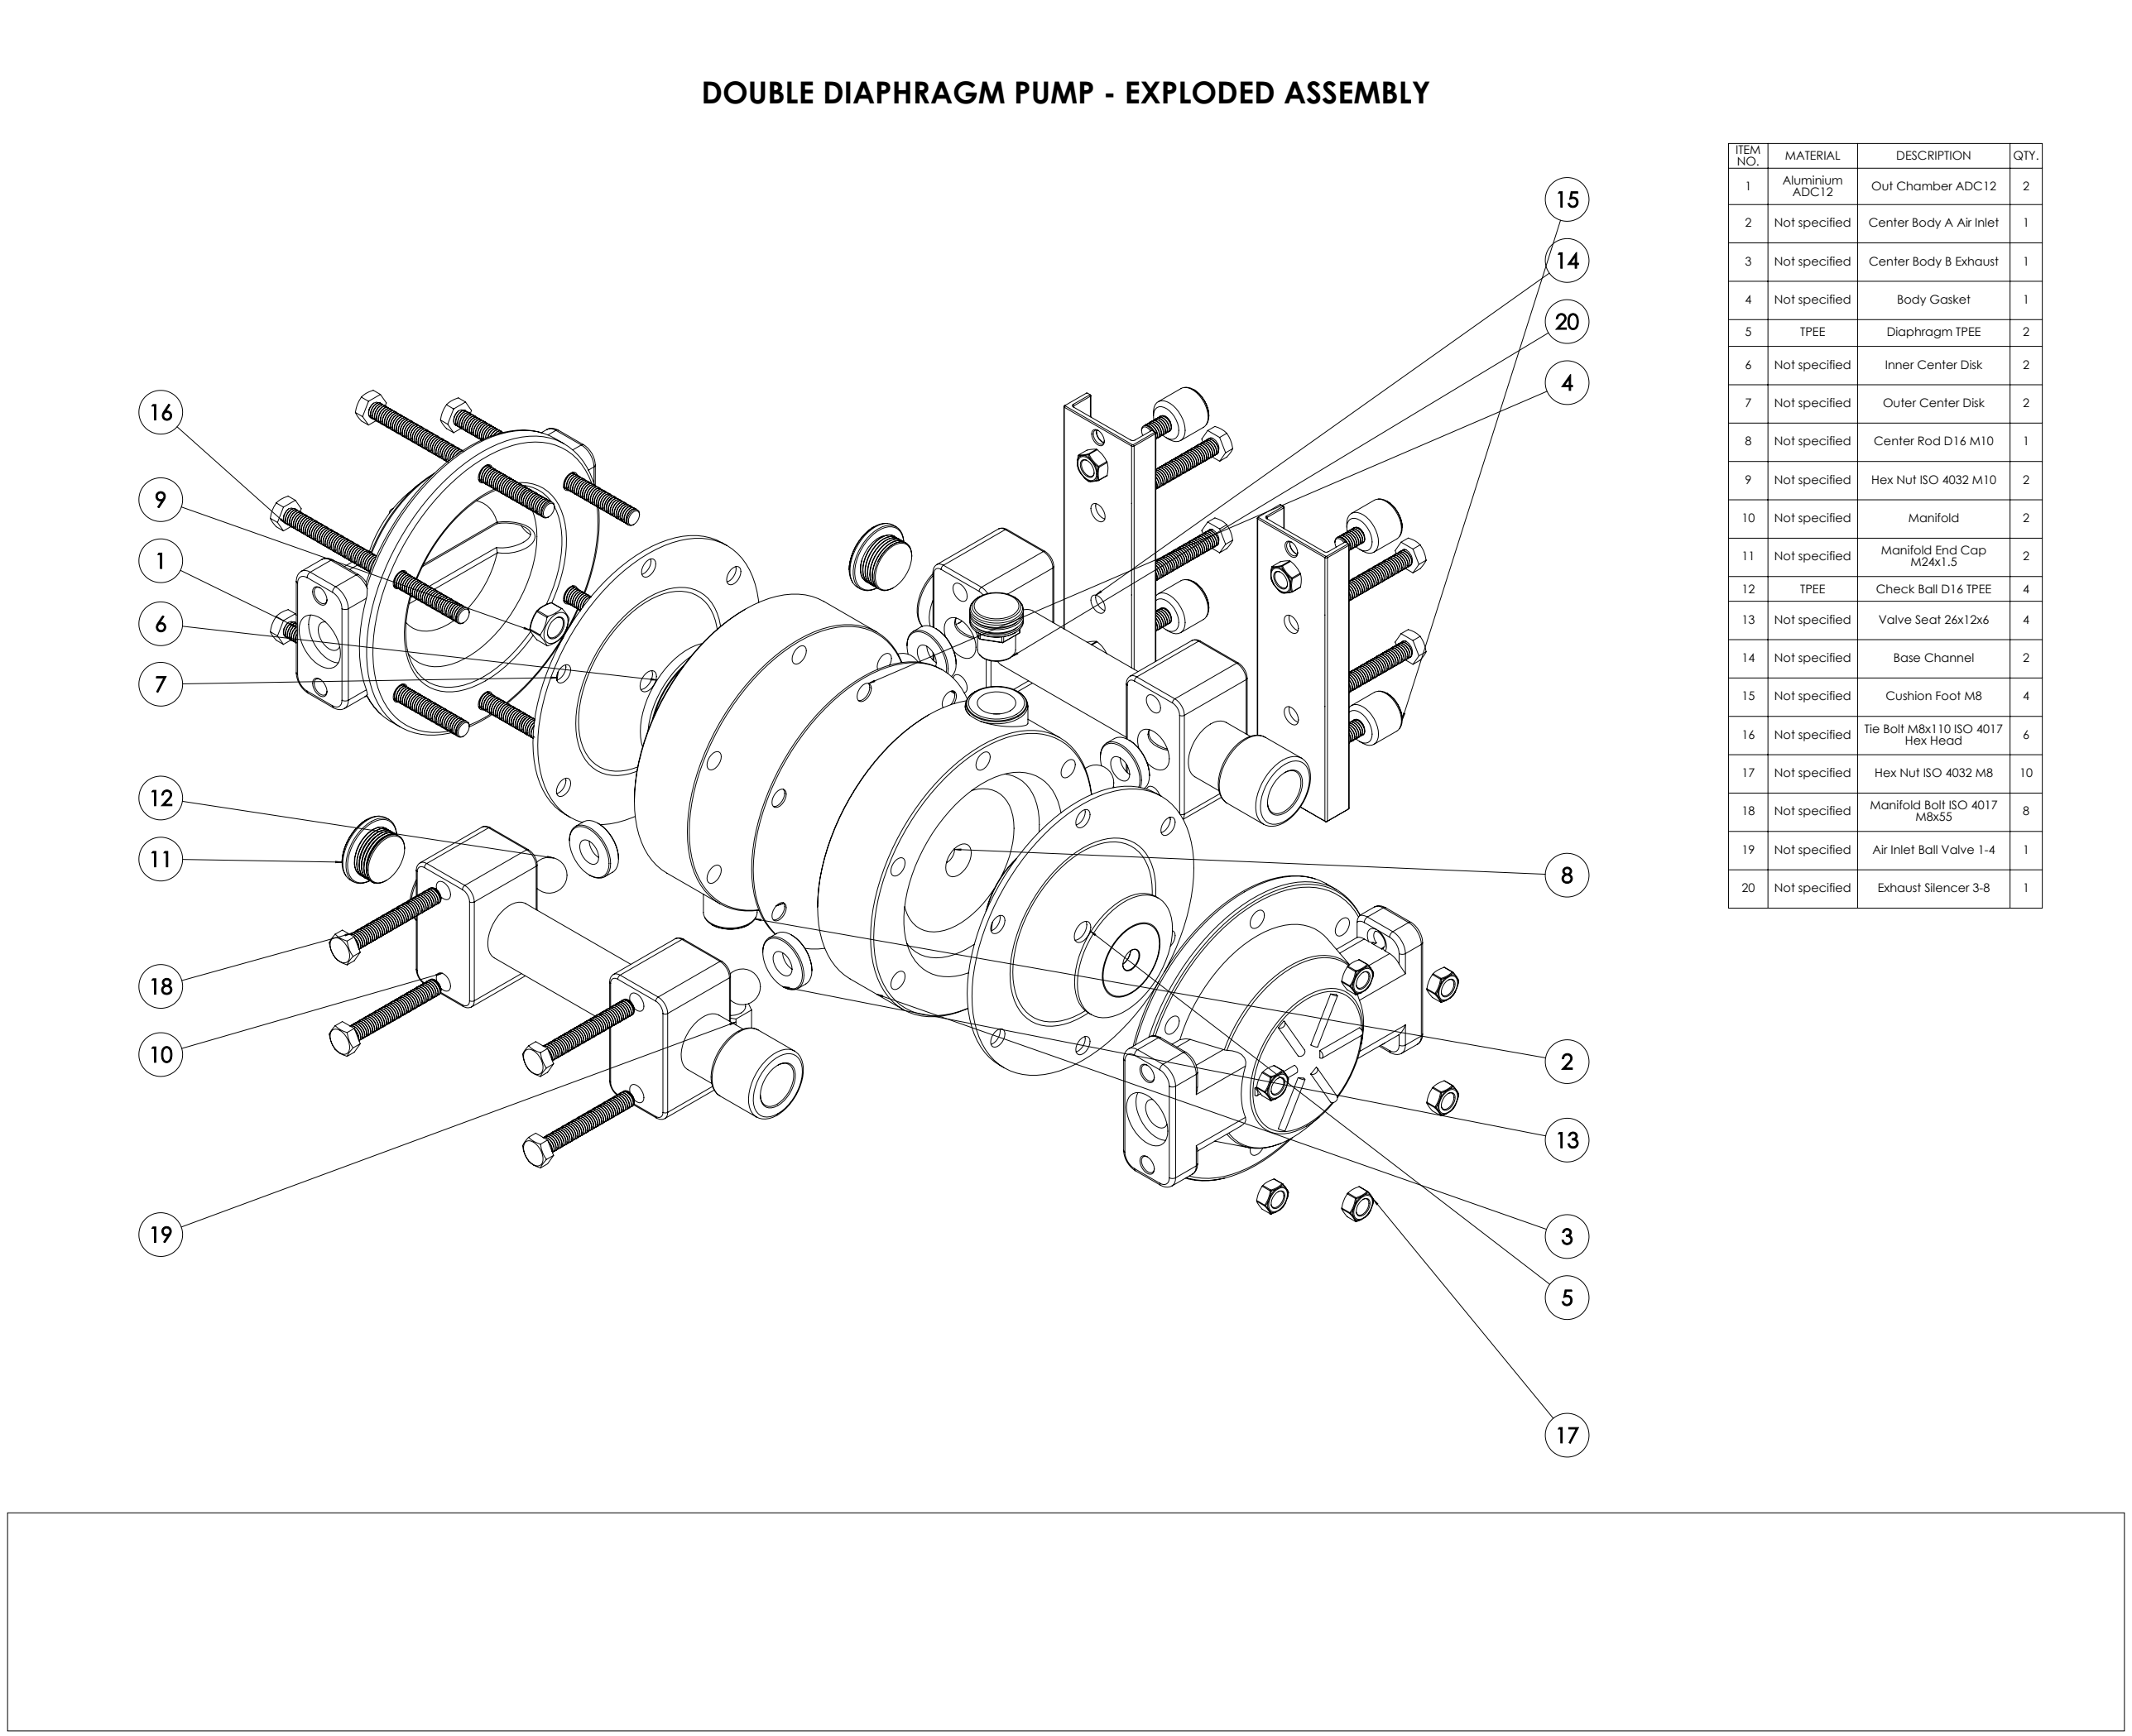
ISO-10303-21;
HEADER;
/* Generated by software containing ST-Developer
 * from STEP Tools, Inc. (www.steptools.com) 
 */

FILE_DESCRIPTION(
/* description */ (''),
/* implementation_level */ '2;1');

FILE_NAME(
/* name */ 'MAS-343',
/* time_stamp */ '2026-10-26T06:13:19-07:00',
/* author */ (''),
/* organization */ (''),
/* preprocessor_version */ 'ST-DEVELOPER v20.2',
/* originating_system */ 'Autodesk Translation Framework v15.15.0.0',
/* authorisation */ '');

FILE_SCHEMA (('AUTOMOTIVE_DESIGN { 1 0 10303 214 3 1 1 }','TECHNICAL_DATA_PACKAGING'));
ENDSEC;

DATA;
#10=MECHANICAL_DESIGN_GEOMETRIC_PRESENTATION_REPRESENTATION('',(#297,#298,
#299,#300,#301,#302,#303,#304,#305,#306,#307,#308,#309,#310,#311,#312,#313,
#314,#315,#316),#56639);
#11=ITEM_DEFINED_TRANSFORMATION($,$,#17191,#18731);
#12=ITEM_DEFINED_TRANSFORMATION($,$,#17191,#18732);
#13=ITEM_DEFINED_TRANSFORMATION($,$,#17485,#18733);
#14=ITEM_DEFINED_TRANSFORMATION($,$,#17536,#18734);
#15=ITEM_DEFINED_TRANSFORMATION($,$,#17588,#18735);
#16=ITEM_DEFINED_TRANSFORMATION($,$,#17615,#18736);
#17=ITEM_DEFINED_TRANSFORMATION($,$,#17615,#18737);
#18=ITEM_DEFINED_TRANSFORMATION($,$,#17650,#18738);
#19=ITEM_DEFINED_TRANSFORMATION($,$,#17650,#18739);
#20=ITEM_DEFINED_TRANSFORMATION($,$,#17664,#18740);
#21=ITEM_DEFINED_TRANSFORMATION($,$,#17664,#18741);
#22=ITEM_DEFINED_TRANSFORMATION($,$,#17684,#18742);
#23=ITEM_DEFINED_TRANSFORMATION($,$,#17774,#18743);
#24=ITEM_DEFINED_TRANSFORMATION($,$,#17774,#18744);
#25=ITEM_DEFINED_TRANSFORMATION($,$,#17818,#18745);
#26=ITEM_DEFINED_TRANSFORMATION($,$,#17818,#18746);
#27=ITEM_DEFINED_TRANSFORMATION($,$,#18010,#18747);
#28=ITEM_DEFINED_TRANSFORMATION($,$,#18010,#18748);
#29=ITEM_DEFINED_TRANSFORMATION($,$,#18066,#18749);
#30=ITEM_DEFINED_TRANSFORMATION($,$,#18137,#18750);
#31=ITEM_DEFINED_TRANSFORMATION($,$,#18202,#18751);
#32=ITEM_DEFINED_TRANSFORMATION($,$,#18202,#18752);
#33=ITEM_DEFINED_TRANSFORMATION($,$,#18205,#18753);
#34=ITEM_DEFINED_TRANSFORMATION($,$,#18205,#18754);
#35=ITEM_DEFINED_TRANSFORMATION($,$,#18218,#18755);
#36=ITEM_DEFINED_TRANSFORMATION($,$,#18327,#18756);
#37=ITEM_DEFINED_TRANSFORMATION($,$,#18687,#18757);
#38=ITEM_DEFINED_TRANSFORMATION($,$,#18327,#18758);
#39=ITEM_DEFINED_TRANSFORMATION($,$,#18687,#18759);
#40=ITEM_DEFINED_TRANSFORMATION($,$,#18375,#18760);
#41=ITEM_DEFINED_TRANSFORMATION($,$,#18375,#18761);
#42=ITEM_DEFINED_TRANSFORMATION($,$,#18375,#18762);
#43=ITEM_DEFINED_TRANSFORMATION($,$,#18375,#18763);
#44=ITEM_DEFINED_TRANSFORMATION($,$,#18202,#18764);
#45=ITEM_DEFINED_TRANSFORMATION($,$,#18202,#18765);
#46=ITEM_DEFINED_TRANSFORMATION($,$,#18205,#18766);
#47=ITEM_DEFINED_TRANSFORMATION($,$,#18205,#18767);
#48=ITEM_DEFINED_TRANSFORMATION($,$,#18218,#18768);
#49=ITEM_DEFINED_TRANSFORMATION($,$,#18327,#18769);
#50=ITEM_DEFINED_TRANSFORMATION($,$,#18687,#18770);
#51=ITEM_DEFINED_TRANSFORMATION($,$,#18327,#18771);
#52=ITEM_DEFINED_TRANSFORMATION($,$,#18687,#18772);
#53=ITEM_DEFINED_TRANSFORMATION($,$,#18375,#18773);
#54=ITEM_DEFINED_TRANSFORMATION($,$,#18375,#18774);
#55=ITEM_DEFINED_TRANSFORMATION($,$,#18375,#18775);
#56=ITEM_DEFINED_TRANSFORMATION($,$,#18375,#18776);
#57=ITEM_DEFINED_TRANSFORMATION($,$,#18487,#18777);
#58=ITEM_DEFINED_TRANSFORMATION($,$,#18687,#18778);
#59=ITEM_DEFINED_TRANSFORMATION($,$,#18487,#18779);
#60=ITEM_DEFINED_TRANSFORMATION($,$,#18687,#18780);
#61=ITEM_DEFINED_TRANSFORMATION($,$,#18487,#18781);
#62=ITEM_DEFINED_TRANSFORMATION($,$,#18687,#18782);
#63=ITEM_DEFINED_TRANSFORMATION($,$,#18487,#18783);
#64=ITEM_DEFINED_TRANSFORMATION($,$,#18687,#18784);
#65=ITEM_DEFINED_TRANSFORMATION($,$,#18487,#18785);
#66=ITEM_DEFINED_TRANSFORMATION($,$,#18687,#18786);
#67=ITEM_DEFINED_TRANSFORMATION($,$,#18487,#18787);
#68=ITEM_DEFINED_TRANSFORMATION($,$,#18687,#18788);
#69=(
REPRESENTATION_RELATIONSHIP($,$,#56745,#56744)
REPRESENTATION_RELATIONSHIP_WITH_TRANSFORMATION(#11)
SHAPE_REPRESENTATION_RELATIONSHIP()
);
#70=(
REPRESENTATION_RELATIONSHIP($,$,#56745,#56744)
REPRESENTATION_RELATIONSHIP_WITH_TRANSFORMATION(#12)
SHAPE_REPRESENTATION_RELATIONSHIP()
);
#71=(
REPRESENTATION_RELATIONSHIP($,$,#56746,#56744)
REPRESENTATION_RELATIONSHIP_WITH_TRANSFORMATION(#13)
SHAPE_REPRESENTATION_RELATIONSHIP()
);
#72=(
REPRESENTATION_RELATIONSHIP($,$,#56747,#56744)
REPRESENTATION_RELATIONSHIP_WITH_TRANSFORMATION(#14)
SHAPE_REPRESENTATION_RELATIONSHIP()
);
#73=(
REPRESENTATION_RELATIONSHIP($,$,#56748,#56744)
REPRESENTATION_RELATIONSHIP_WITH_TRANSFORMATION(#15)
SHAPE_REPRESENTATION_RELATIONSHIP()
);
#74=(
REPRESENTATION_RELATIONSHIP($,$,#56749,#56744)
REPRESENTATION_RELATIONSHIP_WITH_TRANSFORMATION(#16)
SHAPE_REPRESENTATION_RELATIONSHIP()
);
#75=(
REPRESENTATION_RELATIONSHIP($,$,#56749,#56744)
REPRESENTATION_RELATIONSHIP_WITH_TRANSFORMATION(#17)
SHAPE_REPRESENTATION_RELATIONSHIP()
);
#76=(
REPRESENTATION_RELATIONSHIP($,$,#56750,#56744)
REPRESENTATION_RELATIONSHIP_WITH_TRANSFORMATION(#18)
SHAPE_REPRESENTATION_RELATIONSHIP()
);
#77=(
REPRESENTATION_RELATIONSHIP($,$,#56750,#56744)
REPRESENTATION_RELATIONSHIP_WITH_TRANSFORMATION(#19)
SHAPE_REPRESENTATION_RELATIONSHIP()
);
#78=(
REPRESENTATION_RELATIONSHIP($,$,#56751,#56744)
REPRESENTATION_RELATIONSHIP_WITH_TRANSFORMATION(#20)
SHAPE_REPRESENTATION_RELATIONSHIP()
);
#79=(
REPRESENTATION_RELATIONSHIP($,$,#56751,#56744)
REPRESENTATION_RELATIONSHIP_WITH_TRANSFORMATION(#21)
SHAPE_REPRESENTATION_RELATIONSHIP()
);
#80=(
REPRESENTATION_RELATIONSHIP($,$,#56752,#56744)
REPRESENTATION_RELATIONSHIP_WITH_TRANSFORMATION(#22)
SHAPE_REPRESENTATION_RELATIONSHIP()
);
#81=(
REPRESENTATION_RELATIONSHIP($,$,#56753,#56744)
REPRESENTATION_RELATIONSHIP_WITH_TRANSFORMATION(#23)
SHAPE_REPRESENTATION_RELATIONSHIP()
);
#82=(
REPRESENTATION_RELATIONSHIP($,$,#56753,#56744)
REPRESENTATION_RELATIONSHIP_WITH_TRANSFORMATION(#24)
SHAPE_REPRESENTATION_RELATIONSHIP()
);
#83=(
REPRESENTATION_RELATIONSHIP($,$,#56754,#56744)
REPRESENTATION_RELATIONSHIP_WITH_TRANSFORMATION(#25)
SHAPE_REPRESENTATION_RELATIONSHIP()
);
#84=(
REPRESENTATION_RELATIONSHIP($,$,#56754,#56744)
REPRESENTATION_RELATIONSHIP_WITH_TRANSFORMATION(#26)
SHAPE_REPRESENTATION_RELATIONSHIP()
);
#85=(
REPRESENTATION_RELATIONSHIP($,$,#56755,#56744)
REPRESENTATION_RELATIONSHIP_WITH_TRANSFORMATION(#27)
SHAPE_REPRESENTATION_RELATIONSHIP()
);
#86=(
REPRESENTATION_RELATIONSHIP($,$,#56755,#56744)
REPRESENTATION_RELATIONSHIP_WITH_TRANSFORMATION(#28)
SHAPE_REPRESENTATION_RELATIONSHIP()
);
#87=(
REPRESENTATION_RELATIONSHIP($,$,#56756,#56744)
REPRESENTATION_RELATIONSHIP_WITH_TRANSFORMATION(#29)
SHAPE_REPRESENTATION_RELATIONSHIP()
);
#88=(
REPRESENTATION_RELATIONSHIP($,$,#56757,#56744)
REPRESENTATION_RELATIONSHIP_WITH_TRANSFORMATION(#30)
SHAPE_REPRESENTATION_RELATIONSHIP()
);
#89=(
REPRESENTATION_RELATIONSHIP($,$,#56758,#56744)
REPRESENTATION_RELATIONSHIP_WITH_TRANSFORMATION(#31)
SHAPE_REPRESENTATION_RELATIONSHIP()
);
#90=(
REPRESENTATION_RELATIONSHIP($,$,#56758,#56744)
REPRESENTATION_RELATIONSHIP_WITH_TRANSFORMATION(#32)
SHAPE_REPRESENTATION_RELATIONSHIP()
);
#91=(
REPRESENTATION_RELATIONSHIP($,$,#56759,#56744)
REPRESENTATION_RELATIONSHIP_WITH_TRANSFORMATION(#33)
SHAPE_REPRESENTATION_RELATIONSHIP()
);
#92=(
REPRESENTATION_RELATIONSHIP($,$,#56759,#56744)
REPRESENTATION_RELATIONSHIP_WITH_TRANSFORMATION(#34)
SHAPE_REPRESENTATION_RELATIONSHIP()
);
#93=(
REPRESENTATION_RELATIONSHIP($,$,#56760,#56744)
REPRESENTATION_RELATIONSHIP_WITH_TRANSFORMATION(#35)
SHAPE_REPRESENTATION_RELATIONSHIP()
);
#94=(
REPRESENTATION_RELATIONSHIP($,$,#56761,#56744)
REPRESENTATION_RELATIONSHIP_WITH_TRANSFORMATION(#36)
SHAPE_REPRESENTATION_RELATIONSHIP()
);
#95=(
REPRESENTATION_RELATIONSHIP($,$,#56764,#56744)
REPRESENTATION_RELATIONSHIP_WITH_TRANSFORMATION(#37)
SHAPE_REPRESENTATION_RELATIONSHIP()
);
#96=(
REPRESENTATION_RELATIONSHIP($,$,#56761,#56744)
REPRESENTATION_RELATIONSHIP_WITH_TRANSFORMATION(#38)
SHAPE_REPRESENTATION_RELATIONSHIP()
);
#97=(
REPRESENTATION_RELATIONSHIP($,$,#56764,#56744)
REPRESENTATION_RELATIONSHIP_WITH_TRANSFORMATION(#39)
SHAPE_REPRESENTATION_RELATIONSHIP()
);
#98=(
REPRESENTATION_RELATIONSHIP($,$,#56762,#56744)
REPRESENTATION_RELATIONSHIP_WITH_TRANSFORMATION(#40)
SHAPE_REPRESENTATION_RELATIONSHIP()
);
#99=(
REPRESENTATION_RELATIONSHIP($,$,#56762,#56744)
REPRESENTATION_RELATIONSHIP_WITH_TRANSFORMATION(#41)
SHAPE_REPRESENTATION_RELATIONSHIP()
);
#100=(
REPRESENTATION_RELATIONSHIP($,$,#56762,#56744)
REPRESENTATION_RELATIONSHIP_WITH_TRANSFORMATION(#42)
SHAPE_REPRESENTATION_RELATIONSHIP()
);
#101=(
REPRESENTATION_RELATIONSHIP($,$,#56762,#56744)
REPRESENTATION_RELATIONSHIP_WITH_TRANSFORMATION(#43)
SHAPE_REPRESENTATION_RELATIONSHIP()
);
#102=(
REPRESENTATION_RELATIONSHIP($,$,#56758,#56744)
REPRESENTATION_RELATIONSHIP_WITH_TRANSFORMATION(#44)
SHAPE_REPRESENTATION_RELATIONSHIP()
);
#103=(
REPRESENTATION_RELATIONSHIP($,$,#56758,#56744)
REPRESENTATION_RELATIONSHIP_WITH_TRANSFORMATION(#45)
SHAPE_REPRESENTATION_RELATIONSHIP()
);
#104=(
REPRESENTATION_RELATIONSHIP($,$,#56759,#56744)
REPRESENTATION_RELATIONSHIP_WITH_TRANSFORMATION(#46)
SHAPE_REPRESENTATION_RELATIONSHIP()
);
#105=(
REPRESENTATION_RELATIONSHIP($,$,#56759,#56744)
REPRESENTATION_RELATIONSHIP_WITH_TRANSFORMATION(#47)
SHAPE_REPRESENTATION_RELATIONSHIP()
);
#106=(
REPRESENTATION_RELATIONSHIP($,$,#56760,#56744)
REPRESENTATION_RELATIONSHIP_WITH_TRANSFORMATION(#48)
SHAPE_REPRESENTATION_RELATIONSHIP()
);
#107=(
REPRESENTATION_RELATIONSHIP($,$,#56761,#56744)
REPRESENTATION_RELATIONSHIP_WITH_TRANSFORMATION(#49)
SHAPE_REPRESENTATION_RELATIONSHIP()
);
#108=(
REPRESENTATION_RELATIONSHIP($,$,#56764,#56744)
REPRESENTATION_RELATIONSHIP_WITH_TRANSFORMATION(#50)
SHAPE_REPRESENTATION_RELATIONSHIP()
);
#109=(
REPRESENTATION_RELATIONSHIP($,$,#56761,#56744)
REPRESENTATION_RELATIONSHIP_WITH_TRANSFORMATION(#51)
SHAPE_REPRESENTATION_RELATIONSHIP()
);
#110=(
REPRESENTATION_RELATIONSHIP($,$,#56764,#56744)
REPRESENTATION_RELATIONSHIP_WITH_TRANSFORMATION(#52)
SHAPE_REPRESENTATION_RELATIONSHIP()
);
#111=(
REPRESENTATION_RELATIONSHIP($,$,#56762,#56744)
REPRESENTATION_RELATIONSHIP_WITH_TRANSFORMATION(#53)
SHAPE_REPRESENTATION_RELATIONSHIP()
);
#112=(
REPRESENTATION_RELATIONSHIP($,$,#56762,#56744)
REPRESENTATION_RELATIONSHIP_WITH_TRANSFORMATION(#54)
SHAPE_REPRESENTATION_RELATIONSHIP()
);
#113=(
REPRESENTATION_RELATIONSHIP($,$,#56762,#56744)
REPRESENTATION_RELATIONSHIP_WITH_TRANSFORMATION(#55)
SHAPE_REPRESENTATION_RELATIONSHIP()
);
#114=(
REPRESENTATION_RELATIONSHIP($,$,#56762,#56744)
REPRESENTATION_RELATIONSHIP_WITH_TRANSFORMATION(#56)
SHAPE_REPRESENTATION_RELATIONSHIP()
);
#115=(
REPRESENTATION_RELATIONSHIP($,$,#56763,#56744)
REPRESENTATION_RELATIONSHIP_WITH_TRANSFORMATION(#57)
SHAPE_REPRESENTATION_RELATIONSHIP()
);
#116=(
REPRESENTATION_RELATIONSHIP($,$,#56764,#56744)
REPRESENTATION_RELATIONSHIP_WITH_TRANSFORMATION(#58)
SHAPE_REPRESENTATION_RELATIONSHIP()
);
#117=(
REPRESENTATION_RELATIONSHIP($,$,#56763,#56744)
REPRESENTATION_RELATIONSHIP_WITH_TRANSFORMATION(#59)
SHAPE_REPRESENTATION_RELATIONSHIP()
);
#118=(
REPRESENTATION_RELATIONSHIP($,$,#56764,#56744)
REPRESENTATION_RELATIONSHIP_WITH_TRANSFORMATION(#60)
SHAPE_REPRESENTATION_RELATIONSHIP()
);
#119=(
REPRESENTATION_RELATIONSHIP($,$,#56763,#56744)
REPRESENTATION_RELATIONSHIP_WITH_TRANSFORMATION(#61)
SHAPE_REPRESENTATION_RELATIONSHIP()
);
#120=(
REPRESENTATION_RELATIONSHIP($,$,#56764,#56744)
REPRESENTATION_RELATIONSHIP_WITH_TRANSFORMATION(#62)
SHAPE_REPRESENTATION_RELATIONSHIP()
);
#121=(
REPRESENTATION_RELATIONSHIP($,$,#56763,#56744)
REPRESENTATION_RELATIONSHIP_WITH_TRANSFORMATION(#63)
SHAPE_REPRESENTATION_RELATIONSHIP()
);
#122=(
REPRESENTATION_RELATIONSHIP($,$,#56764,#56744)
REPRESENTATION_RELATIONSHIP_WITH_TRANSFORMATION(#64)
SHAPE_REPRESENTATION_RELATIONSHIP()
);
#123=(
REPRESENTATION_RELATIONSHIP($,$,#56763,#56744)
REPRESENTATION_RELATIONSHIP_WITH_TRANSFORMATION(#65)
SHAPE_REPRESENTATION_RELATIONSHIP()
);
#124=(
REPRESENTATION_RELATIONSHIP($,$,#56764,#56744)
REPRESENTATION_RELATIONSHIP_WITH_TRANSFORMATION(#66)
SHAPE_REPRESENTATION_RELATIONSHIP()
);
#125=(
REPRESENTATION_RELATIONSHIP($,$,#56763,#56744)
REPRESENTATION_RELATIONSHIP_WITH_TRANSFORMATION(#67)
SHAPE_REPRESENTATION_RELATIONSHIP()
);
#126=(
REPRESENTATION_RELATIONSHIP($,$,#56764,#56744)
REPRESENTATION_RELATIONSHIP_WITH_TRANSFORMATION(#68)
SHAPE_REPRESENTATION_RELATIONSHIP()
);
#127=CONTEXT_DEPENDENT_SHAPE_REPRESENTATION(#69,#56686);
#128=CONTEXT_DEPENDENT_SHAPE_REPRESENTATION(#70,#56687);
#129=CONTEXT_DEPENDENT_SHAPE_REPRESENTATION(#71,#56688);
#130=CONTEXT_DEPENDENT_SHAPE_REPRESENTATION(#72,#56689);
#131=CONTEXT_DEPENDENT_SHAPE_REPRESENTATION(#73,#56690);
#132=CONTEXT_DEPENDENT_SHAPE_REPRESENTATION(#74,#56691);
#133=CONTEXT_DEPENDENT_SHAPE_REPRESENTATION(#75,#56692);
#134=CONTEXT_DEPENDENT_SHAPE_REPRESENTATION(#76,#56693);
#135=CONTEXT_DEPENDENT_SHAPE_REPRESENTATION(#77,#56694);
#136=CONTEXT_DEPENDENT_SHAPE_REPRESENTATION(#78,#56695);
#137=CONTEXT_DEPENDENT_SHAPE_REPRESENTATION(#79,#56696);
#138=CONTEXT_DEPENDENT_SHAPE_REPRESENTATION(#80,#56697);
#139=CONTEXT_DEPENDENT_SHAPE_REPRESENTATION(#81,#56698);
#140=CONTEXT_DEPENDENT_SHAPE_REPRESENTATION(#82,#56699);
#141=CONTEXT_DEPENDENT_SHAPE_REPRESENTATION(#83,#56700);
#142=CONTEXT_DEPENDENT_SHAPE_REPRESENTATION(#84,#56701);
#143=CONTEXT_DEPENDENT_SHAPE_REPRESENTATION(#85,#56702);
#144=CONTEXT_DEPENDENT_SHAPE_REPRESENTATION(#86,#56703);
#145=CONTEXT_DEPENDENT_SHAPE_REPRESENTATION(#87,#56704);
#146=CONTEXT_DEPENDENT_SHAPE_REPRESENTATION(#88,#56705);
#147=CONTEXT_DEPENDENT_SHAPE_REPRESENTATION(#89,#56706);
#148=CONTEXT_DEPENDENT_SHAPE_REPRESENTATION(#90,#56707);
#149=CONTEXT_DEPENDENT_SHAPE_REPRESENTATION(#91,#56708);
#150=CONTEXT_DEPENDENT_SHAPE_REPRESENTATION(#92,#56709);
#151=CONTEXT_DEPENDENT_SHAPE_REPRESENTATION(#93,#56710);
#152=CONTEXT_DEPENDENT_SHAPE_REPRESENTATION(#94,#56711);
#153=CONTEXT_DEPENDENT_SHAPE_REPRESENTATION(#95,#56712);
#154=CONTEXT_DEPENDENT_SHAPE_REPRESENTATION(#96,#56713);
#155=CONTEXT_DEPENDENT_SHAPE_REPRESENTATION(#97,#56714);
#156=CONTEXT_DEPENDENT_SHAPE_REPRESENTATION(#98,#56715);
#157=CONTEXT_DEPENDENT_SHAPE_REPRESENTATION(#99,#56716);
#158=CONTEXT_DEPENDENT_SHAPE_REPRESENTATION(#100,#56717);
#159=CONTEXT_DEPENDENT_SHAPE_REPRESENTATION(#101,#56718);
#160=CONTEXT_DEPENDENT_SHAPE_REPRESENTATION(#102,#56719);
#161=CONTEXT_DEPENDENT_SHAPE_REPRESENTATION(#103,#56720);
#162=CONTEXT_DEPENDENT_SHAPE_REPRESENTATION(#104,#56721);
#163=CONTEXT_DEPENDENT_SHAPE_REPRESENTATION(#105,#56722);
#164=CONTEXT_DEPENDENT_SHAPE_REPRESENTATION(#106,#56723);
#165=CONTEXT_DEPENDENT_SHAPE_REPRESENTATION(#107,#56724);
#166=CONTEXT_DEPENDENT_SHAPE_REPRESENTATION(#108,#56725);
#167=CONTEXT_DEPENDENT_SHAPE_REPRESENTATION(#109,#56726);
#168=CONTEXT_DEPENDENT_SHAPE_REPRESENTATION(#110,#56727);
#169=CONTEXT_DEPENDENT_SHAPE_REPRESENTATION(#111,#56728);
#170=CONTEXT_DEPENDENT_SHAPE_REPRESENTATION(#112,#56729);
#171=CONTEXT_DEPENDENT_SHAPE_REPRESENTATION(#113,#56730);
#172=CONTEXT_DEPENDENT_SHAPE_REPRESENTATION(#114,#56731);
#173=CONTEXT_DEPENDENT_SHAPE_REPRESENTATION(#115,#56732);
#174=CONTEXT_DEPENDENT_SHAPE_REPRESENTATION(#116,#56733);
#175=CONTEXT_DEPENDENT_SHAPE_REPRESENTATION(#117,#56734);
#176=CONTEXT_DEPENDENT_SHAPE_REPRESENTATION(#118,#56735);
#177=CONTEXT_DEPENDENT_SHAPE_REPRESENTATION(#119,#56736);
#178=CONTEXT_DEPENDENT_SHAPE_REPRESENTATION(#120,#56737);
#179=CONTEXT_DEPENDENT_SHAPE_REPRESENTATION(#121,#56738);
#180=CONTEXT_DEPENDENT_SHAPE_REPRESENTATION(#122,#56739);
#181=CONTEXT_DEPENDENT_SHAPE_REPRESENTATION(#123,#56740);
#182=CONTEXT_DEPENDENT_SHAPE_REPRESENTATION(#124,#56741);
#183=CONTEXT_DEPENDENT_SHAPE_REPRESENTATION(#125,#56742);
#184=CONTEXT_DEPENDENT_SHAPE_REPRESENTATION(#126,#56743);
#185=NEXT_ASSEMBLY_USAGE_OCCURRENCE('01_Out_Chamber_ADC12:2',
'01_Out_Chamber_ADC12:2','01_Out_Chamber_ADC12:2',#56766,#56767,
'01_Out_Chamber_ADC12:2');
#186=NEXT_ASSEMBLY_USAGE_OCCURRENCE('01_Out_Chamber_ADC12:3',
'01_Out_Chamber_ADC12:3','01_Out_Chamber_ADC12:3',#56766,#56767,
'01_Out_Chamber_ADC12:3');
#187=NEXT_ASSEMBLY_USAGE_OCCURRENCE('02_Center_Body_A_Air_Inlet:2',
'02_Center_Body_A_Air_Inlet:2','02_Center_Body_A_Air_Inlet:2',#56766,#56768,
'02_Center_Body_A_Air_Inlet:2');
#188=NEXT_ASSEMBLY_USAGE_OCCURRENCE('03_Center_Body_B_Exhaust:2',
'03_Center_Body_B_Exhaust:2','03_Center_Body_B_Exhaust:2',#56766,#56769,
'03_Center_Body_B_Exhaust:2');
#189=NEXT_ASSEMBLY_USAGE_OCCURRENCE('04_Body_Gasket:2',
'04_Body_Gasket:2','04_Body_Gasket:2',#56766,#56770,'04_Body_Gasket:2');
#190=NEXT_ASSEMBLY_USAGE_OCCURRENCE('05_Diaphragm_TPEE:2',
'05_Diaphragm_TPEE:2','05_Diaphragm_TPEE:2',#56766,#56771,
'05_Diaphragm_TPEE:2');
#191=NEXT_ASSEMBLY_USAGE_OCCURRENCE('05_Diaphragm_TPEE:3',
'05_Diaphragm_TPEE:3','05_Diaphragm_TPEE:3',#56766,#56771,
'05_Diaphragm_TPEE:3');
#192=NEXT_ASSEMBLY_USAGE_OCCURRENCE('06_Inner_Center_Disk:2',
'06_Inner_Center_Disk:2','06_Inner_Center_Disk:2',#56766,#56772,
'06_Inner_Center_Disk:2');
#193=NEXT_ASSEMBLY_USAGE_OCCURRENCE('06_Inner_Center_Disk:3',
'06_Inner_Center_Disk:3','06_Inner_Center_Disk:3',#56766,#56772,
'06_Inner_Center_Disk:3');
#194=NEXT_ASSEMBLY_USAGE_OCCURRENCE('07_Outer_Center_Disk:2',
'07_Outer_Center_Disk:2','07_Outer_Center_Disk:2',#56766,#56773,
'07_Outer_Center_Disk:2');
#195=NEXT_ASSEMBLY_USAGE_OCCURRENCE('07_Outer_Center_Disk:3',
'07_Outer_Center_Disk:3','07_Outer_Center_Disk:3',#56766,#56773,
'07_Outer_Center_Disk:3');
#196=NEXT_ASSEMBLY_USAGE_OCCURRENCE('08_Center_Rod_D16_M10:2',
'08_Center_Rod_D16_M10:2','08_Center_Rod_D16_M10:2',#56766,#56774,
'08_Center_Rod_D16_M10:2');
#197=NEXT_ASSEMBLY_USAGE_OCCURRENCE('09_Hex_Nut_ISO_4032_M10:2',
'09_Hex_Nut_ISO_4032_M10:2','09_Hex_Nut_ISO_4032_M10:2',#56766,#56775,
'09_Hex_Nut_ISO_4032_M10:2');
#198=NEXT_ASSEMBLY_USAGE_OCCURRENCE('09_Hex_Nut_ISO_4032_M10:3',
'09_Hex_Nut_ISO_4032_M10:3','09_Hex_Nut_ISO_4032_M10:3',#56766,#56775,
'09_Hex_Nut_ISO_4032_M10:3');
#199=NEXT_ASSEMBLY_USAGE_OCCURRENCE('10_Manifold:2','10_Manifold:2',
'10_Manifold:2',#56766,#56776,'10_Manifold:2');
#200=NEXT_ASSEMBLY_USAGE_OCCURRENCE('10_Manifold:3','10_Manifold:3',
'10_Manifold:3',#56766,#56776,'10_Manifold:3');
#201=NEXT_ASSEMBLY_USAGE_OCCURRENCE('11_Manifold_End_Cap_M24x1.5:2',
'11_Manifold_End_Cap_M24x1.5:2','11_Manifold_End_Cap_M24x1.5:2',#56766,
#56777,'11_Manifold_End_Cap_M24x1.5:2');
#202=NEXT_ASSEMBLY_USAGE_OCCURRENCE('11_Manifold_End_Cap_M24x1.5:3',
'11_Manifold_End_Cap_M24x1.5:3','11_Manifold_End_Cap_M24x1.5:3',#56766,
#56777,'11_Manifold_End_Cap_M24x1.5:3');
#203=NEXT_ASSEMBLY_USAGE_OCCURRENCE('19_Air_Inlet_Ball_Valve_1-4:2',
'19_Air_Inlet_Ball_Valve_1-4:2','19_Air_Inlet_Ball_Valve_1-4:2',#56766,
#56778,'19_Air_Inlet_Ball_Valve_1-4:2');
#204=NEXT_ASSEMBLY_USAGE_OCCURRENCE('20_Exhaust_Silencer_3-8:2',
'20_Exhaust_Silencer_3-8:2','20_Exhaust_Silencer_3-8:2',#56766,#56779,
'20_Exhaust_Silencer_3-8:2');
#205=NEXT_ASSEMBLY_USAGE_OCCURRENCE('12_Check_Ball_D16_TPEE:2',
'12_Check_Ball_D16_TPEE:2','12_Check_Ball_D16_TPEE:2',#56766,#56780,
'12_Check_Ball_D16_TPEE:2');
#206=NEXT_ASSEMBLY_USAGE_OCCURRENCE('12_Check_Ball_D16_TPEE:3',
'12_Check_Ball_D16_TPEE:3','12_Check_Ball_D16_TPEE:3',#56766,#56780,
'12_Check_Ball_D16_TPEE:3');
#207=NEXT_ASSEMBLY_USAGE_OCCURRENCE('13_Valve_Seat_26x12x6:2',
'13_Valve_Seat_26x12x6:2','13_Valve_Seat_26x12x6:2',#56766,#56781,
'13_Valve_Seat_26x12x6:2');
#208=NEXT_ASSEMBLY_USAGE_OCCURRENCE('13_Valve_Seat_26x12x6:3',
'13_Valve_Seat_26x12x6:3','13_Valve_Seat_26x12x6:3',#56766,#56781,
'13_Valve_Seat_26x12x6:3');
#209=NEXT_ASSEMBLY_USAGE_OCCURRENCE('14_Base_Channel:2',
'14_Base_Channel:2','14_Base_Channel:2',#56766,#56782,
'14_Base_Channel:2');
#210=NEXT_ASSEMBLY_USAGE_OCCURRENCE('15_Cushion_Foot_M8:2',
'15_Cushion_Foot_M8:2','15_Cushion_Foot_M8:2',#56766,#56783,
'15_Cushion_Foot_M8:2');
#211=NEXT_ASSEMBLY_USAGE_OCCURRENCE('17_Hex_Nut_ISO_4032_M8:2',
'17_Hex_Nut_ISO_4032_M8:2','17_Hex_Nut_ISO_4032_M8:2',#56766,#56786,
'17_Hex_Nut_ISO_4032_M8:2');
#212=NEXT_ASSEMBLY_USAGE_OCCURRENCE('15_Cushion_Foot_M8:3',
'15_Cushion_Foot_M8:3','15_Cushion_Foot_M8:3',#56766,#56783,
'15_Cushion_Foot_M8:3');
#213=NEXT_ASSEMBLY_USAGE_OCCURRENCE('17_Hex_Nut_ISO_4032_M8:3',
'17_Hex_Nut_ISO_4032_M8:3','17_Hex_Nut_ISO_4032_M8:3',#56766,#56786,
'17_Hex_Nut_ISO_4032_M8:3');
#214=NEXT_ASSEMBLY_USAGE_OCCURRENCE('18_Manifold_Bolt_ISO_4017_M8x55:2',
'18_Manifold_Bolt_ISO_4017_M8x55:2','18_Manifold_Bolt_ISO_4017_M8x55:2',
#56766,#56784,'18_Manifold_Bolt_ISO_4017_M8x55:2');
#215=NEXT_ASSEMBLY_USAGE_OCCURRENCE('18_Manifold_Bolt_ISO_4017_M8x55:3',
'18_Manifold_Bolt_ISO_4017_M8x55:3','18_Manifold_Bolt_ISO_4017_M8x55:3',
#56766,#56784,'18_Manifold_Bolt_ISO_4017_M8x55:3');
#216=NEXT_ASSEMBLY_USAGE_OCCURRENCE('18_Manifold_Bolt_ISO_4017_M8x55:4',
'18_Manifold_Bolt_ISO_4017_M8x55:4','18_Manifold_Bolt_ISO_4017_M8x55:4',
#56766,#56784,'18_Manifold_Bolt_ISO_4017_M8x55:4');
#217=NEXT_ASSEMBLY_USAGE_OCCURRENCE('18_Manifold_Bolt_ISO_4017_M8x55:5',
'18_Manifold_Bolt_ISO_4017_M8x55:5','18_Manifold_Bolt_ISO_4017_M8x55:5',
#56766,#56784,'18_Manifold_Bolt_ISO_4017_M8x55:5');
#218=NEXT_ASSEMBLY_USAGE_OCCURRENCE('12_Check_Ball_D16_TPEE:4',
'12_Check_Ball_D16_TPEE:4','12_Check_Ball_D16_TPEE:4',#56766,#56780,
'12_Check_Ball_D16_TPEE:4');
#219=NEXT_ASSEMBLY_USAGE_OCCURRENCE('12_Check_Ball_D16_TPEE:5',
'12_Check_Ball_D16_TPEE:5','12_Check_Ball_D16_TPEE:5',#56766,#56780,
'12_Check_Ball_D16_TPEE:5');
#220=NEXT_ASSEMBLY_USAGE_OCCURRENCE('13_Valve_Seat_26x12x6:4',
'13_Valve_Seat_26x12x6:4','13_Valve_Seat_26x12x6:4',#56766,#56781,
'13_Valve_Seat_26x12x6:4');
#221=NEXT_ASSEMBLY_USAGE_OCCURRENCE('13_Valve_Seat_26x12x6:5',
'13_Valve_Seat_26x12x6:5','13_Valve_Seat_26x12x6:5',#56766,#56781,
'13_Valve_Seat_26x12x6:5');
#222=NEXT_ASSEMBLY_USAGE_OCCURRENCE('14_Base_Channel:3',
'14_Base_Channel:3','14_Base_Channel:3',#56766,#56782,
'14_Base_Channel:3');
#223=NEXT_ASSEMBLY_USAGE_OCCURRENCE('15_Cushion_Foot_M8:4',
'15_Cushion_Foot_M8:4','15_Cushion_Foot_M8:4',#56766,#56783,
'15_Cushion_Foot_M8:4');
#224=NEXT_ASSEMBLY_USAGE_OCCURRENCE('17_Hex_Nut_ISO_4032_M8:4',
'17_Hex_Nut_ISO_4032_M8:4','17_Hex_Nut_ISO_4032_M8:4',#56766,#56786,
'17_Hex_Nut_ISO_4032_M8:4');
#225=NEXT_ASSEMBLY_USAGE_OCCURRENCE('15_Cushion_Foot_M8:5',
'15_Cushion_Foot_M8:5','15_Cushion_Foot_M8:5',#56766,#56783,
'15_Cushion_Foot_M8:5');
#226=NEXT_ASSEMBLY_USAGE_OCCURRENCE('17_Hex_Nut_ISO_4032_M8:5',
'17_Hex_Nut_ISO_4032_M8:5','17_Hex_Nut_ISO_4032_M8:5',#56766,#56786,
'17_Hex_Nut_ISO_4032_M8:5');
#227=NEXT_ASSEMBLY_USAGE_OCCURRENCE('18_Manifold_Bolt_ISO_4017_M8x55:6',
'18_Manifold_Bolt_ISO_4017_M8x55:6','18_Manifold_Bolt_ISO_4017_M8x55:6',
#56766,#56784,'18_Manifold_Bolt_ISO_4017_M8x55:6');
#228=NEXT_ASSEMBLY_USAGE_OCCURRENCE('18_Manifold_Bolt_ISO_4017_M8x55:7',
'18_Manifold_Bolt_ISO_4017_M8x55:7','18_Manifold_Bolt_ISO_4017_M8x55:7',
#56766,#56784,'18_Manifold_Bolt_ISO_4017_M8x55:7');
#229=NEXT_ASSEMBLY_USAGE_OCCURRENCE('18_Manifold_Bolt_ISO_4017_M8x55:8',
'18_Manifold_Bolt_ISO_4017_M8x55:8','18_Manifold_Bolt_ISO_4017_M8x55:8',
#56766,#56784,'18_Manifold_Bolt_ISO_4017_M8x55:8');
#230=NEXT_ASSEMBLY_USAGE_OCCURRENCE('18_Manifold_Bolt_ISO_4017_M8x55:9',
'18_Manifold_Bolt_ISO_4017_M8x55:9','18_Manifold_Bolt_ISO_4017_M8x55:9',
#56766,#56784,'18_Manifold_Bolt_ISO_4017_M8x55:9');
#231=NEXT_ASSEMBLY_USAGE_OCCURRENCE(
'16_Tie_Bolt_M8x110_ISO_4017_Hex_Head:2',
'16_Tie_Bolt_M8x110_ISO_4017_Hex_Head:2',
'16_Tie_Bolt_M8x110_ISO_4017_Hex_Head:2',#56766,#56785,
'16_Tie_Bolt_M8x110_ISO_4017_Hex_Head:2');
#232=NEXT_ASSEMBLY_USAGE_OCCURRENCE('17_Hex_Nut_ISO_4032_M8:6',
'17_Hex_Nut_ISO_4032_M8:6','17_Hex_Nut_ISO_4032_M8:6',#56766,#56786,
'17_Hex_Nut_ISO_4032_M8:6');
#233=NEXT_ASSEMBLY_USAGE_OCCURRENCE(
'16_Tie_Bolt_M8x110_ISO_4017_Hex_Head:3',
'16_Tie_Bolt_M8x110_ISO_4017_Hex_Head:3',
'16_Tie_Bolt_M8x110_ISO_4017_Hex_Head:3',#56766,#56785,
'16_Tie_Bolt_M8x110_ISO_4017_Hex_Head:3');
#234=NEXT_ASSEMBLY_USAGE_OCCURRENCE('17_Hex_Nut_ISO_4032_M8:7',
'17_Hex_Nut_ISO_4032_M8:7','17_Hex_Nut_ISO_4032_M8:7',#56766,#56786,
'17_Hex_Nut_ISO_4032_M8:7');
#235=NEXT_ASSEMBLY_USAGE_OCCURRENCE(
'16_Tie_Bolt_M8x110_ISO_4017_Hex_Head:4',
'16_Tie_Bolt_M8x110_ISO_4017_Hex_Head:4',
'16_Tie_Bolt_M8x110_ISO_4017_Hex_Head:4',#56766,#56785,
'16_Tie_Bolt_M8x110_ISO_4017_Hex_Head:4');
#236=NEXT_ASSEMBLY_USAGE_OCCURRENCE('17_Hex_Nut_ISO_4032_M8:8',
'17_Hex_Nut_ISO_4032_M8:8','17_Hex_Nut_ISO_4032_M8:8',#56766,#56786,
'17_Hex_Nut_ISO_4032_M8:8');
#237=NEXT_ASSEMBLY_USAGE_OCCURRENCE(
'16_Tie_Bolt_M8x110_ISO_4017_Hex_Head:5',
'16_Tie_Bolt_M8x110_ISO_4017_Hex_Head:5',
'16_Tie_Bolt_M8x110_ISO_4017_Hex_Head:5',#56766,#56785,
'16_Tie_Bolt_M8x110_ISO_4017_Hex_Head:5');
#238=NEXT_ASSEMBLY_USAGE_OCCURRENCE('17_Hex_Nut_ISO_4032_M8:9',
'17_Hex_Nut_ISO_4032_M8:9','17_Hex_Nut_ISO_4032_M8:9',#56766,#56786,
'17_Hex_Nut_ISO_4032_M8:9');
#239=NEXT_ASSEMBLY_USAGE_OCCURRENCE(
'16_Tie_Bolt_M8x110_ISO_4017_Hex_Head:6',
'16_Tie_Bolt_M8x110_ISO_4017_Hex_Head:6',
'16_Tie_Bolt_M8x110_ISO_4017_Hex_Head:6',#56766,#56785,
'16_Tie_Bolt_M8x110_ISO_4017_Hex_Head:6');
#240=NEXT_ASSEMBLY_USAGE_OCCURRENCE('17_Hex_Nut_ISO_4032_M8:10',
'17_Hex_Nut_ISO_4032_M8:10','17_Hex_Nut_ISO_4032_M8:10',#56766,#56786,
'17_Hex_Nut_ISO_4032_M8:10');
#241=NEXT_ASSEMBLY_USAGE_OCCURRENCE(
'16_Tie_Bolt_M8x110_ISO_4017_Hex_Head:7',
'16_Tie_Bolt_M8x110_ISO_4017_Hex_Head:7',
'16_Tie_Bolt_M8x110_ISO_4017_Hex_Head:7',#56766,#56785,
'16_Tie_Bolt_M8x110_ISO_4017_Hex_Head:7');
#242=NEXT_ASSEMBLY_USAGE_OCCURRENCE('17_Hex_Nut_ISO_4032_M8:11',
'17_Hex_Nut_ISO_4032_M8:11','17_Hex_Nut_ISO_4032_M8:11',#56766,#56786,
'17_Hex_Nut_ISO_4032_M8:11');
#243=SPHERICAL_SURFACE('',#18203,8.);
#244=ELLIPSE('',#17827,15.2397506541282,10.);
#245=ELLIPSE('',#17828,15.2397506541282,10.);
#246=ELLIPSE('',#17829,15.2397506541282,10.);
#247=ELLIPSE('',#17830,15.2397506541282,10.);
#248=ELLIPSE('',#17989,15.2397506541282,10.);
#249=ELLIPSE('',#17990,15.2397506541282,10.);
#250=ELLIPSE('',#17991,15.2397506541282,10.);
#251=ELLIPSE('',#17992,15.2397506541282,10.);
#252=ELLIPSE('',#17993,15.2397506541282,10.);
#253=ELLIPSE('',#17994,15.2397506541282,10.);
#254=ELLIPSE('',#18087,3.46410161513776,3.);
#255=ELLIPSE('',#18088,3.46410161513776,3.);
#256=ELLIPSE('',#18089,3.46410161513776,3.);
#257=SHAPE_REPRESENTATION_RELATIONSHIP('SRR','None',#56745,#277);
#258=SHAPE_REPRESENTATION_RELATIONSHIP('SRR','None',#56746,#278);
#259=SHAPE_REPRESENTATION_RELATIONSHIP('SRR','None',#56747,#279);
#260=SHAPE_REPRESENTATION_RELATIONSHIP('SRR','None',#56748,#280);
#261=SHAPE_REPRESENTATION_RELATIONSHIP('SRR','None',#56749,#281);
#262=SHAPE_REPRESENTATION_RELATIONSHIP('SRR','None',#56750,#282);
#263=SHAPE_REPRESENTATION_RELATIONSHIP('SRR','None',#56751,#283);
#264=SHAPE_REPRESENTATION_RELATIONSHIP('SRR','None',#56752,#284);
#265=SHAPE_REPRESENTATION_RELATIONSHIP('SRR','None',#56753,#285);
#266=SHAPE_REPRESENTATION_RELATIONSHIP('SRR','None',#56754,#286);
#267=SHAPE_REPRESENTATION_RELATIONSHIP('SRR','None',#56755,#287);
#268=SHAPE_REPRESENTATION_RELATIONSHIP('SRR','None',#56756,#288);
#269=SHAPE_REPRESENTATION_RELATIONSHIP('SRR','None',#56757,#289);
#270=SHAPE_REPRESENTATION_RELATIONSHIP('SRR','None',#56758,#290);
#271=SHAPE_REPRESENTATION_RELATIONSHIP('SRR','None',#56759,#291);
#272=SHAPE_REPRESENTATION_RELATIONSHIP('SRR','None',#56760,#292);
#273=SHAPE_REPRESENTATION_RELATIONSHIP('SRR','None',#56761,#293);
#274=SHAPE_REPRESENTATION_RELATIONSHIP('SRR','None',#56762,#294);
#275=SHAPE_REPRESENTATION_RELATIONSHIP('SRR','None',#56763,#295);
#276=SHAPE_REPRESENTATION_RELATIONSHIP('SRR','None',#56764,#296);
#277=ADVANCED_BREP_SHAPE_REPRESENTATION('',(#317),#56619);
#278=ADVANCED_BREP_SHAPE_REPRESENTATION('',(#318),#56620);
#279=ADVANCED_BREP_SHAPE_REPRESENTATION('',(#319),#56621);
#280=ADVANCED_BREP_SHAPE_REPRESENTATION('',(#320),#56622);
#281=ADVANCED_BREP_SHAPE_REPRESENTATION('',(#321),#56623);
#282=ADVANCED_BREP_SHAPE_REPRESENTATION('',(#322),#56624);
#283=ADVANCED_BREP_SHAPE_REPRESENTATION('',(#323),#56625);
#284=ADVANCED_BREP_SHAPE_REPRESENTATION('',(#324),#56626);
#285=ADVANCED_BREP_SHAPE_REPRESENTATION('',(#325),#56627);
#286=ADVANCED_BREP_SHAPE_REPRESENTATION('',(#326),#56628);
#287=ADVANCED_BREP_SHAPE_REPRESENTATION('',(#327),#56629);
#288=ADVANCED_BREP_SHAPE_REPRESENTATION('',(#328),#56630);
#289=ADVANCED_BREP_SHAPE_REPRESENTATION('',(#329),#56631);
#290=ADVANCED_BREP_SHAPE_REPRESENTATION('',(#330),#56632);
#291=ADVANCED_BREP_SHAPE_REPRESENTATION('',(#331),#56633);
#292=ADVANCED_BREP_SHAPE_REPRESENTATION('',(#332),#56634);
#293=ADVANCED_BREP_SHAPE_REPRESENTATION('',(#333),#56635);
#294=ADVANCED_BREP_SHAPE_REPRESENTATION('',(#334),#56636);
#295=ADVANCED_BREP_SHAPE_REPRESENTATION('',(#335),#56637);
#296=ADVANCED_BREP_SHAPE_REPRESENTATION('',(#336),#56638);
#297=STYLED_ITEM('',(#56908),#317);
#298=STYLED_ITEM('',(#56894),#318);
#299=STYLED_ITEM('',(#56894),#319);
#300=STYLED_ITEM('',(#56894),#320);
#301=STYLED_ITEM('',(#56901),#321);
#302=STYLED_ITEM('',(#56929),#322);
#303=STYLED_ITEM('',(#56908),#323);
#304=STYLED_ITEM('',(#56915),#324);
#305=STYLED_ITEM('',(#56922),#325);
#306=STYLED_ITEM('',(#56929),#326);
#307=STYLED_ITEM('',(#56901),#327);
#308=STYLED_ITEM('',(#56929),#328);
#309=STYLED_ITEM('',(#56901),#329);
#310=STYLED_ITEM('',(#56908),#330);
#311=STYLED_ITEM('',(#56908),#331);
#312=STYLED_ITEM('',(#56894),#332);
#313=STYLED_ITEM('',(#56929),#333);
#314=STYLED_ITEM('',(#56922),#334);
#315=STYLED_ITEM('',(#56922),#335);
#316=STYLED_ITEM('',(#56922),#336);
#317=MANIFOLD_SOLID_BREP('Body1',#16949);
#318=MANIFOLD_SOLID_BREP('Body1',#16950);
#319=MANIFOLD_SOLID_BREP('Body1',#16951);
#320=MANIFOLD_SOLID_BREP('Body1',#16952);
#321=MANIFOLD_SOLID_BREP('Body1',#16953);
#322=MANIFOLD_SOLID_BREP('Body1',#16954);
#323=MANIFOLD_SOLID_BREP('Body1',#16955);
#324=MANIFOLD_SOLID_BREP('Body1',#16956);
#325=MANIFOLD_SOLID_BREP('Body1',#16957);
#326=MANIFOLD_SOLID_BREP('Body1',#16958);
#327=MANIFOLD_SOLID_BREP('Body1',#16959);
#328=MANIFOLD_SOLID_BREP('Body1',#16960);
#329=MANIFOLD_SOLID_BREP('Body1',#16961);
#330=MANIFOLD_SOLID_BREP('Body1',#16962);
#331=MANIFOLD_SOLID_BREP('Body1',#16963);
#332=MANIFOLD_SOLID_BREP('Body1',#16964);
#333=MANIFOLD_SOLID_BREP('Body1',#16965);
#334=MANIFOLD_SOLID_BREP('Body1',#16966);
#335=MANIFOLD_SOLID_BREP('Body1',#16967);
#336=MANIFOLD_SOLID_BREP('Body1',#16968);
#337=B_SPLINE_SURFACE_WITH_KNOTS('',3,3,((#23722,#23723,#23724,#23725,#23726,
#23727,#23728,#23729,#23730,#23731,#23732,#23733,#23734,#23735),(#23736,
#23737,#23738,#23739,#23740,#23741,#23742,#23743,#23744,#23745,#23746,#23747,
#23748,#23749),(#23750,#23751,#23752,#23753,#23754,#23755,#23756,#23757,
#23758,#23759,#23760,#23761,#23762,#23763),(#23764,#23765,#23766,#23767,
#23768,#23769,#23770,#23771,#23772,#23773,#23774,#23775,#23776,#23777),
(#23778,#23779,#23780,#23781,#23782,#23783,#23784,#23785,#23786,#23787,
#23788,#23789,#23790,#23791),(#23792,#23793,#23794,#23795,#23796,#23797,
#23798,#23799,#23800,#23801,#23802,#23803,#23804,#23805),(#23806,#23807,
#23808,#23809,#23810,#23811,#23812,#23813,#23814,#23815,#23816,#23817,#23818,
#23819)),.UNSPECIFIED.,.F.,.F.,.F.,(4,1,1,1,4),(4,1,1,1,1,1,1,1,1,1,1,4),
(0.,0.285714285714286,0.571428571428571,0.785714285714286,1.),(4.69190485072485,
5.32399487973813,5.95608490875141,6.27212992325805,6.58817493776469,6.79887161410245,
7.00956829044021,7.22026496677797,7.43096164311573,7.85235499579125,8.48444502480452,
9.1165350538178),.UNSPECIFIED.);
#338=B_SPLINE_SURFACE_WITH_KNOTS('',3,3,((#24134,#24135,#24136,#24137,#24138,
#24139,#24140,#24141,#24142,#24143,#24144,#24145,#24146,#24147,#24148),
(#24149,#24150,#24151,#24152,#24153,#24154,#24155,#24156,#24157,#24158,
#24159,#24160,#24161,#24162,#24163),(#24164,#24165,#24166,#24167,#24168,
#24169,#24170,#24171,#24172,#24173,#24174,#24175,#24176,#24177,#24178),
(#24179,#24180,#24181,#24182,#24183,#24184,#24185,#24186,#24187,#24188,
#24189,#24190,#24191,#24192,#24193),(#24194,#24195,#24196,#24197,#24198,
#24199,#24200,#24201,#24202,#24203,#24204,#24205,#24206,#24207,#24208),
(#24209,#24210,#24211,#24212,#24213,#24214,#24215,#24216,#24217,#24218,
#24219,#24220,#24221,#24222,#24223),(#24224,#24225,#24226,#24227,#24228,
#24229,#24230,#24231,#24232,#24233,#24234,#24235,#24236,#24237,#24238)),
 .UNSPECIFIED.,.F.,.F.,.F.,(4,1,1,1,4),(4,1,1,1,1,1,1,1,1,1,1,1,4),(0.,
0.285714285714286,0.571428571428571,0.785714285714286,1.),(4.69190485072485,
5.32399487973813,5.95608490875141,6.27212992325805,6.58817493776469,6.79887161410245,
7.00956829044021,7.22026496677796,7.43096164311572,7.64165831945348,7.85235499579124,
8.48444502480452,9.1165350538178),.UNSPECIFIED.);
#339=B_SPLINE_SURFACE_WITH_KNOTS('',3,3,((#28895,#28896,#28897,#28898,#28899,
#28900,#28901,#28902,#28903,#28904,#28905,#28906,#28907,#28908,#28909,#28910,
#28911,#28912,#28913,#28914,#28915,#28916,#28917,#28918,#28919,#28920,#28921,
#28922,#28923,#28924,#28925,#28926,#28927,#28928,#28929,#28930,#28931,#28932,
#28933,#28934,#28935,#28936,#28937,#28938,#28939,#28940,#28941,#28942,#28943,
#28944,#28945,#28946,#28947,#28948,#28949,#28950,#28951,#28952,#28953,#28954,
#28955,#28956,#28957,#28958,#28959,#28960,#28961,#28962,#28963,#28964,#28965,
#28966,#28967,#28968,#28969,#28970,#28971,#28972,#28973,#28974,#28975,#28976,
#28977,#28978,#28979,#28980,#28981,#28982,#28983,#28984,#28985,#28986,#28987,
#28988,#28989,#28990,#28991,#28992,#28993,#28994,#28995,#28996,#28997,#28998,
#28999,#29000,#29001,#29002,#29003,#29004,#29005,#29006,#29007,#29008,#29009,
#29010,#29011,#29012,#29013,#29014,#29015,#29016,#29017,#29018,#29019,#29020,
#29021,#29022,#29023,#29024,#29025,#29026,#29027,#29028,#29029,#29030,#29031,
#29032,#29033,#29034,#29035,#29036,#29037,#29038,#29039,#29040,#29041,#29042,
#29043,#29044,#29045,#29046,#29047,#29048,#29049,#29050,#29051,#29052,#29053,
#29054,#29055,#29056,#29057,#29058,#29059,#29060,#29061,#29062,#29063,#29064,
#29065,#29066,#29067,#29068,#29069,#29070,#29071,#29072,#29073,#29074,#29075,
#29076,#29077,#29078,#29079,#29080,#29081,#29082,#29083,#29084,#29085,#29086,
#29087,#29088),(#29089,#29090,#29091,#29092,#29093,#29094,#29095,#29096,
#29097,#29098,#29099,#29100,#29101,#29102,#29103,#29104,#29105,#29106,#29107,
#29108,#29109,#29110,#29111,#29112,#29113,#29114,#29115,#29116,#29117,#29118,
#29119,#29120,#29121,#29122,#29123,#29124,#29125,#29126,#29127,#29128,#29129,
#29130,#29131,#29132,#29133,#29134,#29135,#29136,#29137,#29138,#29139,#29140,
#29141,#29142,#29143,#29144,#29145,#29146,#29147,#29148,#29149,#29150,#29151,
#29152,#29153,#29154,#29155,#29156,#29157,#29158,#29159,#29160,#29161,#29162,
#29163,#29164,#29165,#29166,#29167,#29168,#29169,#29170,#29171,#29172,#29173,
#29174,#29175,#29176,#29177,#29178,#29179,#29180,#29181,#29182,#29183,#29184,
#29185,#29186,#29187,#29188,#29189,#29190,#29191,#29192,#29193,#29194,#29195,
#29196,#29197,#29198,#29199,#29200,#29201,#29202,#29203,#29204,#29205,#29206,
#29207,#29208,#29209,#29210,#29211,#29212,#29213,#29214,#29215,#29216,#29217,
#29218,#29219,#29220,#29221,#29222,#29223,#29224,#29225,#29226,#29227,#29228,
#29229,#29230,#29231,#29232,#29233,#29234,#29235,#29236,#29237,#29238,#29239,
#29240,#29241,#29242,#29243,#29244,#29245,#29246,#29247,#29248,#29249,#29250,
#29251,#29252,#29253,#29254,#29255,#29256,#29257,#29258,#29259,#29260,#29261,
#29262,#29263,#29264,#29265,#29266,#29267,#29268,#29269,#29270,#29271,#29272,
#29273,#29274,#29275,#29276,#29277,#29278,#29279,#29280,#29281,#29282),
(#29283,#29284,#29285,#29286,#29287,#29288,#29289,#29290,#29291,#29292,
#29293,#29294,#29295,#29296,#29297,#29298,#29299,#29300,#29301,#29302,#29303,
#29304,#29305,#29306,#29307,#29308,#29309,#29310,#29311,#29312,#29313,#29314,
#29315,#29316,#29317,#29318,#29319,#29320,#29321,#29322,#29323,#29324,#29325,
#29326,#29327,#29328,#29329,#29330,#29331,#29332,#29333,#29334,#29335,#29336,
#29337,#29338,#29339,#29340,#29341,#29342,#29343,#29344,#29345,#29346,#29347,
#29348,#29349,#29350,#29351,#29352,#29353,#29354,#29355,#29356,#29357,#29358,
#29359,#29360,#29361,#29362,#29363,#29364,#29365,#29366,#29367,#29368,#29369,
#29370,#29371,#29372,#29373,#29374,#29375,#29376,#29377,#29378,#29379,#29380,
#29381,#29382,#29383,#29384,#29385,#29386,#29387,#29388,#29389,#29390,#29391,
#29392,#29393,#29394,#29395,#29396,#29397,#29398,#29399,#29400,#29401,#29402,
#29403,#29404,#29405,#29406,#29407,#29408,#29409,#29410,#29411,#29412,#29413,
#29414,#29415,#29416,#29417,#29418,#29419,#29420,#29421,#29422,#29423,#29424,
#29425,#29426,#29427,#29428,#29429,#29430,#29431,#29432,#29433,#29434,#29435,
#29436,#29437,#29438,#29439,#29440,#29441,#29442,#29443,#29444,#29445,#29446,
#29447,#29448,#29449,#29450,#29451,#29452,#29453,#29454,#29455,#29456,#29457,
#29458,#29459,#29460,#29461,#29462,#29463,#29464,#29465,#29466,#29467,#29468,
#29469,#29470,#29471,#29472,#29473,#29474,#29475,#29476),(#29477,#29478,
#29479,#29480,#29481,#29482,#29483,#29484,#29485,#29486,#29487,#29488,#29489,
#29490,#29491,#29492,#29493,#29494,#29495,#29496,#29497,#29498,#29499,#29500,
#29501,#29502,#29503,#29504,#29505,#29506,#29507,#29508,#29509,#29510,#29511,
#29512,#29513,#29514,#29515,#29516,#29517,#29518,#29519,#29520,#29521,#29522,
#29523,#29524,#29525,#29526,#29527,#29528,#29529,#29530,#29531,#29532,#29533,
#29534,#29535,#29536,#29537,#29538,#29539,#29540,#29541,#29542,#29543,#29544,
#29545,#29546,#29547,#29548,#29549,#29550,#29551,#29552,#29553,#29554,#29555,
#29556,#29557,#29558,#29559,#29560,#29561,#29562,#29563,#29564,#29565,#29566,
#29567,#29568,#29569,#29570,#29571,#29572,#29573,#29574,#29575,#29576,#29577,
#29578,#29579,#29580,#29581,#29582,#29583,#29584,#29585,#29586,#29587,#29588,
#29589,#29590,#29591,#29592,#29593,#29594,#29595,#29596,#29597,#29598,#29599,
#29600,#29601,#29602,#29603,#29604,#29605,#29606,#29607,#29608,#29609,#29610,
#29611,#29612,#29613,#29614,#29615,#29616,#29617,#29618,#29619,#29620,#29621,
#29622,#29623,#29624,#29625,#29626,#29627,#29628,#29629,#29630,#29631,#29632,
#29633,#29634,#29635,#29636,#29637,#29638,#29639,#29640,#29641,#29642,#29643,
#29644,#29645,#29646,#29647,#29648,#29649,#29650,#29651,#29652,#29653,#29654,
#29655,#29656,#29657,#29658,#29659,#29660,#29661,#29662,#29663,#29664,#29665,
#29666,#29667,#29668,#29669,#29670)),.UNSPECIFIED.,.F.,.F.,.F.,(4,4),(4,
1,1,1,1,1,1,1,1,1,1,1,1,1,1,1,1,1,1,1,1,1,1,1,1,1,1,1,1,1,1,1,1,1,1,1,1,
1,1,1,1,1,1,1,1,1,1,1,1,1,1,1,1,1,1,1,1,1,1,1,1,1,1,1,1,1,1,1,1,1,1,1,1,
1,1,1,1,1,1,1,1,1,1,1,1,1,1,1,1,1,1,1,1,1,1,1,1,1,1,1,1,1,1,1,1,1,1,1,1,
1,1,1,1,1,1,1,1,1,1,1,1,1,1,1,1,1,1,1,1,1,1,1,1,1,1,1,1,1,1,1,1,1,1,1,1,
1,1,1,1,1,1,1,1,1,1,1,1,1,1,1,1,1,1,1,1,1,1,1,1,1,1,1,1,1,1,1,1,1,1,1,1,
1,1,1,1,1,1,1,1,1,1,4),(0.,0.0986691610045069),(8.30989595155334,8.80798080180439,
9.30606565205544,9.80415050230649,10.3022353525575,10.8003202028086,11.2984050530596,
11.7964899033107,12.2945747535617,12.7926596038128,13.2907444540638,13.7888293043149,
14.2869141545659,14.784999004817,15.283083855068,15.7811687053191,16.2792535555701,
16.7773384058212,17.2754232560722,17.7735081063233,18.2715929565743,18.7696778068254,
19.2677626570764,19.7658475073275,20.2639323575785,20.7620172078296,21.2601020580806,
21.7581869083317,22.2562717585827,22.7543566088338,23.2524414590848,23.7505263093359,
24.2486111595869,24.746696009838,25.244780860089,25.7428657103401,26.2409505605911,
26.7390354108422,27.2371202610932,27.7352051113443,28.2332899615953,28.7313748118464,
29.2294596620974,29.7275445123485,30.2256293625995,30.7237142128506,31.2217990631016,
31.7198839133527,32.2179687636037,32.7160536138548,33.2141384641058,33.7122233143569,
34.2103081646079,34.708393014859,35.20647786511,35.7045627153611,36.2026475656121,
36.7007324158632,37.1988172661142,37.6969021163653,38.1949869666163,38.6930718168674,
39.1911566671184,39.6892415173695,40.1873263676205,40.6854112178715,41.1834960681226,
41.6815809183737,42.1796657686247,42.6777506188757,43.1758354691268,43.6739203193778,
44.1720051696289,44.67009001988,45.168174870131,45.666259720382,46.1643445706331,
46.6624294208841,47.1605142711352,47.6585991213862,48.1566839716373,48.6547688218883,
49.1528536721394,49.6509385223904,50.1490233726415,50.6471082228925,51.1451930731436,
51.6432779233946,52.1413627736457,52.6394476238967,53.1375324741478,53.6356173243988,
54.1337021746499,54.6317870249009,55.129871875152,56.1260415756541,57.1222112761562,
58.1183809766583,58.6164658269093,59.1145506771604,59.6126355274114,60.1107203776625,
60.6088052279135,61.1068900781646,61.6049749284156,62.1030597786667,62.6011446289177,
63.0992294791688,63.5973143294198,64.0953991796709,64.5934840299219,65.091568880173,
65.589653730424,66.0877385806751,66.5858234309261,67.0839082811772,67.5819931314282,
68.0800779816793,68.5781628319303,69.0762476821814,69.5743325324324,70.0724173826835,
70.5705022329345,71.0685870831856,71.5666719334366,72.0647567836877,72.5628416339387,
73.0609264841898,73.5590113344408,74.0570961846919,74.5551810349429,75.053265885194,
75.551350735445,76.0494355856961,76.5475204359471,77.0456052861982,77.5436901364492,
78.0417749867003,78.5398598369513,79.0379446872024,79.5360295374534,80.0341143877044,
80.5321992379555,81.0302840882066,81.5283689384576,82.0264537887087,82.5245386389597,
83.0226234892107,83.5207083394618,84.0187931897129,84.5168780399639,85.0149628902149,
85.513047740466,86.011132590717,86.5092174409681,87.0073022912191,87.5053871414702,
88.0034719917212,88.5015568419723,88.9996416922233,89.4977265424744,89.9958113927254,
90.4938962429765,90.9919810932275,91.4900659434786,91.9881507937296,92.4862356439807,
92.9843204942317,93.4824053444828,93.9804901947338,94.4785750449849,94.9766598952359,
95.474744745487,95.972829595738,96.4709144459891,96.9689992962401,97.4670841464912,
97.9651689967422,98.4632538469933,98.9613386972443,99.4594235474954,99.9575083977464,
100.455593247997,100.953678098249,101.4517629485,101.949847798751,102.447932649002,
102.946017499253,103.444102349504,103.942187199755,104.440272050006,104.938356900257),
 .UNSPECIFIED.);
#340=B_SPLINE_SURFACE_WITH_KNOTS('',3,3,((#29850,#29851,#29852,#29853,#29854,
#29855,#29856,#29857,#29858,#29859,#29860,#29861,#29862,#29863,#29864,#29865,
#29866,#29867,#29868,#29869,#29870,#29871,#29872,#29873,#29874,#29875,#29876,
#29877,#29878,#29879,#29880,#29881,#29882,#29883,#29884,#29885,#29886,#29887,
#29888,#29889,#29890,#29891,#29892,#29893,#29894,#29895,#29896,#29897,#29898,
#29899,#29900,#29901,#29902,#29903,#29904,#29905,#29906,#29907,#29908,#29909,
#29910,#29911,#29912,#29913,#29914,#29915,#29916,#29917,#29918,#29919,#29920,
#29921,#29922,#29923,#29924,#29925,#29926,#29927,#29928,#29929,#29930,#29931,
#29932,#29933,#29934,#29935,#29936,#29937,#29938,#29939,#29940,#29941,#29942,
#29943,#29944,#29945,#29946,#29947,#29948,#29949,#29950,#29951,#29952,#29953,
#29954,#29955,#29956,#29957,#29958,#29959,#29960,#29961,#29962,#29963,#29964,
#29965,#29966,#29967,#29968,#29969,#29970,#29971,#29972,#29973,#29974,#29975,
#29976,#29977,#29978,#29979,#29980,#29981,#29982,#29983,#29984,#29985,#29986,
#29987,#29988,#29989,#29990,#29991,#29992,#29993,#29994,#29995,#29996,#29997,
#29998,#29999,#30000,#30001,#30002,#30003,#30004,#30005,#30006,#30007,#30008,
#30009,#30010,#30011,#30012,#30013,#30014,#30015,#30016,#30017,#30018,#30019,
#30020,#30021,#30022,#30023,#30024,#30025,#30026,#30027,#30028,#30029,#30030,
#30031,#30032,#30033,#30034,#30035,#30036,#30037,#30038,#30039,#30040,#30041,
#30042,#30043),(#30044,#30045,#30046,#30047,#30048,#30049,#30050,#30051,
#30052,#30053,#30054,#30055,#30056,#30057,#30058,#30059,#30060,#30061,#30062,
#30063,#30064,#30065,#30066,#30067,#30068,#30069,#30070,#30071,#30072,#30073,
#30074,#30075,#30076,#30077,#30078,#30079,#30080,#30081,#30082,#30083,#30084,
#30085,#30086,#30087,#30088,#30089,#30090,#30091,#30092,#30093,#30094,#30095,
#30096,#30097,#30098,#30099,#30100,#30101,#30102,#30103,#30104,#30105,#30106,
#30107,#30108,#30109,#30110,#30111,#30112,#30113,#30114,#30115,#30116,#30117,
#30118,#30119,#30120,#30121,#30122,#30123,#30124,#30125,#30126,#30127,#30128,
#30129,#30130,#30131,#30132,#30133,#30134,#30135,#30136,#30137,#30138,#30139,
#30140,#30141,#30142,#30143,#30144,#30145,#30146,#30147,#30148,#30149,#30150,
#30151,#30152,#30153,#30154,#30155,#30156,#30157,#30158,#30159,#30160,#30161,
#30162,#30163,#30164,#30165,#30166,#30167,#30168,#30169,#30170,#30171,#30172,
#30173,#30174,#30175,#30176,#30177,#30178,#30179,#30180,#30181,#30182,#30183,
#30184,#30185,#30186,#30187,#30188,#30189,#30190,#30191,#30192,#30193,#30194,
#30195,#30196,#30197,#30198,#30199,#30200,#30201,#30202,#30203,#30204,#30205,
#30206,#30207,#30208,#30209,#30210,#30211,#30212,#30213,#30214,#30215,#30216,
#30217,#30218,#30219,#30220,#30221,#30222,#30223,#30224,#30225,#30226,#30227,
#30228,#30229,#30230,#30231,#30232,#30233,#30234,#30235,#30236,#30237),
(#30238,#30239,#30240,#30241,#30242,#30243,#30244,#30245,#30246,#30247,
#30248,#30249,#30250,#30251,#30252,#30253,#30254,#30255,#30256,#30257,#30258,
#30259,#30260,#30261,#30262,#30263,#30264,#30265,#30266,#30267,#30268,#30269,
#30270,#30271,#30272,#30273,#30274,#30275,#30276,#30277,#30278,#30279,#30280,
#30281,#30282,#30283,#30284,#30285,#30286,#30287,#30288,#30289,#30290,#30291,
#30292,#30293,#30294,#30295,#30296,#30297,#30298,#30299,#30300,#30301,#30302,
#30303,#30304,#30305,#30306,#30307,#30308,#30309,#30310,#30311,#30312,#30313,
#30314,#30315,#30316,#30317,#30318,#30319,#30320,#30321,#30322,#30323,#30324,
#30325,#30326,#30327,#30328,#30329,#30330,#30331,#30332,#30333,#30334,#30335,
#30336,#30337,#30338,#30339,#30340,#30341,#30342,#30343,#30344,#30345,#30346,
#30347,#30348,#30349,#30350,#30351,#30352,#30353,#30354,#30355,#30356,#30357,
#30358,#30359,#30360,#30361,#30362,#30363,#30364,#30365,#30366,#30367,#30368,
#30369,#30370,#30371,#30372,#30373,#30374,#30375,#30376,#30377,#30378,#30379,
#30380,#30381,#30382,#30383,#30384,#30385,#30386,#30387,#30388,#30389,#30390,
#30391,#30392,#30393,#30394,#30395,#30396,#30397,#30398,#30399,#30400,#30401,
#30402,#30403,#30404,#30405,#30406,#30407,#30408,#30409,#30410,#30411,#30412,
#30413,#30414,#30415,#30416,#30417,#30418,#30419,#30420,#30421,#30422,#30423,
#30424,#30425,#30426,#30427,#30428,#30429,#30430,#30431),(#30432,#30433,
#30434,#30435,#30436,#30437,#30438,#30439,#30440,#30441,#30442,#30443,#30444,
#30445,#30446,#30447,#30448,#30449,#30450,#30451,#30452,#30453,#30454,#30455,
#30456,#30457,#30458,#30459,#30460,#30461,#30462,#30463,#30464,#30465,#30466,
#30467,#30468,#30469,#30470,#30471,#30472,#30473,#30474,#30475,#30476,#30477,
#30478,#30479,#30480,#30481,#30482,#30483,#30484,#30485,#30486,#30487,#30488,
#30489,#30490,#30491,#30492,#30493,#30494,#30495,#30496,#30497,#30498,#30499,
#30500,#30501,#30502,#30503,#30504,#30505,#30506,#30507,#30508,#30509,#30510,
#30511,#30512,#30513,#30514,#30515,#30516,#30517,#30518,#30519,#30520,#30521,
#30522,#30523,#30524,#30525,#30526,#30527,#30528,#30529,#30530,#30531,#30532,
#30533,#30534,#30535,#30536,#30537,#30538,#30539,#30540,#30541,#30542,#30543,
#30544,#30545,#30546,#30547,#30548,#30549,#30550,#30551,#30552,#30553,#30554,
#30555,#30556,#30557,#30558,#30559,#30560,#30561,#30562,#30563,#30564,#30565,
#30566,#30567,#30568,#30569,#30570,#30571,#30572,#30573,#30574,#30575,#30576,
#30577,#30578,#30579,#30580,#30581,#30582,#30583,#30584,#30585,#30586,#30587,
#30588,#30589,#30590,#30591,#30592,#30593,#30594,#30595,#30596,#30597,#30598,
#30599,#30600,#30601,#30602,#30603,#30604,#30605,#30606,#30607,#30608,#30609,
#30610,#30611,#30612,#30613,#30614,#30615,#30616,#30617,#30618,#30619,#30620,
#30621,#30622,#30623,#30624,#30625)),.UNSPECIFIED.,.F.,.F.,.F.,(4,4),(4,
1,1,1,1,1,1,1,1,1,1,1,1,1,1,1,1,1,1,1,1,1,1,1,1,1,1,1,1,1,1,1,1,1,1,1,1,
1,1,1,1,1,1,1,1,1,1,1,1,1,1,1,1,1,1,1,1,1,1,1,1,1,1,1,1,1,1,1,1,1,1,1,1,
1,1,1,1,1,1,1,1,1,1,1,1,1,1,1,1,1,1,1,1,1,1,1,1,1,1,1,1,1,1,1,1,1,1,1,1,
1,1,1,1,1,1,1,1,1,1,1,1,1,1,1,1,1,1,1,1,1,1,1,1,1,1,1,1,1,1,1,1,1,1,1,1,
1,1,1,1,1,1,1,1,1,1,1,1,1,1,1,1,1,1,1,1,1,1,1,1,1,1,1,1,1,1,1,1,1,1,1,1,
1,1,1,1,1,1,1,1,1,1,4),(0.,0.0986691610045069),(11.6147305479242,12.1128153981753,
12.6109002484263,13.1089850986774,13.6070699489284,14.1051547991795,14.6032396494305,
15.1013244996816,15.5994093499326,16.0974942001837,16.5955790504347,17.0936639006858,
17.5917487509368,18.0898336011878,18.5879184514389,19.0860033016899,19.584088151941,
20.082173002192,20.5802578524431,21.0783427026941,21.5764275529452,22.0745124031962,
22.5725972534473,23.0706821036983,23.5687669539494,24.0668518042004,24.5649366544515,
25.0630215047025,25.5611063549536,26.0591912052046,26.5572760554557,27.0553609057067,
27.5534457559578,28.0515306062088,28.5496154564599,29.0477003067109,29.545785156962,
30.043870007213,30.5419548574641,31.0400397077151,31.5381245579662,32.0362094082172,
32.5342942584683,33.0323791087193,33.5304639589704,34.0285488092214,34.5266336594725,
35.0247185097235,35.5228033599746,36.0208882102256,36.5189730604767,37.0170579107277,
37.5151427609788,38.0132276112298,38.5113124614809,39.0093973117319,39.507482161983,
40.005567012234,40.5036518624851,41.0017367127361,41.4998215629872,41.9979064132382,
42.4959912634893,42.9940761137403,43.4921609639914,43.9902458142424,44.4883306644935,
44.9864155147445,45.4845003649956,45.9825852152466,46.4806700654977,46.9787549157487,
47.4768397659998,47.9749246162508,48.4730094665019,48.9710943167529,49.469179167004,
49.967264017255,50.4653488675061,50.9634337177571,51.4615185680082,51.9596034182592,
52.4576882685103,52.9557731187613,53.4538579690124,53.9519428192634,54.4500276695145,
54.9481125197655,55.4461973700166,55.9442822202676,56.4423670705187,56.9404519207697,
57.4385367710208,57.9366216212718,58.4347064715229,59.430876172025,60.427045872527,
61.4232155730292,61.9213004232802,62.4193852735312,62.9174701237823,63.4155549740333,
63.9136398242844,64.4117246745354,64.9098095247865,65.4078943750375,65.9059792252886,
66.4040640755397,66.9021489257907,67.4002337760417,67.8983186262928,68.3964034765438,
68.8944883267949,69.3925731770459,69.890658027297,70.388742877548,70.8868277277991,
71.3849125780501,71.8829974283012,72.3810822785522,72.8791671288033,73.3772519790543,
73.8753368293054,74.3734216795564,74.8715065298075,75.3695913800585,75.8676762303096,
76.3657610805606,76.8638459308117,77.3619307810627,77.8600156313138,78.3581004815648,
78.8561853318159,79.3542701820669,79.852355032318,80.350439882569,80.8485247328201,
81.3466095830711,81.8446944333222,82.3427792835732,82.8408641338243,83.3389489840753,
83.8370338343264,84.3351186845774,84.8332035348285,85.3312883850795,85.8293732353306,
86.3274580855816,86.8255429358327,87.3236277860837,87.8217126363348,88.3197974865858,
88.8178823368369,89.3159671870879,89.814052037339,90.31213688759,90.8102217378411,
91.3083065880921,91.8063914383432,92.3044762885942,92.8025611388453,93.3006459890963,
93.7987308393474,94.2968156895984,94.7949005398495,95.2929853901005,95.7910702403516,
96.2891550906026,96.7872399408537,97.2853247911047,97.7834096413558,98.2814944916068,
98.7795793418579,99.2776641921089,99.77574904236,100.273833892611,100.771918742862,
101.270003593113,101.768088443364,102.266173293615,102.764258143866,103.262342994117,
103.760427844368,104.258512694619,104.75659754487,105.254682395122,105.752767245373,
106.250852095624,106.748936945875,107.247021796126,107.745106646377,108.243191496628),
 .UNSPECIFIED.);
#341=B_SPLINE_SURFACE_WITH_KNOTS('',3,3,((#30768,#30769,#30770,#30771,#30772,
#30773,#30774,#30775,#30776,#30777,#30778,#30779,#30780,#30781,#30782,#30783,
#30784,#30785,#30786,#30787,#30788,#30789,#30790,#30791,#30792,#30793,#30794,
#30795,#30796,#30797,#30798,#30799,#30800,#30801,#30802,#30803,#30804,#30805,
#30806,#30807,#30808,#30809,#30810,#30811,#30812,#30813,#30814,#30815,#30816,
#30817,#30818,#30819,#30820,#30821,#30822,#30823,#30824,#30825,#30826,#30827,
#30828,#30829,#30830,#30831,#30832,#30833,#30834,#30835,#30836,#30837,#30838,
#30839,#30840,#30841,#30842,#30843,#30844,#30845,#30846,#30847,#30848,#30849,
#30850,#30851,#30852,#30853,#30854,#30855,#30856,#30857,#30858,#30859,#30860,
#30861,#30862,#30863,#30864,#30865,#30866,#30867,#30868,#30869,#30870,#30871,
#30872,#30873,#30874,#30875,#30876,#30877,#30878,#30879,#30880,#30881,#30882,
#30883,#30884,#30885,#30886,#30887,#30888,#30889,#30890,#30891,#30892,#30893,
#30894,#30895,#30896,#30897,#30898,#30899,#30900,#30901,#30902,#30903,#30904,
#30905,#30906,#30907,#30908,#30909,#30910,#30911,#30912,#30913,#30914,#30915,
#30916,#30917,#30918,#30919,#30920,#30921,#30922,#30923,#30924,#30925,#30926,
#30927,#30928,#30929,#30930,#30931,#30932,#30933,#30934,#30935,#30936,#30937,
#30938,#30939,#30940,#30941,#30942,#30943,#30944,#30945,#30946,#30947,#30948,
#30949,#30950,#30951,#30952,#30953,#30954,#30955,#30956,#30957,#30958,#30959,
#30960,#30961),(#30962,#30963,#30964,#30965,#30966,#30967,#30968,#30969,
#30970,#30971,#30972,#30973,#30974,#30975,#30976,#30977,#30978,#30979,#30980,
#30981,#30982,#30983,#30984,#30985,#30986,#30987,#30988,#30989,#30990,#30991,
#30992,#30993,#30994,#30995,#30996,#30997,#30998,#30999,#31000,#31001,#31002,
#31003,#31004,#31005,#31006,#31007,#31008,#31009,#31010,#31011,#31012,#31013,
#31014,#31015,#31016,#31017,#31018,#31019,#31020,#31021,#31022,#31023,#31024,
#31025,#31026,#31027,#31028,#31029,#31030,#31031,#31032,#31033,#31034,#31035,
#31036,#31037,#31038,#31039,#31040,#31041,#31042,#31043,#31044,#31045,#31046,
#31047,#31048,#31049,#31050,#31051,#31052,#31053,#31054,#31055,#31056,#31057,
#31058,#31059,#31060,#31061,#31062,#31063,#31064,#31065,#31066,#31067,#31068,
#31069,#31070,#31071,#31072,#31073,#31074,#31075,#31076,#31077,#31078,#31079,
#31080,#31081,#31082,#31083,#31084,#31085,#31086,#31087,#31088,#31089,#31090,
#31091,#31092,#31093,#31094,#31095,#31096,#31097,#31098,#31099,#31100,#31101,
#31102,#31103,#31104,#31105,#31106,#31107,#31108,#31109,#31110,#31111,#31112,
#31113,#31114,#31115,#31116,#31117,#31118,#31119,#31120,#31121,#31122,#31123,
#31124,#31125,#31126,#31127,#31128,#31129,#31130,#31131,#31132,#31133,#31134,
#31135,#31136,#31137,#31138,#31139,#31140,#31141,#31142,#31143,#31144,#31145,
#31146,#31147,#31148,#31149,#31150,#31151,#31152,#31153,#31154,#31155),
(#31156,#31157,#31158,#31159,#31160,#31161,#31162,#31163,#31164,#31165,
#31166,#31167,#31168,#31169,#31170,#31171,#31172,#31173,#31174,#31175,#31176,
#31177,#31178,#31179,#31180,#31181,#31182,#31183,#31184,#31185,#31186,#31187,
#31188,#31189,#31190,#31191,#31192,#31193,#31194,#31195,#31196,#31197,#31198,
#31199,#31200,#31201,#31202,#31203,#31204,#31205,#31206,#31207,#31208,#31209,
#31210,#31211,#31212,#31213,#31214,#31215,#31216,#31217,#31218,#31219,#31220,
#31221,#31222,#31223,#31224,#31225,#31226,#31227,#31228,#31229,#31230,#31231,
#31232,#31233,#31234,#31235,#31236,#31237,#31238,#31239,#31240,#31241,#31242,
#31243,#31244,#31245,#31246,#31247,#31248,#31249,#31250,#31251,#31252,#31253,
#31254,#31255,#31256,#31257,#31258,#31259,#31260,#31261,#31262,#31263,#31264,
#31265,#31266,#31267,#31268,#31269,#31270,#31271,#31272,#31273,#31274,#31275,
#31276,#31277,#31278,#31279,#31280,#31281,#31282,#31283,#31284,#31285,#31286,
#31287,#31288,#31289,#31290,#31291,#31292,#31293,#31294,#31295,#31296,#31297,
#31298,#31299,#31300,#31301,#31302,#31303,#31304,#31305,#31306,#31307,#31308,
#31309,#31310,#31311,#31312,#31313,#31314,#31315,#31316,#31317,#31318,#31319,
#31320,#31321,#31322,#31323,#31324,#31325,#31326,#31327,#31328,#31329,#31330,
#31331,#31332,#31333,#31334,#31335,#31336,#31337,#31338,#31339,#31340,#31341,
#31342,#31343,#31344,#31345,#31346,#31347,#31348,#31349),(#31350,#31351,
#31352,#31353,#31354,#31355,#31356,#31357,#31358,#31359,#31360,#31361,#31362,
#31363,#31364,#31365,#31366,#31367,#31368,#31369,#31370,#31371,#31372,#31373,
#31374,#31375,#31376,#31377,#31378,#31379,#31380,#31381,#31382,#31383,#31384,
#31385,#31386,#31387,#31388,#31389,#31390,#31391,#31392,#31393,#31394,#31395,
#31396,#31397,#31398,#31399,#31400,#31401,#31402,#31403,#31404,#31405,#31406,
#31407,#31408,#31409,#31410,#31411,#31412,#31413,#31414,#31415,#31416,#31417,
#31418,#31419,#31420,#31421,#31422,#31423,#31424,#31425,#31426,#31427,#31428,
#31429,#31430,#31431,#31432,#31433,#31434,#31435,#31436,#31437,#31438,#31439,
#31440,#31441,#31442,#31443,#31444,#31445,#31446,#31447,#31448,#31449,#31450,
#31451,#31452,#31453,#31454,#31455,#31456,#31457,#31458,#31459,#31460,#31461,
#31462,#31463,#31464,#31465,#31466,#31467,#31468,#31469,#31470,#31471,#31472,
#31473,#31474,#31475,#31476,#31477,#31478,#31479,#31480,#31481,#31482,#31483,
#31484,#31485,#31486,#31487,#31488,#31489,#31490,#31491,#31492,#31493,#31494,
#31495,#31496,#31497,#31498,#31499,#31500,#31501,#31502,#31503,#31504,#31505,
#31506,#31507,#31508,#31509,#31510,#31511,#31512,#31513,#31514,#31515,#31516,
#31517,#31518,#31519,#31520,#31521,#31522,#31523,#31524,#31525,#31526,#31527,
#31528,#31529,#31530,#31531,#31532,#31533,#31534,#31535,#31536,#31537,#31538,
#31539,#31540,#31541,#31542,#31543)),.UNSPECIFIED.,.F.,.F.,.F.,(4,4),(4,
1,1,1,1,1,1,1,1,1,1,1,1,1,1,1,1,1,1,1,1,1,1,1,1,1,1,1,1,1,1,1,1,1,1,1,1,
1,1,1,1,1,1,1,1,1,1,1,1,1,1,1,1,1,1,1,1,1,1,1,1,1,1,1,1,1,1,1,1,1,1,1,1,
1,1,1,1,1,1,1,1,1,1,1,1,1,1,1,1,1,1,1,1,1,1,1,1,1,1,1,1,1,1,1,1,1,1,1,1,
1,1,1,1,1,1,1,1,1,1,1,1,1,1,1,1,1,1,1,1,1,1,1,1,1,1,1,1,1,1,1,1,1,1,1,1,
1,1,1,1,1,1,1,1,1,1,1,1,1,1,1,1,1,1,1,1,1,1,1,1,1,1,1,1,1,1,1,1,1,1,1,1,
1,1,1,1,1,1,1,1,1,1,4),(0.,0.0986691610045069),(8.30989595155336,8.80798080180441,
9.30606565205546,9.80415050230651,10.3022353525576,10.8003202028086,11.2984050530597,
11.7964899033107,12.2945747535618,12.7926596038128,13.2907444540639,13.7888293043149,
14.286914154566,14.784999004817,15.2830838550681,15.7811687053191,16.2792535555702,
16.7773384058212,17.2754232560723,17.7735081063233,18.2715929565744,18.7696778068254,
19.2677626570764,19.7658475073275,20.2639323575785,20.7620172078296,21.2601020580806,
21.7581869083317,22.2562717585827,22.7543566088338,23.2524414590848,23.7505263093359,
24.2486111595869,24.746696009838,25.244780860089,25.7428657103401,26.2409505605911,
26.7390354108422,27.2371202610932,27.7352051113443,28.2332899615953,28.7313748118464,
29.2294596620974,29.7275445123485,30.2256293625995,30.7237142128506,31.2217990631016,
31.7198839133527,32.2179687636037,32.7160536138548,33.2141384641058,33.7122233143569,
34.2103081646079,34.708393014859,35.20647786511,35.7045627153611,36.2026475656121,
36.7007324158632,37.1988172661142,37.6969021163653,38.1949869666163,38.6930718168674,
39.1911566671184,39.6892415173695,40.1873263676205,40.6854112178716,41.1834960681226,
41.6815809183737,42.1796657686247,42.6777506188758,43.1758354691268,43.6739203193779,
44.1720051696289,44.67009001988,45.168174870131,45.6662597203821,46.1643445706331,
46.6624294208842,47.1605142711352,47.6585991213863,48.1566839716373,48.6547688218884,
49.1528536721394,49.6509385223905,50.1490233726415,50.6471082228926,51.1451930731436,
51.6432779233947,52.1413627736457,52.6394476238968,53.1375324741478,53.6356173243989,
54.1337021746499,54.631787024901,55.129871875152,56.1260415756541,57.1222112761562,
58.1183809766583,58.6164658269093,59.1145506771604,59.6126355274115,60.1107203776625,
60.6088052279135,61.1068900781646,61.6049749284156,62.1030597786667,62.6011446289178,
63.0992294791688,63.5973143294198,64.0953991796709,64.5934840299219,65.091568880173,
65.589653730424,66.0877385806751,66.5858234309261,67.0839082811772,67.5819931314282,
68.0800779816793,68.5781628319303,69.0762476821814,69.5743325324324,70.0724173826835,
70.5705022329345,71.0685870831856,71.5666719334366,72.0647567836877,72.5628416339387,
73.0609264841898,73.5590113344408,74.0570961846919,74.5551810349429,75.053265885194,
75.551350735445,76.0494355856961,76.5475204359471,77.0456052861982,77.5436901364492,
78.0417749867003,78.5398598369513,79.0379446872024,79.5360295374534,80.0341143877045,
80.5321992379555,81.0302840882066,81.5283689384576,82.0264537887087,82.5245386389597,
83.0226234892108,83.5207083394618,84.0187931897129,84.5168780399639,85.014962890215,
85.513047740466,86.0111325907171,86.5092174409681,87.0073022912192,87.5053871414702,
88.0034719917213,88.5015568419723,88.9996416922233,89.4977265424744,89.9958113927255,
90.4938962429765,90.9919810932276,91.4900659434786,91.9881507937297,92.4862356439807,
92.9843204942318,93.4824053444828,93.9804901947338,94.4785750449849,94.976659895236,
95.474744745487,95.972829595738,96.4709144459891,96.9689992962401,97.4670841464912,
97.9651689967422,98.4632538469933,98.9613386972443,99.4594235474954,99.9575083977464,
100.455593247997,100.953678098249,101.4517629485,101.949847798751,102.447932649002,
102.946017499253,103.444102349504,103.942187199755,104.440272050006,104.938356900257),
 .UNSPECIFIED.);
#342=B_SPLINE_SURFACE_WITH_KNOTS('',3,3,((#31946,#31947,#31948,#31949,#31950,
#31951,#31952,#31953,#31954,#31955,#31956,#31957,#31958,#31959,#31960,#31961,
#31962,#31963,#31964,#31965,#31966,#31967,#31968,#31969,#31970,#31971,#31972,
#31973,#31974,#31975,#31976,#31977,#31978,#31979,#31980,#31981,#31982,#31983,
#31984,#31985,#31986,#31987,#31988,#31989,#31990,#31991,#31992,#31993,#31994,
#31995,#31996,#31997,#31998,#31999,#32000,#32001,#32002,#32003,#32004,#32005,
#32006,#32007,#32008,#32009,#32010,#32011,#32012,#32013,#32014,#32015,#32016,
#32017,#32018,#32019,#32020,#32021,#32022,#32023,#32024,#32025,#32026,#32027,
#32028,#32029,#32030,#32031,#32032,#32033,#32034,#32035,#32036,#32037,#32038,
#32039,#32040,#32041,#32042,#32043,#32044,#32045,#32046,#32047,#32048,#32049,
#32050,#32051,#32052,#32053,#32054,#32055,#32056,#32057,#32058,#32059,#32060,
#32061,#32062,#32063,#32064,#32065,#32066,#32067,#32068,#32069,#32070,#32071,
#32072,#32073,#32074,#32075,#32076,#32077,#32078,#32079,#32080,#32081,#32082,
#32083,#32084,#32085,#32086,#32087,#32088,#32089,#32090,#32091,#32092,#32093,
#32094,#32095,#32096,#32097,#32098,#32099,#32100,#32101,#32102,#32103,#32104,
#32105,#32106,#32107,#32108,#32109,#32110,#32111,#32112,#32113,#32114,#32115,
#32116,#32117,#32118,#32119,#32120,#32121,#32122,#32123,#32124,#32125,#32126,
#32127,#32128,#32129,#32130,#32131,#32132,#32133,#32134,#32135,#32136,#32137,
#32138,#32139),(#32140,#32141,#32142,#32143,#32144,#32145,#32146,#32147,
#32148,#32149,#32150,#32151,#32152,#32153,#32154,#32155,#32156,#32157,#32158,
#32159,#32160,#32161,#32162,#32163,#32164,#32165,#32166,#32167,#32168,#32169,
#32170,#32171,#32172,#32173,#32174,#32175,#32176,#32177,#32178,#32179,#32180,
#32181,#32182,#32183,#32184,#32185,#32186,#32187,#32188,#32189,#32190,#32191,
#32192,#32193,#32194,#32195,#32196,#32197,#32198,#32199,#32200,#32201,#32202,
#32203,#32204,#32205,#32206,#32207,#32208,#32209,#32210,#32211,#32212,#32213,
#32214,#32215,#32216,#32217,#32218,#32219,#32220,#32221,#32222,#32223,#32224,
#32225,#32226,#32227,#32228,#32229,#32230,#32231,#32232,#32233,#32234,#32235,
#32236,#32237,#32238,#32239,#32240,#32241,#32242,#32243,#32244,#32245,#32246,
#32247,#32248,#32249,#32250,#32251,#32252,#32253,#32254,#32255,#32256,#32257,
#32258,#32259,#32260,#32261,#32262,#32263,#32264,#32265,#32266,#32267,#32268,
#32269,#32270,#32271,#32272,#32273,#32274,#32275,#32276,#32277,#32278,#32279,
#32280,#32281,#32282,#32283,#32284,#32285,#32286,#32287,#32288,#32289,#32290,
#32291,#32292,#32293,#32294,#32295,#32296,#32297,#32298,#32299,#32300,#32301,
#32302,#32303,#32304,#32305,#32306,#32307,#32308,#32309,#32310,#32311,#32312,
#32313,#32314,#32315,#32316,#32317,#32318,#32319,#32320,#32321,#32322,#32323,
#32324,#32325,#32326,#32327,#32328,#32329,#32330,#32331,#32332,#32333),
(#32334,#32335,#32336,#32337,#32338,#32339,#32340,#32341,#32342,#32343,
#32344,#32345,#32346,#32347,#32348,#32349,#32350,#32351,#32352,#32353,#32354,
#32355,#32356,#32357,#32358,#32359,#32360,#32361,#32362,#32363,#32364,#32365,
#32366,#32367,#32368,#32369,#32370,#32371,#32372,#32373,#32374,#32375,#32376,
#32377,#32378,#32379,#32380,#32381,#32382,#32383,#32384,#32385,#32386,#32387,
#32388,#32389,#32390,#32391,#32392,#32393,#32394,#32395,#32396,#32397,#32398,
#32399,#32400,#32401,#32402,#32403,#32404,#32405,#32406,#32407,#32408,#32409,
#32410,#32411,#32412,#32413,#32414,#32415,#32416,#32417,#32418,#32419,#32420,
#32421,#32422,#32423,#32424,#32425,#32426,#32427,#32428,#32429,#32430,#32431,
#32432,#32433,#32434,#32435,#32436,#32437,#32438,#32439,#32440,#32441,#32442,
#32443,#32444,#32445,#32446,#32447,#32448,#32449,#32450,#32451,#32452,#32453,
#32454,#32455,#32456,#32457,#32458,#32459,#32460,#32461,#32462,#32463,#32464,
#32465,#32466,#32467,#32468,#32469,#32470,#32471,#32472,#32473,#32474,#32475,
#32476,#32477,#32478,#32479,#32480,#32481,#32482,#32483,#32484,#32485,#32486,
#32487,#32488,#32489,#32490,#32491,#32492,#32493,#32494,#32495,#32496,#32497,
#32498,#32499,#32500,#32501,#32502,#32503,#32504,#32505,#32506,#32507,#32508,
#32509,#32510,#32511,#32512,#32513,#32514,#32515,#32516,#32517,#32518,#32519,
#32520,#32521,#32522,#32523,#32524,#32525,#32526,#32527),(#32528,#32529,
#32530,#32531,#32532,#32533,#32534,#32535,#32536,#32537,#32538,#32539,#32540,
#32541,#32542,#32543,#32544,#32545,#32546,#32547,#32548,#32549,#32550,#32551,
#32552,#32553,#32554,#32555,#32556,#32557,#32558,#32559,#32560,#32561,#32562,
#32563,#32564,#32565,#32566,#32567,#32568,#32569,#32570,#32571,#32572,#32573,
#32574,#32575,#32576,#32577,#32578,#32579,#32580,#32581,#32582,#32583,#32584,
#32585,#32586,#32587,#32588,#32589,#32590,#32591,#32592,#32593,#32594,#32595,
#32596,#32597,#32598,#32599,#32600,#32601,#32602,#32603,#32604,#32605,#32606,
#32607,#32608,#32609,#32610,#32611,#32612,#32613,#32614,#32615,#32616,#32617,
#32618,#32619,#32620,#32621,#32622,#32623,#32624,#32625,#32626,#32627,#32628,
#32629,#32630,#32631,#32632,#32633,#32634,#32635,#32636,#32637,#32638,#32639,
#32640,#32641,#32642,#32643,#32644,#32645,#32646,#32647,#32648,#32649,#32650,
#32651,#32652,#32653,#32654,#32655,#32656,#32657,#32658,#32659,#32660,#32661,
#32662,#32663,#32664,#32665,#32666,#32667,#32668,#32669,#32670,#32671,#32672,
#32673,#32674,#32675,#32676,#32677,#32678,#32679,#32680,#32681,#32682,#32683,
#32684,#32685,#32686,#32687,#32688,#32689,#32690,#32691,#32692,#32693,#32694,
#32695,#32696,#32697,#32698,#32699,#32700,#32701,#32702,#32703,#32704,#32705,
#32706,#32707,#32708,#32709,#32710,#32711,#32712,#32713,#32714,#32715,#32716,
#32717,#32718,#32719,#32720,#32721)),.UNSPECIFIED.,.F.,.F.,.F.,(4,4),(4,
1,1,1,1,1,1,1,1,1,1,1,1,1,1,1,1,1,1,1,1,1,1,1,1,1,1,1,1,1,1,1,1,1,1,1,1,
1,1,1,1,1,1,1,1,1,1,1,1,1,1,1,1,1,1,1,1,1,1,1,1,1,1,1,1,1,1,1,1,1,1,1,1,
1,1,1,1,1,1,1,1,1,1,1,1,1,1,1,1,1,1,1,1,1,1,1,1,1,1,1,1,1,1,1,1,1,1,1,1,
1,1,1,1,1,1,1,1,1,1,1,1,1,1,1,1,1,1,1,1,1,1,1,1,1,1,1,1,1,1,1,1,1,1,1,1,
1,1,1,1,1,1,1,1,1,1,1,1,1,1,1,1,1,1,1,1,1,1,1,1,1,1,1,1,1,1,1,1,1,1,1,1,
1,1,1,1,1,1,1,1,1,1,4),(0.,0.0986691610045069),(11.6147305479242,12.1128153981753,
12.6109002484263,13.1089850986774,13.6070699489284,14.1051547991795,14.6032396494305,
15.1013244996816,15.5994093499326,16.0974942001837,16.5955790504347,17.0936639006858,
17.5917487509368,18.0898336011879,18.5879184514389,19.08600330169,19.584088151941,
20.0821730021921,20.5802578524431,21.0783427026942,21.5764275529452,22.0745124031963,
22.5725972534473,23.0706821036984,23.5687669539494,24.0668518042005,24.5649366544515,
25.0630215047026,25.5611063549536,26.0591912052047,26.5572760554557,27.0553609057068,
27.5534457559578,28.0515306062089,28.5496154564599,29.047700306711,29.545785156962,
30.0438700072131,30.5419548574641,31.0400397077152,31.5381245579662,32.0362094082173,
32.5342942584683,33.0323791087194,33.5304639589704,34.0285488092214,34.5266336594725,
35.0247185097235,35.5228033599746,36.0208882102256,36.5189730604767,37.0170579107277,
37.5151427609788,38.0132276112299,38.5113124614809,39.0093973117319,39.507482161983,
40.005567012234,40.5036518624851,41.0017367127361,41.4998215629872,41.9979064132382,
42.4959912634893,42.9940761137403,43.4921609639914,43.9902458142424,44.4883306644935,
44.9864155147445,45.4845003649956,45.9825852152466,46.4806700654977,46.9787549157487,
47.4768397659998,47.9749246162508,48.4730094665019,48.9710943167529,49.469179167004,
49.967264017255,50.4653488675061,50.9634337177571,51.4615185680082,51.9596034182592,
52.4576882685103,52.9557731187613,53.4538579690124,53.9519428192634,54.4500276695145,
54.9481125197655,55.4461973700166,55.9442822202676,56.4423670705187,56.9404519207697,
57.4385367710208,57.9366216212718,58.4347064715229,59.430876172025,60.4270458725271,
61.4232155730292,61.9213004232802,62.4193852735313,62.9174701237823,63.4155549740334,
63.9136398242844,64.4117246745355,64.9098095247865,65.4078943750376,65.9059792252886,
66.4040640755397,66.9021489257907,67.4002337760418,67.8983186262928,68.3964034765439,
68.8944883267949,69.392573177046,69.890658027297,70.3887428775481,70.8868277277991,
71.3849125780502,71.8829974283012,72.3810822785523,72.8791671288033,73.3772519790544,
73.8753368293054,74.3734216795565,74.8715065298075,75.3695913800586,75.8676762303096,
76.3657610805606,76.8638459308117,77.3619307810628,77.8600156313138,78.3581004815648,
78.8561853318159,79.3542701820669,79.852355032318,80.350439882569,80.8485247328201,
81.3466095830711,81.8446944333222,82.3427792835733,82.8408641338243,83.3389489840753,
83.8370338343264,84.3351186845774,84.8332035348285,85.3312883850795,85.8293732353306,
86.3274580855816,86.8255429358327,87.3236277860837,87.8217126363348,88.3197974865858,
88.8178823368369,89.3159671870879,89.814052037339,90.31213688759,90.8102217378411,
91.3083065880921,91.8063914383432,92.3044762885942,92.8025611388453,93.3006459890963,
93.7987308393474,94.2968156895984,94.7949005398495,95.2929853901005,95.7910702403516,
96.2891550906026,96.7872399408537,97.2853247911047,97.7834096413558,98.2814944916068,
98.7795793418579,99.2776641921089,99.77574904236,100.273833892611,100.771918742862,
101.270003593113,101.768088443364,102.266173293615,102.764258143866,103.262342994117,
103.760427844368,104.258512694619,104.75659754487,105.254682395122,105.752767245373,
106.250852095624,106.748936945875,107.247021796126,107.745106646377,108.243191496628),
 .UNSPECIFIED.);
#343=B_SPLINE_SURFACE_WITH_KNOTS('',3,3,((#33100,#33101,#33102,#33103,#33104),
(#33105,#33106,#33107,#33108,#33109),(#33110,#33111,#33112,#33113,#33114),
(#33115,#33116,#33117,#33118,#33119)),.UNSPECIFIED.,.F.,.F.,.F.,(4,4),(4,
1,4),(0.,1.),(0.173603820977428,0.583467062619184,1.12995138480819),
 .UNSPECIFIED.);
#344=B_SPLINE_SURFACE_WITH_KNOTS('',3,3,((#33149,#33150,#33151,#33152,#33153),
(#33154,#33155,#33156,#33157,#33158),(#33159,#33160,#33161,#33162,#33163),
(#33164,#33165,#33166,#33167,#33168)),.UNSPECIFIED.,.F.,.F.,.F.,(4,4),(4,
1,4),(0.,1.),(0.173603820977427,0.720088143166436,1.12995138480819),
 .UNSPECIFIED.);
#345=B_SPLINE_SURFACE_WITH_KNOTS('',3,3,((#33238,#33239,#33240,#33241,#33242),
(#33243,#33244,#33245,#33246,#33247),(#33248,#33249,#33250,#33251,#33252),
(#33253,#33254,#33255,#33256,#33257)),.UNSPECIFIED.,.F.,.F.,.F.,(4,4),(4,
1,4),(0.,1.),(0.173603820977428,0.583467062619184,1.12995138480819),
 .UNSPECIFIED.);
#346=B_SPLINE_SURFACE_WITH_KNOTS('',3,3,((#33334,#33335,#33336,#33337,#33338),
(#33339,#33340,#33341,#33342,#33343),(#33344,#33345,#33346,#33347,#33348),
(#33349,#33350,#33351,#33352,#33353)),.UNSPECIFIED.,.F.,.F.,.F.,(4,4),(4,
1,4),(0.,1.),(0.173603820977427,0.720088143166436,1.12995138480819),
 .UNSPECIFIED.);
#347=B_SPLINE_SURFACE_WITH_KNOTS('',3,3,((#33367,#33368,#33369,#33370,#33371),
(#33372,#33373,#33374,#33375,#33376),(#33377,#33378,#33379,#33380,#33381),
(#33382,#33383,#33384,#33385,#33386)),.UNSPECIFIED.,.F.,.F.,.F.,(4,4),(4,
1,4),(0.,1.),(0.173603820977428,0.583467062619184,1.12995138480819),
 .UNSPECIFIED.);
#348=B_SPLINE_SURFACE_WITH_KNOTS('',3,3,((#33408,#33409,#33410,#33411,#33412),
(#33413,#33414,#33415,#33416,#33417),(#33418,#33419,#33420,#33421,#33422),
(#33423,#33424,#33425,#33426,#33427)),.UNSPECIFIED.,.F.,.F.,.F.,(4,4),(4,
1,4),(0.,1.),(0.173603820977428,0.583467062619184,1.12995138480819),
 .UNSPECIFIED.);
#349=B_SPLINE_SURFACE_WITH_KNOTS('',3,3,((#33830,#33831,#33832,#33833,#33834,
#33835,#33836,#33837,#33838,#33839),(#33840,#33841,#33842,#33843,#33844,
#33845,#33846,#33847,#33848,#33849),(#33850,#33851,#33852,#33853,#33854,
#33855,#33856,#33857,#33858,#33859),(#33860,#33861,#33862,#33863,#33864,
#33865,#33866,#33867,#33868,#33869),(#33870,#33871,#33872,#33873,#33874,
#33875,#33876,#33877,#33878,#33879)),.UNSPECIFIED.,.F.,.F.,.F.,(4,1,4),
(4,1,1,1,1,1,1,4),(0.,0.571428571428571,1.),(-1.5707963267949,-1.12199737628207,
-0.673198425769241,-0.224399475256414,0.224399475256414,0.673198425769241,
1.12199737628207,1.5707963267949),.UNSPECIFIED.);
#350=B_SPLINE_SURFACE_WITH_KNOTS('',3,3,((#33883,#33884,#33885,#33886,#33887,
#33888,#33889,#33890,#33891,#33892),(#33893,#33894,#33895,#33896,#33897,
#33898,#33899,#33900,#33901,#33902),(#33903,#33904,#33905,#33906,#33907,
#33908,#33909,#33910,#33911,#33912),(#33913,#33914,#33915,#33916,#33917,
#33918,#33919,#33920,#33921,#33922),(#33923,#33924,#33925,#33926,#33927,
#33928,#33929,#33930,#33931,#33932)),.UNSPECIFIED.,.F.,.F.,.F.,(4,1,4),
(4,1,1,1,1,1,1,4),(0.,0.571428571428571,1.),(-1.5707963267949,-1.12199737628207,
-0.673198425769241,-0.224399475256414,0.224399475256414,0.673198425769241,
1.12199737628207,1.5707963267949),.UNSPECIFIED.);
#351=B_SPLINE_SURFACE_WITH_KNOTS('',3,3,((#33934,#33935,#33936,#33937,#33938,
#33939,#33940,#33941,#33942,#33943),(#33944,#33945,#33946,#33947,#33948,
#33949,#33950,#33951,#33952,#33953),(#33954,#33955,#33956,#33957,#33958,
#33959,#33960,#33961,#33962,#33963),(#33964,#33965,#33966,#33967,#33968,
#33969,#33970,#33971,#33972,#33973),(#33974,#33975,#33976,#33977,#33978,
#33979,#33980,#33981,#33982,#33983)),.UNSPECIFIED.,.F.,.F.,.F.,(4,1,4),
(4,1,1,1,1,1,1,4),(0.,0.571428571428571,1.),(-1.5707963267949,-1.12199737628207,
-0.673198425769241,-0.224399475256414,0.224399475256414,0.673198425769241,
1.12199737628207,1.5707963267949),.UNSPECIFIED.);
#352=B_SPLINE_SURFACE_WITH_KNOTS('',3,3,((#33987,#33988,#33989,#33990,#33991,
#33992,#33993,#33994,#33995,#33996),(#33997,#33998,#33999,#34000,#34001,
#34002,#34003,#34004,#34005,#34006),(#34007,#34008,#34009,#34010,#34011,
#34012,#34013,#34014,#34015,#34016),(#34017,#34018,#34019,#34020,#34021,
#34022,#34023,#34024,#34025,#34026),(#34027,#34028,#34029,#34030,#34031,
#34032,#34033,#34034,#34035,#34036)),.UNSPECIFIED.,.F.,.F.,.F.,(4,1,4),
(4,1,1,1,1,1,1,4),(0.,0.571428571428571,1.),(-1.5707963267949,-1.12199737628207,
-0.673198425769241,-0.224399475256414,0.224399475256414,0.673198425769241,
1.12199737628207,1.5707963267949),.UNSPECIFIED.);
#353=B_SPLINE_SURFACE_WITH_KNOTS('',3,3,((#35356,#35357,#35358,#35359,#35360,
#35361,#35362,#35363,#35364,#35365,#35366,#35367,#35368,#35369,#35370,#35371,
#35372,#35373,#35374,#35375,#35376,#35377,#35378,#35379,#35380,#35381,#35382,
#35383,#35384,#35385,#35386,#35387,#35388,#35389,#35390,#35391,#35392,#35393,
#35394,#35395,#35396,#35397,#35398,#35399,#35400,#35401,#35402,#35403,#35404,
#35405,#35406,#35407,#35408,#35409,#35410,#35411,#35412,#35413,#35414,#35415,
#35416,#35417,#35418,#35419,#35420,#35421,#35422,#35423,#35424,#35425,#35426,
#35427,#35428,#35429,#35430,#35431,#35432,#35433,#35434),(#35435,#35436,
#35437,#35438,#35439,#35440,#35441,#35442,#35443,#35444,#35445,#35446,#35447,
#35448,#35449,#35450,#35451,#35452,#35453,#35454,#35455,#35456,#35457,#35458,
#35459,#35460,#35461,#35462,#35463,#35464,#35465,#35466,#35467,#35468,#35469,
#35470,#35471,#35472,#35473,#35474,#35475,#35476,#35477,#35478,#35479,#35480,
#35481,#35482,#35483,#35484,#35485,#35486,#35487,#35488,#35489,#35490,#35491,
#35492,#35493,#35494,#35495,#35496,#35497,#35498,#35499,#35500,#35501,#35502,
#35503,#35504,#35505,#35506,#35507,#35508,#35509,#35510,#35511,#35512,#35513),
(#35514,#35515,#35516,#35517,#35518,#35519,#35520,#35521,#35522,#35523,
#35524,#35525,#35526,#35527,#35528,#35529,#35530,#35531,#35532,#35533,#35534,
#35535,#35536,#35537,#35538,#35539,#35540,#35541,#35542,#35543,#35544,#35545,
#35546,#35547,#35548,#35549,#35550,#35551,#35552,#35553,#35554,#35555,#35556,
#35557,#35558,#35559,#35560,#35561,#35562,#35563,#35564,#35565,#35566,#35567,
#35568,#35569,#35570,#35571,#35572,#35573,#35574,#35575,#35576,#35577,#35578,
#35579,#35580,#35581,#35582,#35583,#35584,#35585,#35586,#35587,#35588,#35589,
#35590,#35591,#35592),(#35593,#35594,#35595,#35596,#35597,#35598,#35599,
#35600,#35601,#35602,#35603,#35604,#35605,#35606,#35607,#35608,#35609,#35610,
#35611,#35612,#35613,#35614,#35615,#35616,#35617,#35618,#35619,#35620,#35621,
#35622,#35623,#35624,#35625,#35626,#35627,#35628,#35629,#35630,#35631,#35632,
#35633,#35634,#35635,#35636,#35637,#35638,#35639,#35640,#35641,#35642,#35643,
#35644,#35645,#35646,#35647,#35648,#35649,#35650,#35651,#35652,#35653,#35654,
#35655,#35656,#35657,#35658,#35659,#35660,#35661,#35662,#35663,#35664,#35665,
#35666,#35667,#35668,#35669,#35670,#35671)),.UNSPECIFIED.,.F.,.F.,.F.,(4,
4),(4,1,1,1,1,1,1,1,1,1,1,1,1,1,1,1,1,1,1,1,1,1,1,1,1,1,1,1,1,1,1,1,1,1,
1,1,1,1,1,1,1,1,1,1,1,1,1,1,1,1,1,1,1,1,1,1,1,1,1,1,1,1,1,1,1,1,1,1,1,1,
1,1,1,1,1,1,4),(0.,0.0991945497494695),(8.29865039549532,8.79860305073002,
9.29855570596471,9.79850836119941,10.2984610164341,10.7984136716688,11.2983663269035,
11.7983189821382,12.2982716373729,12.7982242926076,13.2981769478423,13.798129603077,
14.2980822583117,14.7980349135464,15.2979875687811,15.7979402240158,16.2978928792505,
16.7978455344852,17.2977981897199,17.7977508449546,18.2977035001893,18.797656155424,
19.2976088106587,19.7975614658934,20.2975141211281,20.7974667763628,21.2974194315975,
21.7973720868322,22.2973247420669,22.7972773973016,23.2972300525363,23.797182707771,
24.2971353630057,24.7970880182404,25.2970406734751,25.7969933287098,26.2969459839445,
26.7968986391792,27.2968512944139,27.7968039496486,28.2967566048833,28.796709260118,
29.2966619153527,29.7966145705874,30.2965672258221,30.7965198810568,31.2964725362915,
31.7964251915262,32.2963778467609,32.7963305019956,33.2962831572303,33.796235812465,
34.2961884676997,34.7961411229344,35.2960937781691,35.7960464334038,36.2959990886385,
36.7959517438732,37.2959043991079,37.7958570543426,38.2958097095773,38.795762364812,
39.2957150200467,39.7956676752814,40.2956203305161,40.7955729857508,41.2955256409855,
41.7954782962202,42.2954309514549,42.7953836066896,43.2953362619243,43.795288917159,
44.2952415723937,44.7951942276284,45.2951468828631,45.7950995380978,46.2950521933325),
 .UNSPECIFIED.);
#354=B_SPLINE_SURFACE_WITH_KNOTS('',3,3,((#35721,#35722,#35723,#35724,#35725,
#35726,#35727,#35728,#35729,#35730,#35731,#35732,#35733,#35734,#35735,#35736,
#35737,#35738,#35739,#35740,#35741,#35742,#35743,#35744,#35745,#35746,#35747,
#35748,#35749,#35750,#35751,#35752,#35753,#35754,#35755,#35756,#35757,#35758,
#35759,#35760,#35761,#35762,#35763,#35764,#35765,#35766,#35767,#35768,#35769,
#35770,#35771,#35772,#35773,#35774,#35775,#35776,#35777,#35778,#35779,#35780,
#35781,#35782,#35783,#35784,#35785,#35786,#35787,#35788,#35789,#35790,#35791,
#35792,#35793,#35794,#35795,#35796,#35797,#35798,#35799),(#35800,#35801,
#35802,#35803,#35804,#35805,#35806,#35807,#35808,#35809,#35810,#35811,#35812,
#35813,#35814,#35815,#35816,#35817,#35818,#35819,#35820,#35821,#35822,#35823,
#35824,#35825,#35826,#35827,#35828,#35829,#35830,#35831,#35832,#35833,#35834,
#35835,#35836,#35837,#35838,#35839,#35840,#35841,#35842,#35843,#35844,#35845,
#35846,#35847,#35848,#35849,#35850,#35851,#35852,#35853,#35854,#35855,#35856,
#35857,#35858,#35859,#35860,#35861,#35862,#35863,#35864,#35865,#35866,#35867,
#35868,#35869,#35870,#35871,#35872,#35873,#35874,#35875,#35876,#35877,#35878),
(#35879,#35880,#35881,#35882,#35883,#35884,#35885,#35886,#35887,#35888,
#35889,#35890,#35891,#35892,#35893,#35894,#35895,#35896,#35897,#35898,#35899,
#35900,#35901,#35902,#35903,#35904,#35905,#35906,#35907,#35908,#35909,#35910,
#35911,#35912,#35913,#35914,#35915,#35916,#35917,#35918,#35919,#35920,#35921,
#35922,#35923,#35924,#35925,#35926,#35927,#35928,#35929,#35930,#35931,#35932,
#35933,#35934,#35935,#35936,#35937,#35938,#35939,#35940,#35941,#35942,#35943,
#35944,#35945,#35946,#35947,#35948,#35949,#35950,#35951,#35952,#35953,#35954,
#35955,#35956,#35957),(#35958,#35959,#35960,#35961,#35962,#35963,#35964,
#35965,#35966,#35967,#35968,#35969,#35970,#35971,#35972,#35973,#35974,#35975,
#35976,#35977,#35978,#35979,#35980,#35981,#35982,#35983,#35984,#35985,#35986,
#35987,#35988,#35989,#35990,#35991,#35992,#35993,#35994,#35995,#35996,#35997,
#35998,#35999,#36000,#36001,#36002,#36003,#36004,#36005,#36006,#36007,#36008,
#36009,#36010,#36011,#36012,#36013,#36014,#36015,#36016,#36017,#36018,#36019,
#36020,#36021,#36022,#36023,#36024,#36025,#36026,#36027,#36028,#36029,#36030,
#36031,#36032,#36033,#36034,#36035,#36036)),.UNSPECIFIED.,.F.,.F.,.F.,(4,
4),(4,1,1,1,1,1,1,1,1,1,1,1,1,1,1,1,1,1,1,1,1,1,1,1,1,1,1,1,1,1,1,1,1,1,
1,1,1,1,1,1,1,1,1,1,1,1,1,1,1,1,1,1,1,1,1,1,1,1,1,1,1,1,1,1,1,1,1,1,1,1,
1,1,1,1,1,1,4),(0.,0.0991945497494695),(11.6149723878396,12.1149250430743,
12.614877698309,13.1148303535437,13.6147830087784,14.1147356640131,14.6146883192478,
15.1146409744825,15.6145936297172,16.1145462849519,16.6144989401866,17.1144515954213,
17.614404250656,18.1143569058907,18.6143095611254,19.1142622163601,19.6142148715948,
20.1141675268295,20.6141201820642,21.1140728372989,21.6140254925336,22.1139781477683,
22.613930803003,23.1138834582377,23.6138361134724,24.1137887687071,24.6137414239418,
25.1136940791765,25.6136467344112,26.1135993896459,26.6135520448806,27.1135047001153,
27.61345735535,28.1134100105847,28.6133626658194,29.1133153210541,29.6132679762888,
30.1132206315235,30.6131732867582,31.1131259419929,31.6130785972276,32.1130312524623,
32.612983907697,33.1129365629317,33.6128892181664,34.1128418734011,34.6127945286358,
35.1127471838705,35.6126998391052,36.1126524943399,36.6126051495746,37.1125578048093,
37.612510460044,38.1124631152787,38.6124157705134,39.1123684257481,39.6123210809828,
40.1122737362175,40.6122263914522,41.1121790466869,41.6121317019216,42.1120843571563,
42.612037012391,43.1119896676257,43.6119423228604,44.1118949780951,44.6118476333298,
45.1118002885645,45.6117529437992,46.1117055990339,46.6116582542686,47.1116109095033,
47.611563564738,48.1115162199727,48.6114688752074,49.1114215304421,49.6113741856768),
 .UNSPECIFIED.);
#355=B_SPLINE_SURFACE_WITH_KNOTS('',3,3,((#37649,#37650,#37651,#37652,#37653,
#37654,#37655,#37656,#37657,#37658,#37659,#37660,#37661,#37662,#37663,#37664,
#37665,#37666,#37667,#37668,#37669,#37670,#37671,#37672,#37673,#37674,#37675,
#37676,#37677,#37678,#37679,#37680,#37681,#37682,#37683,#37684,#37685,#37686,
#37687,#37688,#37689,#37690,#37691,#37692,#37693,#37694,#37695,#37696,#37697,
#37698,#37699,#37700,#37701,#37702,#37703,#37704,#37705,#37706,#37707,#37708,
#37709,#37710,#37711,#37712),(#37713,#37714,#37715,#37716,#37717,#37718,
#37719,#37720,#37721,#37722,#37723,#37724,#37725,#37726,#37727,#37728,#37729,
#37730,#37731,#37732,#37733,#37734,#37735,#37736,#37737,#37738,#37739,#37740,
#37741,#37742,#37743,#37744,#37745,#37746,#37747,#37748,#37749,#37750,#37751,
#37752,#37753,#37754,#37755,#37756,#37757,#37758,#37759,#37760,#37761,#37762,
#37763,#37764,#37765,#37766,#37767,#37768,#37769,#37770,#37771,#37772,#37773,
#37774,#37775,#37776),(#37777,#37778,#37779,#37780,#37781,#37782,#37783,
#37784,#37785,#37786,#37787,#37788,#37789,#37790,#37791,#37792,#37793,#37794,
#37795,#37796,#37797,#37798,#37799,#37800,#37801,#37802,#37803,#37804,#37805,
#37806,#37807,#37808,#37809,#37810,#37811,#37812,#37813,#37814,#37815,#37816,
#37817,#37818,#37819,#37820,#37821,#37822,#37823,#37824,#37825,#37826,#37827,
#37828,#37829,#37830,#37831,#37832,#37833,#37834,#37835,#37836,#37837,#37838,
#37839,#37840),(#37841,#37842,#37843,#37844,#37845,#37846,#37847,#37848,
#37849,#37850,#37851,#37852,#37853,#37854,#37855,#37856,#37857,#37858,#37859,
#37860,#37861,#37862,#37863,#37864,#37865,#37866,#37867,#37868,#37869,#37870,
#37871,#37872,#37873,#37874,#37875,#37876,#37877,#37878,#37879,#37880,#37881,
#37882,#37883,#37884,#37885,#37886,#37887,#37888,#37889,#37890,#37891,#37892,
#37893,#37894,#37895,#37896,#37897,#37898,#37899,#37900,#37901,#37902,#37903,
#37904)),.UNSPECIFIED.,.F.,.F.,.F.,(4,4),(4,1,1,1,1,1,1,1,1,1,1,1,1,1,1,
1,1,1,1,1,1,1,1,1,1,1,1,1,1,1,1,1,1,1,1,1,1,1,1,1,1,1,1,1,1,1,1,1,1,1,1,
1,1,1,1,1,1,1,1,1,1,4),(0.,0.0820126057383863),(8.31473274985799,9.30167185077656,
10.2886109516951,11.2755500526137,12.2624891535323,13.2494282544508,14.2363673553694,
15.223306456288,16.2102455572066,17.1971846581251,18.1841237590437,19.1710628599623,
20.1580019608808,21.1449410617994,22.131880162718,23.1188192636365,24.1057583645551,
25.0926974654737,26.0796365663922,27.0665756673108,28.0535147682294,29.040453869148,
30.0273929700665,31.0143320709851,32.0012711719037,32.9882102728222,33.9751493737408,
34.9620884746594,35.9490275755779,36.9359666764965,37.9229057774151,38.9098448783337,
39.8967839792522,40.8837230801708,41.8706621810894,42.8576012820079,43.8445403829265,
44.8314794838451,45.8184185847636,46.8053576856822,47.7922967866008,48.7792358875193,
49.7661749884379,50.7531140893565,51.7400531902751,52.7269922911936,53.7139313921122,
54.7008704930308,55.6878095939493,56.6747486948679,57.6616877957865,58.6486268967051,
59.6355659976236,60.6225050985422,61.6094441994608,62.5963833003793,63.5833224012979,
64.5702615022165,65.557200603135,66.5441397040536,67.5310788049722,68.5180179058908),
 .UNSPECIFIED.);
#356=B_SPLINE_SURFACE_WITH_KNOTS('',3,3,((#38027,#38028,#38029,#38030,#38031,
#38032,#38033,#38034,#38035,#38036,#38037,#38038,#38039,#38040,#38041,#38042,
#38043,#38044,#38045,#38046,#38047,#38048,#38049,#38050,#38051,#38052,#38053,
#38054,#38055,#38056,#38057,#38058,#38059,#38060,#38061,#38062,#38063,#38064,
#38065,#38066,#38067,#38068,#38069,#38070,#38071,#38072,#38073,#38074,#38075,
#38076,#38077,#38078,#38079,#38080,#38081,#38082,#38083,#38084,#38085,#38086,
#38087,#38088,#38089,#38090),(#38091,#38092,#38093,#38094,#38095,#38096,
#38097,#38098,#38099,#38100,#38101,#38102,#38103,#38104,#38105,#38106,#38107,
#38108,#38109,#38110,#38111,#38112,#38113,#38114,#38115,#38116,#38117,#38118,
#38119,#38120,#38121,#38122,#38123,#38124,#38125,#38126,#38127,#38128,#38129,
#38130,#38131,#38132,#38133,#38134,#38135,#38136,#38137,#38138,#38139,#38140,
#38141,#38142,#38143,#38144,#38145,#38146,#38147,#38148,#38149,#38150,#38151,
#38152,#38153,#38154),(#38155,#38156,#38157,#38158,#38159,#38160,#38161,
#38162,#38163,#38164,#38165,#38166,#38167,#38168,#38169,#38170,#38171,#38172,
#38173,#38174,#38175,#38176,#38177,#38178,#38179,#38180,#38181,#38182,#38183,
#38184,#38185,#38186,#38187,#38188,#38189,#38190,#38191,#38192,#38193,#38194,
#38195,#38196,#38197,#38198,#38199,#38200,#38201,#38202,#38203,#38204,#38205,
#38206,#38207,#38208,#38209,#38210,#38211,#38212,#38213,#38214,#38215,#38216,
#38217,#38218),(#38219,#38220,#38221,#38222,#38223,#38224,#38225,#38226,
#38227,#38228,#38229,#38230,#38231,#38232,#38233,#38234,#38235,#38236,#38237,
#38238,#38239,#38240,#38241,#38242,#38243,#38244,#38245,#38246,#38247,#38248,
#38249,#38250,#38251,#38252,#38253,#38254,#38255,#38256,#38257,#38258,#38259,
#38260,#38261,#38262,#38263,#38264,#38265,#38266,#38267,#38268,#38269,#38270,
#38271,#38272,#38273,#38274,#38275,#38276,#38277,#38278,#38279,#38280,#38281,
#38282)),.UNSPECIFIED.,.F.,.F.,.F.,(4,4),(4,1,1,1,1,1,1,1,1,1,1,1,1,1,1,
1,1,1,1,1,1,1,1,1,1,1,1,1,1,1,1,1,1,1,1,1,1,1,1,1,1,1,1,1,1,1,1,1,1,1,1,
1,1,1,1,1,1,1,1,1,1,4),(0.,0.0820126057383863),(11.6152142277547,12.6021533286733,
13.5890924295918,14.5760315305104,15.562970631429,16.5499097323475,17.5368488332661,
18.5237879341847,19.5107270351033,20.4976661360218,21.4846052369404,22.471544337859,
23.4584834387775,24.4454225396961,25.4323616406147,26.4193007415332,27.4062398424518,
28.3931789433704,29.380118044289,30.3670571452075,31.3539962461261,32.3409353470447,
33.3278744479632,34.3148135488818,35.3017526498004,36.2886917507189,37.2756308516375,
38.2625699525561,39.2495090534747,40.2364481543932,41.2233872553118,42.2103263562304,
43.1972654571489,44.1842045580675,45.1711436589861,46.1580827599046,47.1450218608232,
48.1319609617418,49.1189000626604,50.1058391635789,51.0927782644975,52.0797173654161,
53.0666564663346,54.0535955672532,55.0405346681718,56.0274737690903,57.0144128700089,
58.0013519709275,58.9882910718461,59.9752301727646,60.9621692736832,61.9491083746018,
62.9360474755203,63.9229865764389,64.9099256773575,65.8968647782761,66.8838038791946,
67.8707429801132,68.8576820810318,69.8446211819503,70.8315602828689,71.8184993837875),
 .UNSPECIFIED.);
#357=B_SPLINE_SURFACE_WITH_KNOTS('',3,3,((#41620,#41621,#41622,#41623,#41624,
#41625,#41626,#41627,#41628,#41629,#41630,#41631,#41632,#41633,#41634,#41635,
#41636,#41637,#41638,#41639,#41640,#41641,#41642,#41643,#41644,#41645,#41646,
#41647,#41648,#41649,#41650,#41651,#41652,#41653,#41654,#41655,#41656,#41657,
#41658,#41659,#41660,#41661,#41662,#41663,#41664,#41665,#41666,#41667,#41668,
#41669,#41670,#41671,#41672,#41673,#41674,#41675,#41676,#41677,#41678,#41679,
#41680,#41681,#41682,#41683,#41684,#41685,#41686,#41687,#41688,#41689,#41690,
#41691,#41692,#41693,#41694,#41695,#41696,#41697,#41698,#41699,#41700,#41701,
#41702,#41703,#41704,#41705,#41706,#41707,#41708,#41709,#41710,#41711,#41712,
#41713,#41714,#41715,#41716,#41717,#41718,#41719,#41720,#41721,#41722,#41723,
#41724,#41725,#41726,#41727,#41728,#41729,#41730,#41731,#41732,#41733,#41734,
#41735,#41736,#41737,#41738,#41739,#41740,#41741,#41742,#41743,#41744,#41745,
#41746,#41747,#41748,#41749,#41750,#41751,#41752,#41753,#41754,#41755,#41756,
#41757,#41758,#41759,#41760,#41761,#41762,#41763,#41764,#41765,#41766,#41767,
#41768,#41769,#41770,#41771,#41772,#41773,#41774,#41775,#41776,#41777,#41778,
#41779,#41780,#41781,#41782,#41783,#41784,#41785,#41786,#41787,#41788,#41789,
#41790,#41791,#41792,#41793,#41794,#41795,#41796,#41797,#41798,#41799,#41800,
#41801,#41802,#41803,#41804,#41805,#41806,#41807,#41808,#41809,#41810,#41811,
#41812,#41813,#41814,#41815,#41816,#41817,#41818,#41819,#41820,#41821,#41822,
#41823,#41824,#41825,#41826,#41827,#41828,#41829,#41830,#41831,#41832,#41833,
#41834,#41835,#41836,#41837,#41838,#41839,#41840,#41841,#41842,#41843,#41844,
#41845,#41846,#41847,#41848,#41849,#41850,#41851,#41852,#41853,#41854,#41855,
#41856,#41857,#41858,#41859,#41860,#41861,#41862,#41863,#41864,#41865,#41866,
#41867,#41868,#41869,#41870,#41871,#41872,#41873,#41874,#41875,#41876,#41877,
#41878,#41879,#41880,#41881,#41882,#41883,#41884,#41885,#41886,#41887,#41888,
#41889,#41890,#41891,#41892,#41893,#41894,#41895,#41896,#41897,#41898,#41899),
(#41900,#41901,#41902,#41903,#41904,#41905,#41906,#41907,#41908,#41909,
#41910,#41911,#41912,#41913,#41914,#41915,#41916,#41917,#41918,#41919,#41920,
#41921,#41922,#41923,#41924,#41925,#41926,#41927,#41928,#41929,#41930,#41931,
#41932,#41933,#41934,#41935,#41936,#41937,#41938,#41939,#41940,#41941,#41942,
#41943,#41944,#41945,#41946,#41947,#41948,#41949,#41950,#41951,#41952,#41953,
#41954,#41955,#41956,#41957,#41958,#41959,#41960,#41961,#41962,#41963,#41964,
#41965,#41966,#41967,#41968,#41969,#41970,#41971,#41972,#41973,#41974,#41975,
#41976,#41977,#41978,#41979,#41980,#41981,#41982,#41983,#41984,#41985,#41986,
#41987,#41988,#41989,#41990,#41991,#41992,#41993,#41994,#41995,#41996,#41997,
#41998,#41999,#42000,#42001,#42002,#42003,#42004,#42005,#42006,#42007,#42008,
#42009,#42010,#42011,#42012,#42013,#42014,#42015,#42016,#42017,#42018,#42019,
#42020,#42021,#42022,#42023,#42024,#42025,#42026,#42027,#42028,#42029,#42030,
#42031,#42032,#42033,#42034,#42035,#42036,#42037,#42038,#42039,#42040,#42041,
#42042,#42043,#42044,#42045,#42046,#42047,#42048,#42049,#42050,#42051,#42052,
#42053,#42054,#42055,#42056,#42057,#42058,#42059,#42060,#42061,#42062,#42063,
#42064,#42065,#42066,#42067,#42068,#42069,#42070,#42071,#42072,#42073,#42074,
#42075,#42076,#42077,#42078,#42079,#42080,#42081,#42082,#42083,#42084,#42085,
#42086,#42087,#42088,#42089,#42090,#42091,#42092,#42093,#42094,#42095,#42096,
#42097,#42098,#42099,#42100,#42101,#42102,#42103,#42104,#42105,#42106,#42107,
#42108,#42109,#42110,#42111,#42112,#42113,#42114,#42115,#42116,#42117,#42118,
#42119,#42120,#42121,#42122,#42123,#42124,#42125,#42126,#42127,#42128,#42129,
#42130,#42131,#42132,#42133,#42134,#42135,#42136,#42137,#42138,#42139,#42140,
#42141,#42142,#42143,#42144,#42145,#42146,#42147,#42148,#42149,#42150,#42151,
#42152,#42153,#42154,#42155,#42156,#42157,#42158,#42159,#42160,#42161,#42162,
#42163,#42164,#42165,#42166,#42167,#42168,#42169,#42170,#42171,#42172,#42173,
#42174,#42175,#42176,#42177,#42178,#42179),(#42180,#42181,#42182,#42183,
#42184,#42185,#42186,#42187,#42188,#42189,#42190,#42191,#42192,#42193,#42194,
#42195,#42196,#42197,#42198,#42199,#42200,#42201,#42202,#42203,#42204,#42205,
#42206,#42207,#42208,#42209,#42210,#42211,#42212,#42213,#42214,#42215,#42216,
#42217,#42218,#42219,#42220,#42221,#42222,#42223,#42224,#42225,#42226,#42227,
#42228,#42229,#42230,#42231,#42232,#42233,#42234,#42235,#42236,#42237,#42238,
#42239,#42240,#42241,#42242,#42243,#42244,#42245,#42246,#42247,#42248,#42249,
#42250,#42251,#42252,#42253,#42254,#42255,#42256,#42257,#42258,#42259,#42260,
#42261,#42262,#42263,#42264,#42265,#42266,#42267,#42268,#42269,#42270,#42271,
#42272,#42273,#42274,#42275,#42276,#42277,#42278,#42279,#42280,#42281,#42282,
#42283,#42284,#42285,#42286,#42287,#42288,#42289,#42290,#42291,#42292,#42293,
#42294,#42295,#42296,#42297,#42298,#42299,#42300,#42301,#42302,#42303,#42304,
#42305,#42306,#42307,#42308,#42309,#42310,#42311,#42312,#42313,#42314,#42315,
#42316,#42317,#42318,#42319,#42320,#42321,#42322,#42323,#42324,#42325,#42326,
#42327,#42328,#42329,#42330,#42331,#42332,#42333,#42334,#42335,#42336,#42337,
#42338,#42339,#42340,#42341,#42342,#42343,#42344,#42345,#42346,#42347,#42348,
#42349,#42350,#42351,#42352,#42353,#42354,#42355,#42356,#42357,#42358,#42359,
#42360,#42361,#42362,#42363,#42364,#42365,#42366,#42367,#42368,#42369,#42370,
#42371,#42372,#42373,#42374,#42375,#42376,#42377,#42378,#42379,#42380,#42381,
#42382,#42383,#42384,#42385,#42386,#42387,#42388,#42389,#42390,#42391,#42392,
#42393,#42394,#42395,#42396,#42397,#42398,#42399,#42400,#42401,#42402,#42403,
#42404,#42405,#42406,#42407,#42408,#42409,#42410,#42411,#42412,#42413,#42414,
#42415,#42416,#42417,#42418,#42419,#42420,#42421,#42422,#42423,#42424,#42425,
#42426,#42427,#42428,#42429,#42430,#42431,#42432,#42433,#42434,#42435,#42436,
#42437,#42438,#42439,#42440,#42441,#42442,#42443,#42444,#42445,#42446,#42447,
#42448,#42449,#42450,#42451,#42452,#42453,#42454,#42455,#42456,#42457,#42458,
#42459),(#42460,#42461,#42462,#42463,#42464,#42465,#42466,#42467,#42468,
#42469,#42470,#42471,#42472,#42473,#42474,#42475,#42476,#42477,#42478,#42479,
#42480,#42481,#42482,#42483,#42484,#42485,#42486,#42487,#42488,#42489,#42490,
#42491,#42492,#42493,#42494,#42495,#42496,#42497,#42498,#42499,#42500,#42501,
#42502,#42503,#42504,#42505,#42506,#42507,#42508,#42509,#42510,#42511,#42512,
#42513,#42514,#42515,#42516,#42517,#42518,#42519,#42520,#42521,#42522,#42523,
#42524,#42525,#42526,#42527,#42528,#42529,#42530,#42531,#42532,#42533,#42534,
#42535,#42536,#42537,#42538,#42539,#42540,#42541,#42542,#42543,#42544,#42545,
#42546,#42547,#42548,#42549,#42550,#42551,#42552,#42553,#42554,#42555,#42556,
#42557,#42558,#42559,#42560,#42561,#42562,#42563,#42564,#42565,#42566,#42567,
#42568,#42569,#42570,#42571,#42572,#42573,#42574,#42575,#42576,#42577,#42578,
#42579,#42580,#42581,#42582,#42583,#42584,#42585,#42586,#42587,#42588,#42589,
#42590,#42591,#42592,#42593,#42594,#42595,#42596,#42597,#42598,#42599,#42600,
#42601,#42602,#42603,#42604,#42605,#42606,#42607,#42608,#42609,#42610,#42611,
#42612,#42613,#42614,#42615,#42616,#42617,#42618,#42619,#42620,#42621,#42622,
#42623,#42624,#42625,#42626,#42627,#42628,#42629,#42630,#42631,#42632,#42633,
#42634,#42635,#42636,#42637,#42638,#42639,#42640,#42641,#42642,#42643,#42644,
#42645,#42646,#42647,#42648,#42649,#42650,#42651,#42652,#42653,#42654,#42655,
#42656,#42657,#42658,#42659,#42660,#42661,#42662,#42663,#42664,#42665,#42666,
#42667,#42668,#42669,#42670,#42671,#42672,#42673,#42674,#42675,#42676,#42677,
#42678,#42679,#42680,#42681,#42682,#42683,#42684,#42685,#42686,#42687,#42688,
#42689,#42690,#42691,#42692,#42693,#42694,#42695,#42696,#42697,#42698,#42699,
#42700,#42701,#42702,#42703,#42704,#42705,#42706,#42707,#42708,#42709,#42710,
#42711,#42712,#42713,#42714,#42715,#42716,#42717,#42718,#42719,#42720,#42721,
#42722,#42723,#42724,#42725,#42726,#42727,#42728,#42729,#42730,#42731,#42732,
#42733,#42734,#42735,#42736,#42737,#42738,#42739)),.UNSPECIFIED.,.F.,.F.,
 .F.,(4,4),(4,1,1,1,1,1,1,1,1,1,1,1,1,1,1,1,1,1,1,1,1,1,1,1,1,1,1,1,1,1,
1,1,1,1,1,1,1,1,1,1,1,1,1,1,1,1,1,1,1,1,1,1,1,1,1,1,1,1,1,1,1,1,1,1,1,1,
1,1,1,1,1,1,1,1,1,1,1,1,1,1,1,1,1,1,1,1,1,1,1,1,1,1,1,1,1,1,1,1,1,1,1,1,
1,1,1,1,1,1,1,1,1,1,1,1,1,1,1,1,1,1,1,1,1,1,1,1,1,1,1,1,1,1,1,1,1,1,1,1,
1,1,1,1,1,1,1,1,1,1,1,1,1,1,1,1,1,1,1,1,1,1,1,1,1,1,1,1,1,1,1,1,1,1,1,1,
1,1,1,1,1,1,1,1,1,1,1,1,1,1,1,1,1,1,1,1,1,1,1,1,1,1,1,1,1,1,1,1,1,1,1,1,
1,1,1,1,1,1,1,1,1,1,1,1,1,1,1,1,1,1,1,1,1,1,1,1,1,1,1,1,1,1,1,1,1,1,1,1,
1,1,1,1,1,1,1,1,1,1,1,1,1,1,1,1,1,1,1,1,1,1,1,1,1,1,1,1,1,1,1,4),(0.,0.0820126057383863),
(8.31473274985836,9.31236762250461,10.3100024951509,11.3076373677971,12.3052722404433,
13.3029071130896,14.3005419857358,15.2981768583821,16.2958117310283,17.2934466036746,
18.2910814763208,19.2887163489671,20.2863512216133,21.2839860942596,22.2816209669058,
23.2792558395521,24.2768907121983,25.2745255848446,26.2721604574908,27.2697953301371,
28.2674302027833,29.2650650754296,30.2626999480758,31.2603348207221,32.2579696933683,
33.2556045660146,34.2532394386608,35.2508743113071,36.2485091839533,37.2461440565995,
38.2437789292458,39.241413801892,40.2390486745383,41.2366835471845,42.2343184198308,
43.231953292477,44.2295881651233,45.2272230377695,46.2248579104158,47.222492783062,
48.2201276557083,49.2177625283545,50.2153974010008,51.213032273647,52.2106671462933,
53.2083020189395,54.2059368915858,55.203571764232,56.2012066368783,57.1988415095245,
58.1964763821708,59.194111254817,60.1917461274632,61.1893810001095,62.1870158727557,
63.184650745402,64.1822856180482,65.1799204906945,66.1775553633407,67.175190235987,
68.1728251086332,69.1704599812795,70.1680948539257,71.165729726572,72.1633645992182,
73.1609994718645,74.1586343445107,75.156269217157,76.1539040898032,77.1515389624495,
78.1491738350957,79.146808707742,80.1444435803882,81.1420784530345,82.1397133256807,
83.1373481983269,84.1349830709732,85.1326179436194,86.1302528162657,87.1278876889119,
88.1255225615582,89.1231574342044,90.1207923068507,91.1184271794969,92.1160620521432,
93.1136969247894,94.1113317974357,95.1089666700819,96.1066015427282,97.1042364153744,
98.1018712880207,99.0995061606669,100.097141033313,101.094775905959,102.092410778606,
103.090045651252,104.087680523898,105.085315396544,106.082950269191,107.080585141837,
108.078220014483,109.075854887129,110.073489759776,111.071124632422,112.068759505068,
113.066394377714,114.064029250361,115.061664123007,116.059298995653,117.056933868299,
118.054568740946,119.052203613592,120.049838486238,121.047473358884,122.045108231531,
123.042743104177,124.040377976823,125.038012849469,126.035647722116,127.033282594762,
128.030917467408,129.028552340054,130.026187212701,131.023822085347,132.021456957993,
133.019091830639,134.016726703286,135.014361575932,136.011996448578,137.009631321224,
138.007266193871,139.004901066517,140.002535939163,141.000170811809,141.997805684456,
142.995440557102,143.993075429748,144.990710302394,145.988345175041,146.985980047687,
147.983614920333,148.981249792979,149.978884665626,150.976519538272,151.974154410918,
152.971789283564,153.969424156211,154.967059028857,155.964693901503,156.962328774149,
157.959963646796,158.957598519442,159.955233392088,160.952868264734,161.950503137381,
162.948138010027,163.945772882673,164.943407755319,165.941042627966,166.938677500612,
167.936312373258,168.933947245904,169.931582118551,170.929216991197,171.926851863843,
172.924486736489,173.922121609136,174.919756481782,175.917391354428,176.915026227074,
177.912661099721,178.910295972367,179.907930845013,180.905565717659,181.903200590305,
182.900835462952,183.898470335598,184.896105208244,185.89374008089,186.891374953537,
187.889009826183,188.886644698829,189.884279571475,190.881914444122,191.879549316768,
192.877184189414,193.87481906206,194.872453934707,195.870088807353,196.867723679999,
197.865358552645,198.862993425292,199.860628297938,200.858263170584,201.85589804323,
202.853532915877,203.851167788523,204.848802661169,205.846437533815,206.844072406462,
207.841707279108,208.839342151754,209.8369770244,210.834611897047,211.832246769693,
212.829881642339,213.827516514985,214.825151387632,215.822786260278,216.820421132924,
217.81805600557,218.815690878217,219.813325750863,220.810960623509,221.808595496155,
222.806230368802,223.803865241448,224.801500114094,225.79913498674,226.796769859387,
227.794404732033,228.792039604679,229.789674477325,230.787309349972,231.784944222618,
232.782579095264,233.78021396791,234.777848840557,235.775483713203,236.773118585849,
237.770753458495,238.768388331142,239.766023203788,240.763658076434,241.76129294908,
242.758927821727,243.756562694373,244.754197567019,245.751832439665,246.749467312312,
247.747102184958,248.744737057604,249.74237193025,250.740006802897,251.737641675543,
252.735276548189,253.732911420835,254.730546293482,255.728181166128,256.725816038774,
257.72345091142,258.721085784067,259.718720656713,260.716355529359,261.713990402005,
262.711625274652,263.709260147298,264.706895019944,265.70452989259,266.702164765237,
267.699799637883,268.697434510529,269.695069383175,270.692704255822,271.690339128468,
272.687974001114,273.68560887376,274.683243746407,275.680878619053,276.678513491699,
277.676148364345,278.673783236992,279.671418109638,280.669052982284,281.66668785493,
282.664322727577,283.661957600223,284.659592472869),.UNSPECIFIED.);
#358=B_SPLINE_SURFACE_WITH_KNOTS('',3,3,((#43073,#43074,#43075,#43076,#43077,
#43078,#43079,#43080,#43081,#43082,#43083,#43084,#43085,#43086,#43087,#43088,
#43089,#43090,#43091,#43092,#43093,#43094,#43095,#43096,#43097,#43098,#43099,
#43100,#43101,#43102,#43103,#43104,#43105,#43106,#43107,#43108,#43109,#43110,
#43111,#43112,#43113,#43114,#43115,#43116,#43117,#43118,#43119,#43120,#43121,
#43122,#43123,#43124,#43125,#43126,#43127,#43128,#43129,#43130,#43131,#43132,
#43133,#43134,#43135,#43136,#43137,#43138,#43139,#43140,#43141,#43142,#43143,
#43144,#43145,#43146,#43147,#43148,#43149,#43150,#43151,#43152,#43153,#43154,
#43155,#43156,#43157,#43158,#43159,#43160,#43161,#43162,#43163,#43164,#43165,
#43166,#43167,#43168,#43169,#43170,#43171,#43172,#43173,#43174,#43175,#43176,
#43177,#43178,#43179,#43180,#43181,#43182,#43183,#43184,#43185,#43186,#43187,
#43188,#43189,#43190,#43191,#43192,#43193,#43194,#43195,#43196,#43197,#43198,
#43199,#43200,#43201,#43202,#43203,#43204,#43205,#43206,#43207,#43208,#43209,
#43210,#43211,#43212,#43213,#43214,#43215,#43216,#43217,#43218,#43219,#43220,
#43221,#43222,#43223,#43224,#43225,#43226,#43227,#43228,#43229,#43230,#43231,
#43232,#43233,#43234,#43235,#43236,#43237,#43238,#43239,#43240,#43241,#43242,
#43243,#43244,#43245,#43246,#43247,#43248,#43249,#43250,#43251,#43252,#43253,
#43254,#43255,#43256,#43257,#43258,#43259,#43260,#43261,#43262,#43263,#43264,
#43265,#43266,#43267,#43268,#43269,#43270,#43271,#43272,#43273,#43274,#43275,
#43276,#43277,#43278,#43279,#43280,#43281,#43282,#43283,#43284,#43285,#43286,
#43287,#43288,#43289,#43290,#43291,#43292,#43293,#43294,#43295,#43296,#43297,
#43298,#43299,#43300,#43301,#43302,#43303,#43304,#43305,#43306,#43307,#43308,
#43309,#43310,#43311,#43312,#43313,#43314,#43315,#43316,#43317,#43318,#43319,
#43320,#43321,#43322,#43323,#43324,#43325,#43326,#43327,#43328,#43329,#43330,
#43331,#43332,#43333,#43334,#43335,#43336,#43337,#43338,#43339,#43340,#43341,
#43342,#43343,#43344,#43345,#43346,#43347,#43348,#43349,#43350,#43351,#43352),
(#43353,#43354,#43355,#43356,#43357,#43358,#43359,#43360,#43361,#43362,
#43363,#43364,#43365,#43366,#43367,#43368,#43369,#43370,#43371,#43372,#43373,
#43374,#43375,#43376,#43377,#43378,#43379,#43380,#43381,#43382,#43383,#43384,
#43385,#43386,#43387,#43388,#43389,#43390,#43391,#43392,#43393,#43394,#43395,
#43396,#43397,#43398,#43399,#43400,#43401,#43402,#43403,#43404,#43405,#43406,
#43407,#43408,#43409,#43410,#43411,#43412,#43413,#43414,#43415,#43416,#43417,
#43418,#43419,#43420,#43421,#43422,#43423,#43424,#43425,#43426,#43427,#43428,
#43429,#43430,#43431,#43432,#43433,#43434,#43435,#43436,#43437,#43438,#43439,
#43440,#43441,#43442,#43443,#43444,#43445,#43446,#43447,#43448,#43449,#43450,
#43451,#43452,#43453,#43454,#43455,#43456,#43457,#43458,#43459,#43460,#43461,
#43462,#43463,#43464,#43465,#43466,#43467,#43468,#43469,#43470,#43471,#43472,
#43473,#43474,#43475,#43476,#43477,#43478,#43479,#43480,#43481,#43482,#43483,
#43484,#43485,#43486,#43487,#43488,#43489,#43490,#43491,#43492,#43493,#43494,
#43495,#43496,#43497,#43498,#43499,#43500,#43501,#43502,#43503,#43504,#43505,
#43506,#43507,#43508,#43509,#43510,#43511,#43512,#43513,#43514,#43515,#43516,
#43517,#43518,#43519,#43520,#43521,#43522,#43523,#43524,#43525,#43526,#43527,
#43528,#43529,#43530,#43531,#43532,#43533,#43534,#43535,#43536,#43537,#43538,
#43539,#43540,#43541,#43542,#43543,#43544,#43545,#43546,#43547,#43548,#43549,
#43550,#43551,#43552,#43553,#43554,#43555,#43556,#43557,#43558,#43559,#43560,
#43561,#43562,#43563,#43564,#43565,#43566,#43567,#43568,#43569,#43570,#43571,
#43572,#43573,#43574,#43575,#43576,#43577,#43578,#43579,#43580,#43581,#43582,
#43583,#43584,#43585,#43586,#43587,#43588,#43589,#43590,#43591,#43592,#43593,
#43594,#43595,#43596,#43597,#43598,#43599,#43600,#43601,#43602,#43603,#43604,
#43605,#43606,#43607,#43608,#43609,#43610,#43611,#43612,#43613,#43614,#43615,
#43616,#43617,#43618,#43619,#43620,#43621,#43622,#43623,#43624,#43625,#43626,
#43627,#43628,#43629,#43630,#43631,#43632),(#43633,#43634,#43635,#43636,
#43637,#43638,#43639,#43640,#43641,#43642,#43643,#43644,#43645,#43646,#43647,
#43648,#43649,#43650,#43651,#43652,#43653,#43654,#43655,#43656,#43657,#43658,
#43659,#43660,#43661,#43662,#43663,#43664,#43665,#43666,#43667,#43668,#43669,
#43670,#43671,#43672,#43673,#43674,#43675,#43676,#43677,#43678,#43679,#43680,
#43681,#43682,#43683,#43684,#43685,#43686,#43687,#43688,#43689,#43690,#43691,
#43692,#43693,#43694,#43695,#43696,#43697,#43698,#43699,#43700,#43701,#43702,
#43703,#43704,#43705,#43706,#43707,#43708,#43709,#43710,#43711,#43712,#43713,
#43714,#43715,#43716,#43717,#43718,#43719,#43720,#43721,#43722,#43723,#43724,
#43725,#43726,#43727,#43728,#43729,#43730,#43731,#43732,#43733,#43734,#43735,
#43736,#43737,#43738,#43739,#43740,#43741,#43742,#43743,#43744,#43745,#43746,
#43747,#43748,#43749,#43750,#43751,#43752,#43753,#43754,#43755,#43756,#43757,
#43758,#43759,#43760,#43761,#43762,#43763,#43764,#43765,#43766,#43767,#43768,
#43769,#43770,#43771,#43772,#43773,#43774,#43775,#43776,#43777,#43778,#43779,
#43780,#43781,#43782,#43783,#43784,#43785,#43786,#43787,#43788,#43789,#43790,
#43791,#43792,#43793,#43794,#43795,#43796,#43797,#43798,#43799,#43800,#43801,
#43802,#43803,#43804,#43805,#43806,#43807,#43808,#43809,#43810,#43811,#43812,
#43813,#43814,#43815,#43816,#43817,#43818,#43819,#43820,#43821,#43822,#43823,
#43824,#43825,#43826,#43827,#43828,#43829,#43830,#43831,#43832,#43833,#43834,
#43835,#43836,#43837,#43838,#43839,#43840,#43841,#43842,#43843,#43844,#43845,
#43846,#43847,#43848,#43849,#43850,#43851,#43852,#43853,#43854,#43855,#43856,
#43857,#43858,#43859,#43860,#43861,#43862,#43863,#43864,#43865,#43866,#43867,
#43868,#43869,#43870,#43871,#43872,#43873,#43874,#43875,#43876,#43877,#43878,
#43879,#43880,#43881,#43882,#43883,#43884,#43885,#43886,#43887,#43888,#43889,
#43890,#43891,#43892,#43893,#43894,#43895,#43896,#43897,#43898,#43899,#43900,
#43901,#43902,#43903,#43904,#43905,#43906,#43907,#43908,#43909,#43910,#43911,
#43912),(#43913,#43914,#43915,#43916,#43917,#43918,#43919,#43920,#43921,
#43922,#43923,#43924,#43925,#43926,#43927,#43928,#43929,#43930,#43931,#43932,
#43933,#43934,#43935,#43936,#43937,#43938,#43939,#43940,#43941,#43942,#43943,
#43944,#43945,#43946,#43947,#43948,#43949,#43950,#43951,#43952,#43953,#43954,
#43955,#43956,#43957,#43958,#43959,#43960,#43961,#43962,#43963,#43964,#43965,
#43966,#43967,#43968,#43969,#43970,#43971,#43972,#43973,#43974,#43975,#43976,
#43977,#43978,#43979,#43980,#43981,#43982,#43983,#43984,#43985,#43986,#43987,
#43988,#43989,#43990,#43991,#43992,#43993,#43994,#43995,#43996,#43997,#43998,
#43999,#44000,#44001,#44002,#44003,#44004,#44005,#44006,#44007,#44008,#44009,
#44010,#44011,#44012,#44013,#44014,#44015,#44016,#44017,#44018,#44019,#44020,
#44021,#44022,#44023,#44024,#44025,#44026,#44027,#44028,#44029,#44030,#44031,
#44032,#44033,#44034,#44035,#44036,#44037,#44038,#44039,#44040,#44041,#44042,
#44043,#44044,#44045,#44046,#44047,#44048,#44049,#44050,#44051,#44052,#44053,
#44054,#44055,#44056,#44057,#44058,#44059,#44060,#44061,#44062,#44063,#44064,
#44065,#44066,#44067,#44068,#44069,#44070,#44071,#44072,#44073,#44074,#44075,
#44076,#44077,#44078,#44079,#44080,#44081,#44082,#44083,#44084,#44085,#44086,
#44087,#44088,#44089,#44090,#44091,#44092,#44093,#44094,#44095,#44096,#44097,
#44098,#44099,#44100,#44101,#44102,#44103,#44104,#44105,#44106,#44107,#44108,
#44109,#44110,#44111,#44112,#44113,#44114,#44115,#44116,#44117,#44118,#44119,
#44120,#44121,#44122,#44123,#44124,#44125,#44126,#44127,#44128,#44129,#44130,
#44131,#44132,#44133,#44134,#44135,#44136,#44137,#44138,#44139,#44140,#44141,
#44142,#44143,#44144,#44145,#44146,#44147,#44148,#44149,#44150,#44151,#44152,
#44153,#44154,#44155,#44156,#44157,#44158,#44159,#44160,#44161,#44162,#44163,
#44164,#44165,#44166,#44167,#44168,#44169,#44170,#44171,#44172,#44173,#44174,
#44175,#44176,#44177,#44178,#44179,#44180,#44181,#44182,#44183,#44184,#44185,
#44186,#44187,#44188,#44189,#44190,#44191,#44192)),.UNSPECIFIED.,.F.,.F.,
 .F.,(4,4),(4,1,1,1,1,1,1,1,1,1,1,1,1,1,1,1,1,1,1,1,1,1,1,1,1,1,1,1,1,1,
1,1,1,1,1,1,1,1,1,1,1,1,1,1,1,1,1,1,1,1,1,1,1,1,1,1,1,1,1,1,1,1,1,1,1,1,
1,1,1,1,1,1,1,1,1,1,1,1,1,1,1,1,1,1,1,1,1,1,1,1,1,1,1,1,1,1,1,1,1,1,1,1,
1,1,1,1,1,1,1,1,1,1,1,1,1,1,1,1,1,1,1,1,1,1,1,1,1,1,1,1,1,1,1,1,1,1,1,1,
1,1,1,1,1,1,1,1,1,1,1,1,1,1,1,1,1,1,1,1,1,1,1,1,1,1,1,1,1,1,1,1,1,1,1,1,
1,1,1,1,1,1,1,1,1,1,1,1,1,1,1,1,1,1,1,1,1,1,1,1,1,1,1,1,1,1,1,1,1,1,1,1,
1,1,1,1,1,1,1,1,1,1,1,1,1,1,1,1,1,1,1,1,1,1,1,1,1,1,1,1,1,1,1,1,1,1,1,1,
1,1,1,1,1,1,1,1,1,1,1,1,1,1,1,1,1,1,1,1,1,1,1,1,1,1,1,1,1,1,1,4),(0.,0.0820126057383863),
(11.6152142277551,12.6128491004014,13.6104839730476,14.6081188456939,15.6057537183401,
16.6033885909864,17.6010234636326,18.5986583362789,19.5962932089251,20.5939280815713,
21.5915629542176,22.5891978268638,23.5868326995101,24.5844675721563,25.5821024448026,
26.5797373174488,27.5773721900951,28.5750070627413,29.5726419353876,30.5702768080338,
31.5679116806801,32.5655465533263,33.5631814259726,34.5608162986188,35.5584511712651,
36.5560860439113,37.5537209165576,38.5513557892038,39.54899066185,40.5466255344963,
41.5442604071425,42.5418952797888,43.539530152435,44.5371650250813,45.5347998977275,
46.5324347703738,47.53006964302,48.5277045156663,49.5253393883125,50.5229742609588,
51.520609133605,52.5182440062513,53.5158788788975,54.5135137515438,55.51114862419,
56.5087834968363,57.5064183694825,58.5040532421287,59.501688114775,60.4993229874212,
61.4969578600675,62.4945927327137,63.49222760536,64.4898624780062,65.4874973506525,
66.4851322232987,67.482767095945,68.4804019685912,69.4780368412375,70.4756717138837,
71.47330658653,72.4709414591762,73.4685763318225,74.4662112044687,75.463846077115,
76.4614809497612,77.4591158224074,78.4567506950537,79.4543855676999,80.4520204403462,
81.4496553129924,82.4472901856387,83.4449250582849,84.4425599309312,85.4401948035774,
86.4378296762237,87.4354645488699,88.4330994215162,89.4307342941624,90.4283691668087,
91.4260040394549,92.4236389121012,93.4212737847474,94.4189086573937,95.4165435300399,
96.4141784026861,97.4118132753324,98.4094481479786,99.4070830206249,100.404717893271,
101.402352765917,102.399987638564,103.39762251121,104.395257383856,105.392892256502,
106.390527129149,107.388162001795,108.385796874441,109.383431747087,110.381066619734,
111.37870149238,112.376336365026,113.373971237672,114.371606110319,115.369240982965,
116.366875855611,117.364510728257,118.362145600904,119.35978047355,120.357415346196,
121.355050218842,122.352685091489,123.350319964135,124.347954836781,125.345589709427,
126.343224582074,127.34085945472,128.338494327366,129.336129200012,130.333764072659,
131.331398945305,132.329033817951,133.326668690597,134.324303563244,135.32193843589,
136.319573308536,137.317208181182,138.314843053829,139.312477926475,140.310112799121,
141.307747671767,142.305382544414,143.30301741706,144.300652289706,145.298287162352,
146.295922034999,147.293556907645,148.291191780291,149.288826652937,150.286461525584,
151.28409639823,152.281731270876,153.279366143522,154.277001016168,155.274635888815,
156.272270761461,157.269905634107,158.267540506754,159.2651753794,160.262810252046,
161.260445124692,162.258079997338,163.255714869985,164.253349742631,165.250984615277,
166.248619487923,167.24625436057,168.243889233216,169.241524105862,170.239158978508,
171.236793851155,172.234428723801,173.232063596447,174.229698469093,175.22733334174,
176.224968214386,177.222603087032,178.220237959678,179.217872832325,180.215507704971,
181.213142577617,182.210777450263,183.20841232291,184.206047195556,185.203682068202,
186.201316940848,187.198951813495,188.196586686141,189.194221558787,190.191856431433,
191.18949130408,192.187126176726,193.184761049372,194.182395922018,195.180030794665,
196.177665667311,197.175300539957,198.172935412603,199.17057028525,200.168205157896,
201.165840030542,202.163474903188,203.161109775835,204.158744648481,205.156379521127,
206.154014393773,207.15164926642,208.149284139066,209.146919011712,210.144553884358,
211.142188757005,212.139823629651,213.137458502297,214.135093374943,215.13272824759,
216.130363120236,217.127997992882,218.125632865528,219.123267738175,220.120902610821,
221.118537483467,222.116172356113,223.11380722876,224.111442101406,225.109076974052,
226.106711846698,227.104346719345,228.101981591991,229.099616464637,230.097251337283,
231.09488620993,232.092521082576,233.090155955222,234.087790827868,235.085425700515,
236.083060573161,237.080695445807,238.078330318453,239.0759651911,240.073600063746,
241.071234936392,242.068869809038,243.066504681685,244.064139554331,245.061774426977,
246.059409299623,247.05704417227,248.054679044916,249.052313917562,250.049948790208,
251.047583662854,252.045218535501,253.042853408147,254.040488280793,255.038123153439,
256.035758026086,257.033392898732,258.031027771378,259.028662644024,260.026297516671,
261.023932389317,262.021567261963,263.019202134609,264.016837007256,265.014471879902,
266.012106752548,267.009741625194,268.007376497841,269.005011370487,270.002646243133,
271.000281115779,271.997915988426,272.995550861072,273.993185733718,274.990820606364,
275.988455479011,276.986090351657,277.983725224303,278.981360096949,279.978994969596,
280.976629842242,281.974264714888,282.971899587534,283.969534460181,284.967169332827,
285.964804205473,286.962439078119,287.960073950766),.UNSPECIFIED.);
#359=B_SPLINE_SURFACE_WITH_KNOTS('',3,3,((#50971,#50972,#50973,#50974,#50975,
#50976,#50977,#50978,#50979,#50980,#50981,#50982,#50983,#50984,#50985,#50986,
#50987,#50988,#50989,#50990,#50991,#50992,#50993,#50994,#50995,#50996,#50997,
#50998,#50999,#51000,#51001,#51002,#51003,#51004,#51005,#51006,#51007,#51008,
#51009,#51010,#51011,#51012,#51013,#51014,#51015,#51016,#51017,#51018,#51019,
#51020,#51021,#51022,#51023,#51024,#51025,#51026,#51027,#51028,#51029,#51030,
#51031,#51032,#51033,#51034,#51035,#51036,#51037,#51038,#51039,#51040,#51041,
#51042,#51043,#51044,#51045,#51046,#51047,#51048,#51049,#51050,#51051,#51052,
#51053,#51054,#51055,#51056,#51057,#51058,#51059,#51060,#51061,#51062,#51063,
#51064,#51065,#51066,#51067,#51068,#51069,#51070,#51071,#51072,#51073,#51074,
#51075,#51076,#51077,#51078,#51079,#51080,#51081,#51082,#51083,#51084,#51085,
#51086,#51087,#51088,#51089,#51090,#51091,#51092,#51093,#51094,#51095,#51096,
#51097,#51098,#51099,#51100,#51101,#51102,#51103,#51104,#51105,#51106,#51107,
#51108,#51109,#51110,#51111,#51112,#51113,#51114,#51115,#51116,#51117,#51118,
#51119,#51120,#51121,#51122,#51123,#51124,#51125,#51126,#51127,#51128,#51129,
#51130,#51131,#51132,#51133,#51134,#51135,#51136,#51137,#51138,#51139,#51140,
#51141,#51142,#51143,#51144,#51145,#51146,#51147,#51148,#51149,#51150,#51151,
#51152,#51153,#51154,#51155,#51156,#51157,#51158,#51159,#51160,#51161,#51162,
#51163,#51164,#51165,#51166,#51167,#51168,#51169,#51170,#51171,#51172,#51173,
#51174,#51175,#51176,#51177,#51178,#51179,#51180,#51181,#51182,#51183,#51184,
#51185,#51186,#51187,#51188,#51189,#51190,#51191,#51192,#51193,#51194,#51195,
#51196,#51197,#51198,#51199,#51200,#51201,#51202,#51203,#51204,#51205,#51206,
#51207,#51208,#51209,#51210,#51211,#51212,#51213,#51214,#51215,#51216,#51217,
#51218,#51219,#51220,#51221,#51222,#51223,#51224,#51225,#51226,#51227,#51228,
#51229,#51230,#51231,#51232,#51233,#51234,#51235,#51236,#51237,#51238,#51239,
#51240,#51241,#51242,#51243,#51244,#51245,#51246,#51247,#51248,#51249,#51250,
#51251,#51252,#51253,#51254,#51255,#51256,#51257,#51258,#51259,#51260,#51261,
#51262,#51263,#51264,#51265,#51266,#51267,#51268,#51269,#51270,#51271,#51272,
#51273,#51274,#51275,#51276,#51277,#51278,#51279,#51280,#51281,#51282,#51283,
#51284,#51285,#51286,#51287,#51288,#51289,#51290,#51291,#51292,#51293,#51294,
#51295,#51296,#51297,#51298,#51299,#51300,#51301,#51302,#51303,#51304,#51305,
#51306,#51307,#51308,#51309,#51310,#51311,#51312,#51313,#51314,#51315,#51316,
#51317,#51318,#51319,#51320,#51321,#51322,#51323,#51324,#51325,#51326,#51327,
#51328,#51329,#51330,#51331,#51332,#51333,#51334,#51335,#51336,#51337,#51338,
#51339,#51340,#51341,#51342,#51343,#51344,#51345,#51346,#51347,#51348,#51349,
#51350,#51351,#51352,#51353,#51354,#51355,#51356,#51357,#51358,#51359,#51360,
#51361,#51362,#51363,#51364,#51365,#51366,#51367,#51368,#51369,#51370,#51371,
#51372,#51373,#51374,#51375,#51376,#51377,#51378,#51379,#51380,#51381,#51382,
#51383,#51384,#51385,#51386,#51387,#51388,#51389,#51390,#51391,#51392,#51393,
#51394,#51395,#51396,#51397,#51398,#51399,#51400,#51401,#51402,#51403,#51404,
#51405,#51406,#51407,#51408,#51409,#51410,#51411,#51412,#51413,#51414,#51415,
#51416,#51417,#51418,#51419,#51420,#51421,#51422,#51423,#51424,#51425,#51426,
#51427,#51428,#51429,#51430,#51431,#51432,#51433,#51434,#51435,#51436,#51437,
#51438,#51439,#51440,#51441,#51442,#51443,#51444,#51445,#51446,#51447,#51448,
#51449,#51450,#51451,#51452,#51453,#51454,#51455,#51456,#51457,#51458,#51459,
#51460,#51461,#51462,#51463,#51464,#51465,#51466,#51467,#51468,#51469,#51470,
#51471,#51472,#51473,#51474,#51475,#51476,#51477,#51478,#51479,#51480,#51481,
#51482,#51483,#51484,#51485,#51486,#51487,#51488,#51489,#51490,#51491,#51492,
#51493,#51494,#51495,#51496,#51497,#51498,#51499,#51500,#51501,#51502,#51503,
#51504,#51505,#51506,#51507,#51508,#51509,#51510,#51511,#51512,#51513,#51514,
#51515,#51516,#51517,#51518,#51519,#51520,#51521,#51522,#51523,#51524,#51525,
#51526),(#51527,#51528,#51529,#51530,#51531,#51532,#51533,#51534,#51535,
#51536,#51537,#51538,#51539,#51540,#51541,#51542,#51543,#51544,#51545,#51546,
#51547,#51548,#51549,#51550,#51551,#51552,#51553,#51554,#51555,#51556,#51557,
#51558,#51559,#51560,#51561,#51562,#51563,#51564,#51565,#51566,#51567,#51568,
#51569,#51570,#51571,#51572,#51573,#51574,#51575,#51576,#51577,#51578,#51579,
#51580,#51581,#51582,#51583,#51584,#51585,#51586,#51587,#51588,#51589,#51590,
#51591,#51592,#51593,#51594,#51595,#51596,#51597,#51598,#51599,#51600,#51601,
#51602,#51603,#51604,#51605,#51606,#51607,#51608,#51609,#51610,#51611,#51612,
#51613,#51614,#51615,#51616,#51617,#51618,#51619,#51620,#51621,#51622,#51623,
#51624,#51625,#51626,#51627,#51628,#51629,#51630,#51631,#51632,#51633,#51634,
#51635,#51636,#51637,#51638,#51639,#51640,#51641,#51642,#51643,#51644,#51645,
#51646,#51647,#51648,#51649,#51650,#51651,#51652,#51653,#51654,#51655,#51656,
#51657,#51658,#51659,#51660,#51661,#51662,#51663,#51664,#51665,#51666,#51667,
#51668,#51669,#51670,#51671,#51672,#51673,#51674,#51675,#51676,#51677,#51678,
#51679,#51680,#51681,#51682,#51683,#51684,#51685,#51686,#51687,#51688,#51689,
#51690,#51691,#51692,#51693,#51694,#51695,#51696,#51697,#51698,#51699,#51700,
#51701,#51702,#51703,#51704,#51705,#51706,#51707,#51708,#51709,#51710,#51711,
#51712,#51713,#51714,#51715,#51716,#51717,#51718,#51719,#51720,#51721,#51722,
#51723,#51724,#51725,#51726,#51727,#51728,#51729,#51730,#51731,#51732,#51733,
#51734,#51735,#51736,#51737,#51738,#51739,#51740,#51741,#51742,#51743,#51744,
#51745,#51746,#51747,#51748,#51749,#51750,#51751,#51752,#51753,#51754,#51755,
#51756,#51757,#51758,#51759,#51760,#51761,#51762,#51763,#51764,#51765,#51766,
#51767,#51768,#51769,#51770,#51771,#51772,#51773,#51774,#51775,#51776,#51777,
#51778,#51779,#51780,#51781,#51782,#51783,#51784,#51785,#51786,#51787,#51788,
#51789,#51790,#51791,#51792,#51793,#51794,#51795,#51796,#51797,#51798,#51799,
#51800,#51801,#51802,#51803,#51804,#51805,#51806,#51807,#51808,#51809,#51810,
#51811,#51812,#51813,#51814,#51815,#51816,#51817,#51818,#51819,#51820,#51821,
#51822,#51823,#51824,#51825,#51826,#51827,#51828,#51829,#51830,#51831,#51832,
#51833,#51834,#51835,#51836,#51837,#51838,#51839,#51840,#51841,#51842,#51843,
#51844,#51845,#51846,#51847,#51848,#51849,#51850,#51851,#51852,#51853,#51854,
#51855,#51856,#51857,#51858,#51859,#51860,#51861,#51862,#51863,#51864,#51865,
#51866,#51867,#51868,#51869,#51870,#51871,#51872,#51873,#51874,#51875,#51876,
#51877,#51878,#51879,#51880,#51881,#51882,#51883,#51884,#51885,#51886,#51887,
#51888,#51889,#51890,#51891,#51892,#51893,#51894,#51895,#51896,#51897,#51898,
#51899,#51900,#51901,#51902,#51903,#51904,#51905,#51906,#51907,#51908,#51909,
#51910,#51911,#51912,#51913,#51914,#51915,#51916,#51917,#51918,#51919,#51920,
#51921,#51922,#51923,#51924,#51925,#51926,#51927,#51928,#51929,#51930,#51931,
#51932,#51933,#51934,#51935,#51936,#51937,#51938,#51939,#51940,#51941,#51942,
#51943,#51944,#51945,#51946,#51947,#51948,#51949,#51950,#51951,#51952,#51953,
#51954,#51955,#51956,#51957,#51958,#51959,#51960,#51961,#51962,#51963,#51964,
#51965,#51966,#51967,#51968,#51969,#51970,#51971,#51972,#51973,#51974,#51975,
#51976,#51977,#51978,#51979,#51980,#51981,#51982,#51983,#51984,#51985,#51986,
#51987,#51988,#51989,#51990,#51991,#51992,#51993,#51994,#51995,#51996,#51997,
#51998,#51999,#52000,#52001,#52002,#52003,#52004,#52005,#52006,#52007,#52008,
#52009,#52010,#52011,#52012,#52013,#52014,#52015,#52016,#52017,#52018,#52019,
#52020,#52021,#52022,#52023,#52024,#52025,#52026,#52027,#52028,#52029,#52030,
#52031,#52032,#52033,#52034,#52035,#52036,#52037,#52038,#52039,#52040,#52041,
#52042,#52043,#52044,#52045,#52046,#52047,#52048,#52049,#52050,#52051,#52052,
#52053,#52054,#52055,#52056,#52057,#52058,#52059,#52060,#52061,#52062,#52063,
#52064,#52065,#52066,#52067,#52068,#52069,#52070,#52071,#52072,#52073,#52074,
#52075,#52076,#52077,#52078,#52079,#52080,#52081,#52082),(#52083,#52084,
#52085,#52086,#52087,#52088,#52089,#52090,#52091,#52092,#52093,#52094,#52095,
#52096,#52097,#52098,#52099,#52100,#52101,#52102,#52103,#52104,#52105,#52106,
#52107,#52108,#52109,#52110,#52111,#52112,#52113,#52114,#52115,#52116,#52117,
#52118,#52119,#52120,#52121,#52122,#52123,#52124,#52125,#52126,#52127,#52128,
#52129,#52130,#52131,#52132,#52133,#52134,#52135,#52136,#52137,#52138,#52139,
#52140,#52141,#52142,#52143,#52144,#52145,#52146,#52147,#52148,#52149,#52150,
#52151,#52152,#52153,#52154,#52155,#52156,#52157,#52158,#52159,#52160,#52161,
#52162,#52163,#52164,#52165,#52166,#52167,#52168,#52169,#52170,#52171,#52172,
#52173,#52174,#52175,#52176,#52177,#52178,#52179,#52180,#52181,#52182,#52183,
#52184,#52185,#52186,#52187,#52188,#52189,#52190,#52191,#52192,#52193,#52194,
#52195,#52196,#52197,#52198,#52199,#52200,#52201,#52202,#52203,#52204,#52205,
#52206,#52207,#52208,#52209,#52210,#52211,#52212,#52213,#52214,#52215,#52216,
#52217,#52218,#52219,#52220,#52221,#52222,#52223,#52224,#52225,#52226,#52227,
#52228,#52229,#52230,#52231,#52232,#52233,#52234,#52235,#52236,#52237,#52238,
#52239,#52240,#52241,#52242,#52243,#52244,#52245,#52246,#52247,#52248,#52249,
#52250,#52251,#52252,#52253,#52254,#52255,#52256,#52257,#52258,#52259,#52260,
#52261,#52262,#52263,#52264,#52265,#52266,#52267,#52268,#52269,#52270,#52271,
#52272,#52273,#52274,#52275,#52276,#52277,#52278,#52279,#52280,#52281,#52282,
#52283,#52284,#52285,#52286,#52287,#52288,#52289,#52290,#52291,#52292,#52293,
#52294,#52295,#52296,#52297,#52298,#52299,#52300,#52301,#52302,#52303,#52304,
#52305,#52306,#52307,#52308,#52309,#52310,#52311,#52312,#52313,#52314,#52315,
#52316,#52317,#52318,#52319,#52320,#52321,#52322,#52323,#52324,#52325,#52326,
#52327,#52328,#52329,#52330,#52331,#52332,#52333,#52334,#52335,#52336,#52337,
#52338,#52339,#52340,#52341,#52342,#52343,#52344,#52345,#52346,#52347,#52348,
#52349,#52350,#52351,#52352,#52353,#52354,#52355,#52356,#52357,#52358,#52359,
#52360,#52361,#52362,#52363,#52364,#52365,#52366,#52367,#52368,#52369,#52370,
#52371,#52372,#52373,#52374,#52375,#52376,#52377,#52378,#52379,#52380,#52381,
#52382,#52383,#52384,#52385,#52386,#52387,#52388,#52389,#52390,#52391,#52392,
#52393,#52394,#52395,#52396,#52397,#52398,#52399,#52400,#52401,#52402,#52403,
#52404,#52405,#52406,#52407,#52408,#52409,#52410,#52411,#52412,#52413,#52414,
#52415,#52416,#52417,#52418,#52419,#52420,#52421,#52422,#52423,#52424,#52425,
#52426,#52427,#52428,#52429,#52430,#52431,#52432,#52433,#52434,#52435,#52436,
#52437,#52438,#52439,#52440,#52441,#52442,#52443,#52444,#52445,#52446,#52447,
#52448,#52449,#52450,#52451,#52452,#52453,#52454,#52455,#52456,#52457,#52458,
#52459,#52460,#52461,#52462,#52463,#52464,#52465,#52466,#52467,#52468,#52469,
#52470,#52471,#52472,#52473,#52474,#52475,#52476,#52477,#52478,#52479,#52480,
#52481,#52482,#52483,#52484,#52485,#52486,#52487,#52488,#52489,#52490,#52491,
#52492,#52493,#52494,#52495,#52496,#52497,#52498,#52499,#52500,#52501,#52502,
#52503,#52504,#52505,#52506,#52507,#52508,#52509,#52510,#52511,#52512,#52513,
#52514,#52515,#52516,#52517,#52518,#52519,#52520,#52521,#52522,#52523,#52524,
#52525,#52526,#52527,#52528,#52529,#52530,#52531,#52532,#52533,#52534,#52535,
#52536,#52537,#52538,#52539,#52540,#52541,#52542,#52543,#52544,#52545,#52546,
#52547,#52548,#52549,#52550,#52551,#52552,#52553,#52554,#52555,#52556,#52557,
#52558,#52559,#52560,#52561,#52562,#52563,#52564,#52565,#52566,#52567,#52568,
#52569,#52570,#52571,#52572,#52573,#52574,#52575,#52576,#52577,#52578,#52579,
#52580,#52581,#52582,#52583,#52584,#52585,#52586,#52587,#52588,#52589,#52590,
#52591,#52592,#52593,#52594,#52595,#52596,#52597,#52598,#52599,#52600,#52601,
#52602,#52603,#52604,#52605,#52606,#52607,#52608,#52609,#52610,#52611,#52612,
#52613,#52614,#52615,#52616,#52617,#52618,#52619,#52620,#52621,#52622,#52623,
#52624,#52625,#52626,#52627,#52628,#52629,#52630,#52631,#52632,#52633,#52634,
#52635,#52636,#52637,#52638),(#52639,#52640,#52641,#52642,#52643,#52644,
#52645,#52646,#52647,#52648,#52649,#52650,#52651,#52652,#52653,#52654,#52655,
#52656,#52657,#52658,#52659,#52660,#52661,#52662,#52663,#52664,#52665,#52666,
#52667,#52668,#52669,#52670,#52671,#52672,#52673,#52674,#52675,#52676,#52677,
#52678,#52679,#52680,#52681,#52682,#52683,#52684,#52685,#52686,#52687,#52688,
#52689,#52690,#52691,#52692,#52693,#52694,#52695,#52696,#52697,#52698,#52699,
#52700,#52701,#52702,#52703,#52704,#52705,#52706,#52707,#52708,#52709,#52710,
#52711,#52712,#52713,#52714,#52715,#52716,#52717,#52718,#52719,#52720,#52721,
#52722,#52723,#52724,#52725,#52726,#52727,#52728,#52729,#52730,#52731,#52732,
#52733,#52734,#52735,#52736,#52737,#52738,#52739,#52740,#52741,#52742,#52743,
#52744,#52745,#52746,#52747,#52748,#52749,#52750,#52751,#52752,#52753,#52754,
#52755,#52756,#52757,#52758,#52759,#52760,#52761,#52762,#52763,#52764,#52765,
#52766,#52767,#52768,#52769,#52770,#52771,#52772,#52773,#52774,#52775,#52776,
#52777,#52778,#52779,#52780,#52781,#52782,#52783,#52784,#52785,#52786,#52787,
#52788,#52789,#52790,#52791,#52792,#52793,#52794,#52795,#52796,#52797,#52798,
#52799,#52800,#52801,#52802,#52803,#52804,#52805,#52806,#52807,#52808,#52809,
#52810,#52811,#52812,#52813,#52814,#52815,#52816,#52817,#52818,#52819,#52820,
#52821,#52822,#52823,#52824,#52825,#52826,#52827,#52828,#52829,#52830,#52831,
#52832,#52833,#52834,#52835,#52836,#52837,#52838,#52839,#52840,#52841,#52842,
#52843,#52844,#52845,#52846,#52847,#52848,#52849,#52850,#52851,#52852,#52853,
#52854,#52855,#52856,#52857,#52858,#52859,#52860,#52861,#52862,#52863,#52864,
#52865,#52866,#52867,#52868,#52869,#52870,#52871,#52872,#52873,#52874,#52875,
#52876,#52877,#52878,#52879,#52880,#52881,#52882,#52883,#52884,#52885,#52886,
#52887,#52888,#52889,#52890,#52891,#52892,#52893,#52894,#52895,#52896,#52897,
#52898,#52899,#52900,#52901,#52902,#52903,#52904,#52905,#52906,#52907,#52908,
#52909,#52910,#52911,#52912,#52913,#52914,#52915,#52916,#52917,#52918,#52919,
#52920,#52921,#52922,#52923,#52924,#52925,#52926,#52927,#52928,#52929,#52930,
#52931,#52932,#52933,#52934,#52935,#52936,#52937,#52938,#52939,#52940,#52941,
#52942,#52943,#52944,#52945,#52946,#52947,#52948,#52949,#52950,#52951,#52952,
#52953,#52954,#52955,#52956,#52957,#52958,#52959,#52960,#52961,#52962,#52963,
#52964,#52965,#52966,#52967,#52968,#52969,#52970,#52971,#52972,#52973,#52974,
#52975,#52976,#52977,#52978,#52979,#52980,#52981,#52982,#52983,#52984,#52985,
#52986,#52987,#52988,#52989,#52990,#52991,#52992,#52993,#52994,#52995,#52996,
#52997,#52998,#52999,#53000,#53001,#53002,#53003,#53004,#53005,#53006,#53007,
#53008,#53009,#53010,#53011,#53012,#53013,#53014,#53015,#53016,#53017,#53018,
#53019,#53020,#53021,#53022,#53023,#53024,#53025,#53026,#53027,#53028,#53029,
#53030,#53031,#53032,#53033,#53034,#53035,#53036,#53037,#53038,#53039,#53040,
#53041,#53042,#53043,#53044,#53045,#53046,#53047,#53048,#53049,#53050,#53051,
#53052,#53053,#53054,#53055,#53056,#53057,#53058,#53059,#53060,#53061,#53062,
#53063,#53064,#53065,#53066,#53067,#53068,#53069,#53070,#53071,#53072,#53073,
#53074,#53075,#53076,#53077,#53078,#53079,#53080,#53081,#53082,#53083,#53084,
#53085,#53086,#53087,#53088,#53089,#53090,#53091,#53092,#53093,#53094,#53095,
#53096,#53097,#53098,#53099,#53100,#53101,#53102,#53103,#53104,#53105,#53106,
#53107,#53108,#53109,#53110,#53111,#53112,#53113,#53114,#53115,#53116,#53117,
#53118,#53119,#53120,#53121,#53122,#53123,#53124,#53125,#53126,#53127,#53128,
#53129,#53130,#53131,#53132,#53133,#53134,#53135,#53136,#53137,#53138,#53139,
#53140,#53141,#53142,#53143,#53144,#53145,#53146,#53147,#53148,#53149,#53150,
#53151,#53152,#53153,#53154,#53155,#53156,#53157,#53158,#53159,#53160,#53161,
#53162,#53163,#53164,#53165,#53166,#53167,#53168,#53169,#53170,#53171,#53172,
#53173,#53174,#53175,#53176,#53177,#53178,#53179,#53180,#53181,#53182,#53183,
#53184,#53185,#53186,#53187,#53188,#53189,#53190,#53191,#53192,#53193,#53194)),
 .UNSPECIFIED.,.F.,.F.,.F.,(4,4),(4,1,1,1,1,1,1,1,1,1,1,1,1,1,1,1,1,1,1,
1,1,1,1,1,1,1,1,1,1,1,1,1,1,1,1,1,1,1,1,1,1,1,1,1,1,1,1,1,1,1,1,1,1,1,1,
1,1,1,1,1,1,1,1,1,1,1,1,1,1,1,1,1,1,1,1,1,1,1,1,1,1,1,1,1,1,1,1,1,1,1,1,
1,1,1,1,1,1,1,1,1,1,1,1,1,1,1,1,1,1,1,1,1,1,1,1,1,1,1,1,1,1,1,1,1,1,1,1,
1,1,1,1,1,1,1,1,1,1,1,1,1,1,1,1,1,1,1,1,1,1,1,1,1,1,1,1,1,1,1,1,1,1,1,1,
1,1,1,1,1,1,1,1,1,1,1,1,1,1,1,1,1,1,1,1,1,1,1,1,1,1,1,1,1,1,1,1,1,1,1,1,
1,1,1,1,1,1,1,1,1,1,1,1,1,1,1,1,1,1,1,1,1,1,1,1,1,1,1,1,1,1,1,1,1,1,1,1,
1,1,1,1,1,1,1,1,1,1,1,1,1,1,1,1,1,1,1,1,1,1,1,1,1,1,1,1,1,1,1,1,1,1,1,1,
1,1,1,1,1,1,1,1,1,1,1,1,1,1,1,1,1,1,1,1,1,1,1,1,1,1,1,1,1,1,1,1,1,1,1,1,
1,1,1,1,1,1,1,1,1,1,1,1,1,1,1,1,1,1,1,1,1,1,1,1,1,1,1,1,1,1,1,1,1,1,1,1,
1,1,1,1,1,1,1,1,1,1,1,1,1,1,1,1,1,1,1,1,1,1,1,1,1,1,1,1,1,1,1,1,1,1,1,1,
1,1,1,1,1,1,1,1,1,1,1,1,1,1,1,1,1,1,1,1,1,1,1,1,1,1,1,1,1,1,1,1,1,1,1,1,
1,1,1,1,1,1,1,1,1,1,1,1,1,1,1,1,1,1,1,1,1,1,1,1,1,1,1,1,1,1,1,1,1,1,1,1,
1,1,1,1,1,1,1,1,1,1,1,1,1,1,1,1,1,1,1,1,1,1,1,1,1,1,1,1,1,1,1,1,1,1,1,1,
1,1,1,1,1,1,1,1,1,1,1,1,1,1,1,1,1,1,1,1,1,1,1,1,1,1,1,1,1,1,1,1,1,1,1,1,
1,1,1,1,1,1,1,1,1,1,1,1,1,1,1,1,1,1,1,1,1,1,1,1,1,1,1,1,1,1,4),(0.,0.0820126057383858),
(8.31473274985908,9.31438015173777,10.3140275536165,11.3136749554951,12.3133223573738,
13.3129697592525,14.3126171611312,15.3122645630099,16.3119119648886,17.3115593667672,
18.3112067686459,19.3108541705246,20.3105015724033,21.310148974282,22.3097963761607,
23.3094437780394,24.309091179918,25.3087385817967,26.3083859836754,27.3080333855541,
28.3076807874328,29.3073281893115,30.3069755911901,31.3066229930688,32.3062703949475,
33.3059177968262,34.3055651987049,35.3052126005836,36.3048600024622,37.3045074043409,
38.3041548062196,39.3038022080983,40.303449609977,41.3030970118557,42.3027444137344,
43.302391815613,44.3020392174917,45.3016866193704,46.3013340212491,47.3009814231278,
48.3006288250065,49.3002762268852,50.2999236287638,51.2995710306425,52.2992184325212,
53.2988658343999,54.2985132362786,55.2981606381573,56.2978080400359,57.2974554419146,
58.2971028437933,59.296750245672,60.2963976475507,61.2960450494294,62.295692451308,
63.2953398531867,64.2949872550654,65.2946346569441,66.2942820588228,67.2939294607015,
68.2935768625802,69.2932242644588,70.2928716663375,71.2925190682162,72.2921664700949,
73.2918138719736,74.2914612738523,75.291108675731,76.2907560776096,77.2904034794883,
78.290050881367,79.2896982832457,80.2893456851244,81.2889930870031,82.2886404888818,
83.2882878907604,84.2879352926391,85.2875826945178,86.2872300963965,87.2868774982752,
88.2865249001539,89.2861723020325,90.2858197039112,91.2854671057899,92.2851145076686,
93.2847619095473,94.2844093114259,95.2840567133046,96.2837041151833,97.283351517062,
98.2829989189407,99.2826463208194,100.282293722698,101.281941124577,102.281588526455,
103.281235928334,104.280883330213,105.280530732091,106.28017813397,107.279825535849,
108.279472937728,109.279120339606,110.278767741485,111.278415143364,112.278062545242,
113.277709947121,114.277357349,115.277004750878,116.276652152757,117.276299554636,
118.275946956514,119.275594358393,120.275241760272,121.27488916215,122.274536564029,
123.274183965908,124.273831367786,125.273478769665,126.273126171544,127.272773573423,
128.272420975301,129.27206837718,130.271715779059,131.271363180937,132.271010582816,
133.270657984695,134.270305386573,135.269952788452,136.269600190331,137.269247592209,
138.268894994088,139.268542395967,140.268189797845,141.267837199724,142.267484601603,
143.267132003481,144.26677940536,145.266426807239,146.266074209118,147.265721610996,
148.265369012875,149.265016414754,150.264663816632,151.264311218511,152.26395862039,
153.263606022268,154.263253424147,155.262900826026,156.262548227904,157.262195629783,
158.261843031662,159.26149043354,160.261137835419,161.260785237298,162.260432639177,
163.260080041055,164.259727442934,165.259374844813,166.259022246691,167.25866964857,
168.258317050449,169.257964452327,170.257611854206,171.257259256085,172.256906657963,
173.256554059842,174.256201461721,175.255848863599,176.255496265478,177.255143667357,
178.254791069235,179.254438471114,180.254085872993,181.253733274872,182.25338067675,
183.253028078629,184.252675480508,185.252322882386,186.251970284265,187.251617686144,
188.251265088022,189.250912489901,190.25055989178,191.250207293658,192.249854695537,
193.249502097416,194.249149499294,195.248796901173,196.248444303052,197.24809170493,
198.247739106809,199.247386508688,200.247033910567,201.246681312445,202.246328714324,
203.245976116203,204.245623518081,205.24527091996,206.244918321839,207.244565723717,
208.244213125596,209.243860527475,210.243507929353,211.243155331232,212.242802733111,
213.242450134989,214.242097536868,215.241744938747,216.241392340625,217.241039742504,
218.240687144383,219.240334546262,220.23998194814,221.239629350019,222.239276751898,
223.238924153776,224.238571555655,225.238218957534,226.237866359412,227.237513761291,
228.23716116317,229.236808565048,230.236455966927,231.236103368806,232.235750770684,
233.235398172563,234.235045574442,235.23469297632,236.234340378199,237.233987780078,
238.233635181957,239.233282583835,240.232929985714,241.232577387593,242.232224789471,
243.23187219135,244.231519593229,245.231166995107,246.230814396986,247.230461798865,
248.230109200743,249.229756602622,250.229404004501,251.229051406379,252.228698808258,
253.228346210137,254.227993612015,255.227641013894,256.227288415773,257.226935817652,
258.22658321953,259.226230621409,260.225878023288,261.225525425166,262.225172827045,
263.224820228924,264.224467630802,265.224115032681,266.22376243456,267.223409836438,
268.223057238317,269.222704640196,270.222352042074,271.221999443953,272.221646845832,
273.221294247711,274.220941649589,275.220589051468,276.220236453347,277.219883855225,
278.219531257104,279.219178658983,280.218826060861,281.21847346274,282.218120864619,
283.217768266497,284.217415668376,285.217063070255,286.216710472133,287.216357874012,
288.216005275891,289.215652677769,290.215300079648,291.214947481527,292.214594883406,
293.214242285284,294.213889687163,295.213537089042,296.21318449092,297.212831892799,
298.212479294678,299.212126696556,300.211774098435,301.211421500314,302.211068902192,
303.210716304071,304.21036370595,305.210011107828,306.209658509707,307.209305911586,
308.208953313464,309.208600715343,310.208248117222,311.207895519101,312.207542920979,
313.207190322858,314.206837724737,315.206485126615,316.206132528494,317.205779930373,
318.205427332251,319.20507473413,320.204722136009,321.204369537887,322.204016939766,
323.203664341645,324.203311743523,325.202959145402,326.202606547281,327.20225394916,
328.201901351038,329.201548752917,330.201196154796,331.200843556674,332.200490958553,
333.200138360432,334.19978576231,335.199433164189,336.199080566068,337.198727967946,
338.198375369825,339.198022771704,340.197670173582,341.197317575461,342.19696497734,
343.196612379218,344.196259781097,345.195907182976,346.195554584855,347.195201986733,
348.194849388612,349.194496790491,350.194144192369,351.193791594248,352.193438996127,
353.193086398005,354.192733799884,355.192381201763,356.192028603641,357.19167600552,
358.191323407399,359.190970809277,360.190618211156,361.190265613035,362.189913014913,
363.189560416792,364.189207818671,365.188855220549,366.188502622428,367.188150024307,
368.187797426186,369.187444828064,370.187092229943,371.186739631822,372.1863870337,
373.186034435579,374.185681837458,375.185329239336,376.184976641215,377.184624043094,
378.184271444972,379.183918846851,380.18356624873,381.183213650608,382.182861052487,
383.182508454366,384.182155856244,385.181803258123,386.181450660002,387.181098061881,
388.180745463759,389.180392865638,390.180040267517,391.179687669395,392.179335071274,
393.178982473153,394.178629875031,395.17827727691,396.177924678789,397.177572080667,
398.177219482546,399.176866884425,400.176514286303,401.176161688182,402.175809090061,
403.17545649194,404.175103893818,405.174751295697,406.174398697576,407.174046099454,
408.173693501333,409.173340903212,410.17298830509,411.172635706969,412.172283108848,
413.171930510726,414.171577912605,415.171225314484,416.170872716362,417.170520118241,
418.17016752012,419.169814921998,420.169462323877,421.169109725756,422.168757127635,
423.168404529513,424.168051931392,425.167699333271,426.167346735149,427.166994137028,
428.166641538907,429.166288940785,430.165936342664,431.165583744543,432.165231146421,
433.1648785483,434.164525950179,435.164173352057,436.163820753936,437.163468155815,
438.163115557694,439.162762959572,440.162410361451,441.16205776333,442.161705165208,
443.161352567087,444.160999968966,445.160647370844,446.160294772723,447.159942174602,
448.15958957648,449.159236978359,450.158884380238,451.158531782116,452.158179183995,
453.157826585874,454.157473987752,455.157121389631,456.15676879151,457.156416193389,
458.156063595267,459.155710997146,460.155358399025,461.155005800903,462.154653202782,
463.154300604661,464.153948006539,465.153595408418,466.153242810297,467.152890212175,
468.152537614054,469.152185015933,470.151832417811,471.15147981969,472.151127221569,
473.150774623447,474.150422025326,475.150069427205,476.149716829084,477.149364230962,
478.149011632841,479.14865903472,480.148306436598,481.147953838477,482.147601240356,
483.147248642234,484.146896044113,485.146543445992,486.14619084787,487.145838249749,
488.145485651628,489.145133053506,490.144780455385,491.144427857264,492.144075259142,
493.143722661021,494.1433700629,495.143017464778,496.142664866657,497.142312268536,
498.141959670415,499.141607072293,500.141254474172,501.140901876051,502.140549277929,
503.140196679808,504.139844081687,505.139491483565,506.139138885444,507.138786287323,
508.138433689201,509.13808109108,510.137728492959,511.137375894837,512.137023296716,
513.136670698595,514.136318100474,515.135965502352,516.135612904231,517.13526030611,
518.134907707988,519.134555109867,520.134202511746,521.133849913624,522.133497315503,
523.133144717382,524.13279211926,525.132439521139,526.132086923018,527.131734324896,
528.131381726775,529.131029128654,530.130676530532,531.130323932411,532.12997133429,
533.129618736168,534.129266138047,535.128913539926,536.128560941805,537.128208343683,
538.127855745562,539.127503147441,540.127150549319,541.126797951198,542.126445353077,
543.126092754955,544.125740156834,545.125387558713,546.125034960591,547.12468236247,
548.124329764349,549.123977166228,550.123624568106,551.123271969985,552.122919371864,
553.122566773742,554.122214175621,555.1218615775,556.121508979378,557.121156381257,
558.120803783136,559.120451185014,560.120098586893,561.119745988772),
 .UNSPECIFIED.);
#360=B_SPLINE_SURFACE_WITH_KNOTS('',3,3,((#53525,#53526,#53527,#53528,#53529,
#53530,#53531,#53532,#53533,#53534,#53535,#53536,#53537,#53538,#53539,#53540,
#53541,#53542,#53543,#53544,#53545,#53546,#53547,#53548,#53549,#53550,#53551,
#53552,#53553,#53554,#53555,#53556,#53557,#53558,#53559,#53560,#53561,#53562,
#53563,#53564,#53565,#53566,#53567,#53568,#53569,#53570,#53571,#53572,#53573,
#53574,#53575,#53576,#53577,#53578,#53579,#53580,#53581,#53582,#53583,#53584,
#53585,#53586,#53587,#53588,#53589,#53590,#53591,#53592,#53593,#53594,#53595,
#53596,#53597,#53598,#53599,#53600,#53601,#53602,#53603,#53604,#53605,#53606,
#53607,#53608,#53609,#53610,#53611,#53612,#53613,#53614,#53615,#53616,#53617,
#53618,#53619,#53620,#53621,#53622,#53623,#53624,#53625,#53626,#53627,#53628,
#53629,#53630,#53631,#53632,#53633,#53634,#53635,#53636,#53637,#53638,#53639,
#53640,#53641,#53642,#53643,#53644,#53645,#53646,#53647,#53648,#53649,#53650,
#53651,#53652,#53653,#53654,#53655,#53656,#53657,#53658,#53659,#53660,#53661,
#53662,#53663,#53664,#53665,#53666,#53667,#53668,#53669,#53670,#53671,#53672,
#53673,#53674,#53675,#53676,#53677,#53678,#53679,#53680,#53681,#53682,#53683,
#53684,#53685,#53686,#53687,#53688,#53689,#53690,#53691,#53692,#53693,#53694,
#53695,#53696,#53697,#53698,#53699,#53700,#53701,#53702,#53703,#53704,#53705,
#53706,#53707,#53708,#53709,#53710,#53711,#53712,#53713,#53714,#53715,#53716,
#53717,#53718,#53719,#53720,#53721,#53722,#53723,#53724,#53725,#53726,#53727,
#53728,#53729,#53730,#53731,#53732,#53733,#53734,#53735,#53736,#53737,#53738,
#53739,#53740,#53741,#53742,#53743,#53744,#53745,#53746,#53747,#53748,#53749,
#53750,#53751,#53752,#53753,#53754,#53755,#53756,#53757,#53758,#53759,#53760,
#53761,#53762,#53763,#53764,#53765,#53766,#53767,#53768,#53769,#53770,#53771,
#53772,#53773,#53774,#53775,#53776,#53777,#53778,#53779,#53780,#53781,#53782,
#53783,#53784,#53785,#53786,#53787,#53788,#53789,#53790,#53791,#53792,#53793,
#53794,#53795,#53796,#53797,#53798,#53799,#53800,#53801,#53802,#53803,#53804,
#53805,#53806,#53807,#53808,#53809,#53810,#53811,#53812,#53813,#53814,#53815,
#53816,#53817,#53818,#53819,#53820,#53821,#53822,#53823,#53824,#53825,#53826,
#53827,#53828,#53829,#53830,#53831,#53832,#53833,#53834,#53835,#53836,#53837,
#53838,#53839,#53840,#53841,#53842,#53843,#53844,#53845,#53846,#53847,#53848,
#53849,#53850,#53851,#53852,#53853,#53854,#53855,#53856,#53857,#53858,#53859,
#53860,#53861,#53862,#53863,#53864,#53865,#53866,#53867,#53868,#53869,#53870,
#53871,#53872,#53873,#53874,#53875,#53876,#53877,#53878,#53879,#53880,#53881,
#53882,#53883,#53884,#53885,#53886,#53887,#53888,#53889,#53890,#53891,#53892,
#53893,#53894,#53895,#53896,#53897,#53898,#53899,#53900,#53901,#53902,#53903,
#53904,#53905,#53906,#53907,#53908,#53909,#53910,#53911,#53912,#53913,#53914,
#53915,#53916,#53917,#53918,#53919,#53920,#53921,#53922,#53923,#53924,#53925,
#53926,#53927,#53928,#53929,#53930,#53931,#53932,#53933,#53934,#53935,#53936,
#53937,#53938,#53939,#53940,#53941,#53942,#53943,#53944,#53945,#53946,#53947,
#53948,#53949,#53950,#53951,#53952,#53953,#53954,#53955,#53956,#53957,#53958,
#53959,#53960,#53961,#53962,#53963,#53964,#53965,#53966,#53967,#53968,#53969,
#53970,#53971,#53972,#53973,#53974,#53975,#53976,#53977,#53978,#53979,#53980,
#53981,#53982,#53983,#53984,#53985,#53986,#53987,#53988,#53989,#53990,#53991,
#53992,#53993,#53994,#53995,#53996,#53997,#53998,#53999,#54000,#54001,#54002,
#54003,#54004,#54005,#54006,#54007,#54008,#54009,#54010,#54011,#54012,#54013,
#54014,#54015,#54016,#54017,#54018,#54019,#54020,#54021,#54022,#54023,#54024,
#54025,#54026,#54027,#54028,#54029,#54030,#54031,#54032,#54033,#54034,#54035,
#54036,#54037,#54038,#54039,#54040,#54041,#54042,#54043,#54044,#54045,#54046,
#54047,#54048,#54049,#54050,#54051,#54052,#54053,#54054,#54055,#54056,#54057,
#54058,#54059,#54060,#54061,#54062,#54063,#54064,#54065,#54066,#54067,#54068,
#54069,#54070,#54071,#54072,#54073,#54074,#54075,#54076,#54077,#54078,#54079,
#54080),(#54081,#54082,#54083,#54084,#54085,#54086,#54087,#54088,#54089,
#54090,#54091,#54092,#54093,#54094,#54095,#54096,#54097,#54098,#54099,#54100,
#54101,#54102,#54103,#54104,#54105,#54106,#54107,#54108,#54109,#54110,#54111,
#54112,#54113,#54114,#54115,#54116,#54117,#54118,#54119,#54120,#54121,#54122,
#54123,#54124,#54125,#54126,#54127,#54128,#54129,#54130,#54131,#54132,#54133,
#54134,#54135,#54136,#54137,#54138,#54139,#54140,#54141,#54142,#54143,#54144,
#54145,#54146,#54147,#54148,#54149,#54150,#54151,#54152,#54153,#54154,#54155,
#54156,#54157,#54158,#54159,#54160,#54161,#54162,#54163,#54164,#54165,#54166,
#54167,#54168,#54169,#54170,#54171,#54172,#54173,#54174,#54175,#54176,#54177,
#54178,#54179,#54180,#54181,#54182,#54183,#54184,#54185,#54186,#54187,#54188,
#54189,#54190,#54191,#54192,#54193,#54194,#54195,#54196,#54197,#54198,#54199,
#54200,#54201,#54202,#54203,#54204,#54205,#54206,#54207,#54208,#54209,#54210,
#54211,#54212,#54213,#54214,#54215,#54216,#54217,#54218,#54219,#54220,#54221,
#54222,#54223,#54224,#54225,#54226,#54227,#54228,#54229,#54230,#54231,#54232,
#54233,#54234,#54235,#54236,#54237,#54238,#54239,#54240,#54241,#54242,#54243,
#54244,#54245,#54246,#54247,#54248,#54249,#54250,#54251,#54252,#54253,#54254,
#54255,#54256,#54257,#54258,#54259,#54260,#54261,#54262,#54263,#54264,#54265,
#54266,#54267,#54268,#54269,#54270,#54271,#54272,#54273,#54274,#54275,#54276,
#54277,#54278,#54279,#54280,#54281,#54282,#54283,#54284,#54285,#54286,#54287,
#54288,#54289,#54290,#54291,#54292,#54293,#54294,#54295,#54296,#54297,#54298,
#54299,#54300,#54301,#54302,#54303,#54304,#54305,#54306,#54307,#54308,#54309,
#54310,#54311,#54312,#54313,#54314,#54315,#54316,#54317,#54318,#54319,#54320,
#54321,#54322,#54323,#54324,#54325,#54326,#54327,#54328,#54329,#54330,#54331,
#54332,#54333,#54334,#54335,#54336,#54337,#54338,#54339,#54340,#54341,#54342,
#54343,#54344,#54345,#54346,#54347,#54348,#54349,#54350,#54351,#54352,#54353,
#54354,#54355,#54356,#54357,#54358,#54359,#54360,#54361,#54362,#54363,#54364,
#54365,#54366,#54367,#54368,#54369,#54370,#54371,#54372,#54373,#54374,#54375,
#54376,#54377,#54378,#54379,#54380,#54381,#54382,#54383,#54384,#54385,#54386,
#54387,#54388,#54389,#54390,#54391,#54392,#54393,#54394,#54395,#54396,#54397,
#54398,#54399,#54400,#54401,#54402,#54403,#54404,#54405,#54406,#54407,#54408,
#54409,#54410,#54411,#54412,#54413,#54414,#54415,#54416,#54417,#54418,#54419,
#54420,#54421,#54422,#54423,#54424,#54425,#54426,#54427,#54428,#54429,#54430,
#54431,#54432,#54433,#54434,#54435,#54436,#54437,#54438,#54439,#54440,#54441,
#54442,#54443,#54444,#54445,#54446,#54447,#54448,#54449,#54450,#54451,#54452,
#54453,#54454,#54455,#54456,#54457,#54458,#54459,#54460,#54461,#54462,#54463,
#54464,#54465,#54466,#54467,#54468,#54469,#54470,#54471,#54472,#54473,#54474,
#54475,#54476,#54477,#54478,#54479,#54480,#54481,#54482,#54483,#54484,#54485,
#54486,#54487,#54488,#54489,#54490,#54491,#54492,#54493,#54494,#54495,#54496,
#54497,#54498,#54499,#54500,#54501,#54502,#54503,#54504,#54505,#54506,#54507,
#54508,#54509,#54510,#54511,#54512,#54513,#54514,#54515,#54516,#54517,#54518,
#54519,#54520,#54521,#54522,#54523,#54524,#54525,#54526,#54527,#54528,#54529,
#54530,#54531,#54532,#54533,#54534,#54535,#54536,#54537,#54538,#54539,#54540,
#54541,#54542,#54543,#54544,#54545,#54546,#54547,#54548,#54549,#54550,#54551,
#54552,#54553,#54554,#54555,#54556,#54557,#54558,#54559,#54560,#54561,#54562,
#54563,#54564,#54565,#54566,#54567,#54568,#54569,#54570,#54571,#54572,#54573,
#54574,#54575,#54576,#54577,#54578,#54579,#54580,#54581,#54582,#54583,#54584,
#54585,#54586,#54587,#54588,#54589,#54590,#54591,#54592,#54593,#54594,#54595,
#54596,#54597,#54598,#54599,#54600,#54601,#54602,#54603,#54604,#54605,#54606,
#54607,#54608,#54609,#54610,#54611,#54612,#54613,#54614,#54615,#54616,#54617,
#54618,#54619,#54620,#54621,#54622,#54623,#54624,#54625,#54626,#54627,#54628,
#54629,#54630,#54631,#54632,#54633,#54634,#54635,#54636),(#54637,#54638,
#54639,#54640,#54641,#54642,#54643,#54644,#54645,#54646,#54647,#54648,#54649,
#54650,#54651,#54652,#54653,#54654,#54655,#54656,#54657,#54658,#54659,#54660,
#54661,#54662,#54663,#54664,#54665,#54666,#54667,#54668,#54669,#54670,#54671,
#54672,#54673,#54674,#54675,#54676,#54677,#54678,#54679,#54680,#54681,#54682,
#54683,#54684,#54685,#54686,#54687,#54688,#54689,#54690,#54691,#54692,#54693,
#54694,#54695,#54696,#54697,#54698,#54699,#54700,#54701,#54702,#54703,#54704,
#54705,#54706,#54707,#54708,#54709,#54710,#54711,#54712,#54713,#54714,#54715,
#54716,#54717,#54718,#54719,#54720,#54721,#54722,#54723,#54724,#54725,#54726,
#54727,#54728,#54729,#54730,#54731,#54732,#54733,#54734,#54735,#54736,#54737,
#54738,#54739,#54740,#54741,#54742,#54743,#54744,#54745,#54746,#54747,#54748,
#54749,#54750,#54751,#54752,#54753,#54754,#54755,#54756,#54757,#54758,#54759,
#54760,#54761,#54762,#54763,#54764,#54765,#54766,#54767,#54768,#54769,#54770,
#54771,#54772,#54773,#54774,#54775,#54776,#54777,#54778,#54779,#54780,#54781,
#54782,#54783,#54784,#54785,#54786,#54787,#54788,#54789,#54790,#54791,#54792,
#54793,#54794,#54795,#54796,#54797,#54798,#54799,#54800,#54801,#54802,#54803,
#54804,#54805,#54806,#54807,#54808,#54809,#54810,#54811,#54812,#54813,#54814,
#54815,#54816,#54817,#54818,#54819,#54820,#54821,#54822,#54823,#54824,#54825,
#54826,#54827,#54828,#54829,#54830,#54831,#54832,#54833,#54834,#54835,#54836,
#54837,#54838,#54839,#54840,#54841,#54842,#54843,#54844,#54845,#54846,#54847,
#54848,#54849,#54850,#54851,#54852,#54853,#54854,#54855,#54856,#54857,#54858,
#54859,#54860,#54861,#54862,#54863,#54864,#54865,#54866,#54867,#54868,#54869,
#54870,#54871,#54872,#54873,#54874,#54875,#54876,#54877,#54878,#54879,#54880,
#54881,#54882,#54883,#54884,#54885,#54886,#54887,#54888,#54889,#54890,#54891,
#54892,#54893,#54894,#54895,#54896,#54897,#54898,#54899,#54900,#54901,#54902,
#54903,#54904,#54905,#54906,#54907,#54908,#54909,#54910,#54911,#54912,#54913,
#54914,#54915,#54916,#54917,#54918,#54919,#54920,#54921,#54922,#54923,#54924,
#54925,#54926,#54927,#54928,#54929,#54930,#54931,#54932,#54933,#54934,#54935,
#54936,#54937,#54938,#54939,#54940,#54941,#54942,#54943,#54944,#54945,#54946,
#54947,#54948,#54949,#54950,#54951,#54952,#54953,#54954,#54955,#54956,#54957,
#54958,#54959,#54960,#54961,#54962,#54963,#54964,#54965,#54966,#54967,#54968,
#54969,#54970,#54971,#54972,#54973,#54974,#54975,#54976,#54977,#54978,#54979,
#54980,#54981,#54982,#54983,#54984,#54985,#54986,#54987,#54988,#54989,#54990,
#54991,#54992,#54993,#54994,#54995,#54996,#54997,#54998,#54999,#55000,#55001,
#55002,#55003,#55004,#55005,#55006,#55007,#55008,#55009,#55010,#55011,#55012,
#55013,#55014,#55015,#55016,#55017,#55018,#55019,#55020,#55021,#55022,#55023,
#55024,#55025,#55026,#55027,#55028,#55029,#55030,#55031,#55032,#55033,#55034,
#55035,#55036,#55037,#55038,#55039,#55040,#55041,#55042,#55043,#55044,#55045,
#55046,#55047,#55048,#55049,#55050,#55051,#55052,#55053,#55054,#55055,#55056,
#55057,#55058,#55059,#55060,#55061,#55062,#55063,#55064,#55065,#55066,#55067,
#55068,#55069,#55070,#55071,#55072,#55073,#55074,#55075,#55076,#55077,#55078,
#55079,#55080,#55081,#55082,#55083,#55084,#55085,#55086,#55087,#55088,#55089,
#55090,#55091,#55092,#55093,#55094,#55095,#55096,#55097,#55098,#55099,#55100,
#55101,#55102,#55103,#55104,#55105,#55106,#55107,#55108,#55109,#55110,#55111,
#55112,#55113,#55114,#55115,#55116,#55117,#55118,#55119,#55120,#55121,#55122,
#55123,#55124,#55125,#55126,#55127,#55128,#55129,#55130,#55131,#55132,#55133,
#55134,#55135,#55136,#55137,#55138,#55139,#55140,#55141,#55142,#55143,#55144,
#55145,#55146,#55147,#55148,#55149,#55150,#55151,#55152,#55153,#55154,#55155,
#55156,#55157,#55158,#55159,#55160,#55161,#55162,#55163,#55164,#55165,#55166,
#55167,#55168,#55169,#55170,#55171,#55172,#55173,#55174,#55175,#55176,#55177,
#55178,#55179,#55180,#55181,#55182,#55183,#55184,#55185,#55186,#55187,#55188,
#55189,#55190,#55191,#55192),(#55193,#55194,#55195,#55196,#55197,#55198,
#55199,#55200,#55201,#55202,#55203,#55204,#55205,#55206,#55207,#55208,#55209,
#55210,#55211,#55212,#55213,#55214,#55215,#55216,#55217,#55218,#55219,#55220,
#55221,#55222,#55223,#55224,#55225,#55226,#55227,#55228,#55229,#55230,#55231,
#55232,#55233,#55234,#55235,#55236,#55237,#55238,#55239,#55240,#55241,#55242,
#55243,#55244,#55245,#55246,#55247,#55248,#55249,#55250,#55251,#55252,#55253,
#55254,#55255,#55256,#55257,#55258,#55259,#55260,#55261,#55262,#55263,#55264,
#55265,#55266,#55267,#55268,#55269,#55270,#55271,#55272,#55273,#55274,#55275,
#55276,#55277,#55278,#55279,#55280,#55281,#55282,#55283,#55284,#55285,#55286,
#55287,#55288,#55289,#55290,#55291,#55292,#55293,#55294,#55295,#55296,#55297,
#55298,#55299,#55300,#55301,#55302,#55303,#55304,#55305,#55306,#55307,#55308,
#55309,#55310,#55311,#55312,#55313,#55314,#55315,#55316,#55317,#55318,#55319,
#55320,#55321,#55322,#55323,#55324,#55325,#55326,#55327,#55328,#55329,#55330,
#55331,#55332,#55333,#55334,#55335,#55336,#55337,#55338,#55339,#55340,#55341,
#55342,#55343,#55344,#55345,#55346,#55347,#55348,#55349,#55350,#55351,#55352,
#55353,#55354,#55355,#55356,#55357,#55358,#55359,#55360,#55361,#55362,#55363,
#55364,#55365,#55366,#55367,#55368,#55369,#55370,#55371,#55372,#55373,#55374,
#55375,#55376,#55377,#55378,#55379,#55380,#55381,#55382,#55383,#55384,#55385,
#55386,#55387,#55388,#55389,#55390,#55391,#55392,#55393,#55394,#55395,#55396,
#55397,#55398,#55399,#55400,#55401,#55402,#55403,#55404,#55405,#55406,#55407,
#55408,#55409,#55410,#55411,#55412,#55413,#55414,#55415,#55416,#55417,#55418,
#55419,#55420,#55421,#55422,#55423,#55424,#55425,#55426,#55427,#55428,#55429,
#55430,#55431,#55432,#55433,#55434,#55435,#55436,#55437,#55438,#55439,#55440,
#55441,#55442,#55443,#55444,#55445,#55446,#55447,#55448,#55449,#55450,#55451,
#55452,#55453,#55454,#55455,#55456,#55457,#55458,#55459,#55460,#55461,#55462,
#55463,#55464,#55465,#55466,#55467,#55468,#55469,#55470,#55471,#55472,#55473,
#55474,#55475,#55476,#55477,#55478,#55479,#55480,#55481,#55482,#55483,#55484,
#55485,#55486,#55487,#55488,#55489,#55490,#55491,#55492,#55493,#55494,#55495,
#55496,#55497,#55498,#55499,#55500,#55501,#55502,#55503,#55504,#55505,#55506,
#55507,#55508,#55509,#55510,#55511,#55512,#55513,#55514,#55515,#55516,#55517,
#55518,#55519,#55520,#55521,#55522,#55523,#55524,#55525,#55526,#55527,#55528,
#55529,#55530,#55531,#55532,#55533,#55534,#55535,#55536,#55537,#55538,#55539,
#55540,#55541,#55542,#55543,#55544,#55545,#55546,#55547,#55548,#55549,#55550,
#55551,#55552,#55553,#55554,#55555,#55556,#55557,#55558,#55559,#55560,#55561,
#55562,#55563,#55564,#55565,#55566,#55567,#55568,#55569,#55570,#55571,#55572,
#55573,#55574,#55575,#55576,#55577,#55578,#55579,#55580,#55581,#55582,#55583,
#55584,#55585,#55586,#55587,#55588,#55589,#55590,#55591,#55592,#55593,#55594,
#55595,#55596,#55597,#55598,#55599,#55600,#55601,#55602,#55603,#55604,#55605,
#55606,#55607,#55608,#55609,#55610,#55611,#55612,#55613,#55614,#55615,#55616,
#55617,#55618,#55619,#55620,#55621,#55622,#55623,#55624,#55625,#55626,#55627,
#55628,#55629,#55630,#55631,#55632,#55633,#55634,#55635,#55636,#55637,#55638,
#55639,#55640,#55641,#55642,#55643,#55644,#55645,#55646,#55647,#55648,#55649,
#55650,#55651,#55652,#55653,#55654,#55655,#55656,#55657,#55658,#55659,#55660,
#55661,#55662,#55663,#55664,#55665,#55666,#55667,#55668,#55669,#55670,#55671,
#55672,#55673,#55674,#55675,#55676,#55677,#55678,#55679,#55680,#55681,#55682,
#55683,#55684,#55685,#55686,#55687,#55688,#55689,#55690,#55691,#55692,#55693,
#55694,#55695,#55696,#55697,#55698,#55699,#55700,#55701,#55702,#55703,#55704,
#55705,#55706,#55707,#55708,#55709,#55710,#55711,#55712,#55713,#55714,#55715,
#55716,#55717,#55718,#55719,#55720,#55721,#55722,#55723,#55724,#55725,#55726,
#55727,#55728,#55729,#55730,#55731,#55732,#55733,#55734,#55735,#55736,#55737,
#55738,#55739,#55740,#55741,#55742,#55743,#55744,#55745,#55746,#55747,#55748)),
 .UNSPECIFIED.,.F.,.F.,.F.,(4,4),(4,1,1,1,1,1,1,1,1,1,1,1,1,1,1,1,1,1,1,
1,1,1,1,1,1,1,1,1,1,1,1,1,1,1,1,1,1,1,1,1,1,1,1,1,1,1,1,1,1,1,1,1,1,1,1,
1,1,1,1,1,1,1,1,1,1,1,1,1,1,1,1,1,1,1,1,1,1,1,1,1,1,1,1,1,1,1,1,1,1,1,1,
1,1,1,1,1,1,1,1,1,1,1,1,1,1,1,1,1,1,1,1,1,1,1,1,1,1,1,1,1,1,1,1,1,1,1,1,
1,1,1,1,1,1,1,1,1,1,1,1,1,1,1,1,1,1,1,1,1,1,1,1,1,1,1,1,1,1,1,1,1,1,1,1,
1,1,1,1,1,1,1,1,1,1,1,1,1,1,1,1,1,1,1,1,1,1,1,1,1,1,1,1,1,1,1,1,1,1,1,1,
1,1,1,1,1,1,1,1,1,1,1,1,1,1,1,1,1,1,1,1,1,1,1,1,1,1,1,1,1,1,1,1,1,1,1,1,
1,1,1,1,1,1,1,1,1,1,1,1,1,1,1,1,1,1,1,1,1,1,1,1,1,1,1,1,1,1,1,1,1,1,1,1,
1,1,1,1,1,1,1,1,1,1,1,1,1,1,1,1,1,1,1,1,1,1,1,1,1,1,1,1,1,1,1,1,1,1,1,1,
1,1,1,1,1,1,1,1,1,1,1,1,1,1,1,1,1,1,1,1,1,1,1,1,1,1,1,1,1,1,1,1,1,1,1,1,
1,1,1,1,1,1,1,1,1,1,1,1,1,1,1,1,1,1,1,1,1,1,1,1,1,1,1,1,1,1,1,1,1,1,1,1,
1,1,1,1,1,1,1,1,1,1,1,1,1,1,1,1,1,1,1,1,1,1,1,1,1,1,1,1,1,1,1,1,1,1,1,1,
1,1,1,1,1,1,1,1,1,1,1,1,1,1,1,1,1,1,1,1,1,1,1,1,1,1,1,1,1,1,1,1,1,1,1,1,
1,1,1,1,1,1,1,1,1,1,1,1,1,1,1,1,1,1,1,1,1,1,1,1,1,1,1,1,1,1,1,1,1,1,1,1,
1,1,1,1,1,1,1,1,1,1,1,1,1,1,1,1,1,1,1,1,1,1,1,1,1,1,1,1,1,1,1,1,1,1,1,1,
1,1,1,1,1,1,1,1,1,1,1,1,1,1,1,1,1,1,1,1,1,1,1,1,1,1,1,1,1,1,4),(0.,0.0820126057383858),
(11.6152142277561,12.6148616296348,13.6145090315135,14.6141564333922,15.6138038352709,
16.6134512371495,17.6130986390282,18.6127460409069,19.6123934427856,20.6120408446643,
21.611688246543,22.6113356484216,23.6109830503003,24.610630452179,25.6102778540577,
26.6099252559364,27.6095726578151,28.6092200596937,29.6088674615724,30.6085148634511,
31.6081622653298,32.6078096672085,33.6074570690872,34.6071044709659,35.6067518728445,
36.6063992747232,37.6060466766019,38.6056940784806,39.6053414803593,40.604988882238,
41.6046362841166,42.6042836859953,43.603931087874,44.6035784897527,45.6032258916314,
46.6028732935101,47.6025206953887,48.6021680972674,49.6018154991461,50.6014629010248,
51.6011103029035,52.6007577047822,53.6004051066608,54.6000525085395,55.5996999104182,
56.5993473122969,57.5989947141756,58.5986421160543,59.5982895179329,60.5979369198116,
61.5975843216903,62.597231723569,63.5968791254477,64.5965265273264,65.5961739292051,
66.5958213310837,67.5954687329624,68.5951161348411,69.5947635367198,70.5944109385985,
71.5940583404772,72.5937057423558,73.5933531442345,74.5930005461132,75.5926479479919,
76.5922953498706,77.5919427517493,78.5915901536279,79.5912375555066,80.5908849573853,
81.590532359264,82.5901797611427,83.5898271630214,84.5894745649001,85.5891219667787,
86.5887693686574,87.5884167705361,88.5880641724148,89.5877115742935,90.5873589761722,
91.5870063780508,92.5866537799295,93.5863011818082,94.5859485836869,95.5855959855656,
96.5852433874443,97.5848907893229,98.5845381912016,99.5841855930803,100.583832994959,
101.583480396838,102.583127798716,103.582775200595,104.582422602474,105.582070004352,
106.581717406231,107.58136480811,108.581012209988,109.580659611867,110.580307013746,
111.579954415625,112.579601817503,113.579249219382,114.578896621261,115.578544023139,
116.578191425018,117.577838826897,118.577486228775,119.577133630654,120.576781032533,
121.576428434411,122.57607583629,123.575723238169,124.575370640047,125.575018041926,
126.574665443805,127.574312845683,128.573960247562,129.573607649441,130.57325505132,
131.572902453198,132.572549855077,133.572197256956,134.571844658834,135.571492060713,
136.571139462592,137.57078686447,138.570434266349,139.570081668228,140.569729070106,
141.569376471985,142.569023873864,143.568671275742,144.568318677621,145.5679660795,
146.567613481378,147.567260883257,148.566908285136,149.566555687014,150.566203088893,
151.565850490772,152.565497892651,153.565145294529,154.564792696408,155.564440098287,
156.564087500165,157.563734902044,158.563382303923,159.563029705801,160.56267710768,
161.562324509559,162.561971911437,163.561619313316,164.561266715195,165.560914117073,
166.560561518952,167.560208920831,168.559856322709,169.559503724588,170.559151126467,
171.558798528346,172.558445930224,173.558093332103,174.557740733982,175.55738813586,
176.557035537739,177.556682939618,178.556330341496,179.555977743375,180.555625145254,
181.555272547132,182.554919949011,183.55456735089,184.554214752768,185.553862154647,
186.553509556526,187.553156958405,188.552804360283,189.552451762162,190.552099164041,
191.551746565919,192.551393967798,193.551041369677,194.550688771555,195.550336173434,
196.549983575313,197.549630977191,198.54927837907,199.548925780949,200.548573182827,
201.548220584706,202.547867986585,203.547515388463,204.547162790342,205.546810192221,
206.5464575941,207.546104995978,208.545752397857,209.545399799736,210.545047201614,
211.544694603493,212.544342005372,213.54398940725,214.543636809129,215.543284211008,
216.542931612886,217.542579014765,218.542226416644,219.541873818522,220.541521220401,
221.54116862228,222.540816024158,223.540463426037,224.540110827916,225.539758229795,
226.539405631673,227.539053033552,228.538700435431,229.538347837309,230.537995239188,
231.537642641067,232.537290042945,233.536937444824,234.536584846703,235.536232248581,
236.53587965046,237.535527052339,238.535174454217,239.534821856096,240.534469257975,
241.534116659853,242.533764061732,243.533411463611,244.533058865489,245.532706267368,
246.532353669247,247.532001071126,248.531648473004,249.531295874883,250.530943276762,
251.53059067864,252.530238080519,253.529885482398,254.529532884276,255.529180286155,
256.528827688034,257.528475089912,258.528122491791,259.52776989367,260.527417295548,
261.527064697427,262.526712099306,263.526359501184,264.526006903063,265.525654304942,
266.525301706821,267.524949108699,268.524596510578,269.524243912457,270.523891314335,
271.523538716214,272.523186118093,273.522833519971,274.52248092185,275.522128323729,
276.521775725607,277.521423127486,278.521070529365,279.520717931243,280.520365333122,
281.520012735001,282.519660136879,283.519307538758,284.518954940637,285.518602342516,
286.518249744394,287.517897146273,288.517544548152,289.51719195003,290.516839351909,
291.516486753788,292.516134155666,293.515781557545,294.515428959424,295.515076361302,
296.514723763181,297.51437116506,298.514018566938,299.513665968817,300.513313370696,
301.512960772574,302.512608174453,303.512255576332,304.511902978211,305.511550380089,
306.511197781968,307.510845183847,308.510492585725,309.510139987604,310.509787389483,
311.509434791361,312.50908219324,313.508729595119,314.508376996997,315.508024398876,
316.507671800755,317.507319202633,318.506966604512,319.506614006391,320.506261408269,
321.505908810148,322.505556212027,323.505203613906,324.504851015784,325.504498417663,
326.504145819542,327.50379322142,328.503440623299,329.503088025178,330.502735427056,
331.502382828935,332.502030230814,333.501677632692,334.501325034571,335.50097243645,
336.500619838328,337.500267240207,338.499914642086,339.499562043964,340.499209445843,
341.498856847722,342.498504249601,343.498151651479,344.497799053358,345.497446455237,
346.497093857115,347.496741258994,348.496388660873,349.496036062751,350.49568346463,
351.495330866509,352.494978268387,353.494625670266,354.494273072145,355.493920474023,
356.493567875902,357.493215277781,358.492862679659,359.492510081538,360.492157483417,
361.491804885295,362.491452287174,363.491099689053,364.490747090932,365.49039449281,
366.490041894689,367.489689296568,368.489336698446,369.488984100325,370.488631502204,
371.488278904082,372.487926305961,373.48757370784,374.487221109718,375.486868511597,
376.486515913476,377.486163315354,378.485810717233,379.485458119112,380.48510552099,
381.484752922869,382.484400324748,383.484047726626,384.483695128505,385.483342530384,
386.482989932263,387.482637334141,388.48228473602,389.481932137899,390.481579539777,
391.481226941656,392.480874343535,393.480521745413,394.480169147292,395.479816549171,
396.479463951049,397.479111352928,398.478758754807,399.478406156685,400.478053558564,
401.477700960443,402.477348362322,403.4769957642,404.476643166079,405.476290567958,
406.475937969836,407.475585371715,408.475232773594,409.474880175472,410.474527577351,
411.47417497923,412.473822381108,413.473469782987,414.473117184866,415.472764586744,
416.472411988623,417.472059390502,418.47170679238,419.471354194259,420.471001596138,
421.470648998017,422.470296399895,423.469943801774,424.469591203653,425.469238605531,
426.46888600741,427.468533409289,428.468180811167,429.467828213046,430.467475614925,
431.467123016803,432.466770418682,433.466417820561,434.466065222439,435.465712624318,
436.465360026197,437.465007428075,438.464654829954,439.464302231833,440.463949633712,
441.46359703559,442.463244437469,443.462891839348,444.462539241226,445.462186643105,
446.461834044984,447.461481446862,448.461128848741,449.46077625062,450.460423652498,
451.460071054377,452.459718456256,453.459365858134,454.459013260013,455.458660661892,
456.45830806377,457.457955465649,458.457602867528,459.457250269407,460.456897671285,
461.456545073164,462.456192475043,463.455839876921,464.4554872788,465.455134680679,
466.454782082557,467.454429484436,468.454076886315,469.453724288193,470.453371690072,
471.453019091951,472.452666493829,473.452313895708,474.451961297587,475.451608699465,
476.451256101344,477.450903503223,478.450550905102,479.45019830698,480.449845708859,
481.449493110738,482.449140512616,483.448787914495,484.448435316374,485.448082718252,
486.447730120131,487.44737752201,488.447024923888,489.446672325767,490.446319727646,
491.445967129524,492.445614531403,493.445261933282,494.44490933516,495.444556737039,
496.444204138918,497.443851540797,498.443498942675,499.443146344554,500.442793746433,
501.442441148311,502.44208855019,503.441735952069,504.441383353947,505.441030755826,
506.440678157705,507.440325559583,508.439972961462,509.439620363341,510.439267765219,
511.438915167098,512.438562568977,513.438209970855,514.437857372734,515.437504774613,
516.437152176492,517.43679957837,518.436446980249,519.436094382128,520.435741784006,
521.435389185885,522.435036587764,523.434683989642,524.434331391521,525.4339787934,
526.433626195278,527.433273597157,528.432920999036,529.432568400914,530.432215802793,
531.431863204672,532.431510606551,533.431158008429,534.430805410308,535.430452812187,
536.430100214065,537.429747615944,538.429395017823,539.429042419701,540.42868982158,
541.428337223459,542.427984625337,543.427632027216,544.427279429095,545.426926830973,
546.426574232852,547.426221634731,548.425869036609,549.425516438488,550.425163840367,
551.424811242245,552.424458644124,553.424106046003,554.423753447881,555.42340084976,
556.423048251639,557.422695653518,558.422343055396,559.421990457275,560.421637859154,
561.421285261032,562.420932662911,563.42058006479,564.420227466668),
 .UNSPECIFIED.);
#361=B_SPLINE_SURFACE_WITH_KNOTS('',3,3,((#56136,#56137,#56138,#56139,#56140),
(#56141,#56142,#56143,#56144,#56145),(#56146,#56147,#56148,#56149,#56150),
(#56151,#56152,#56153,#56154,#56155)),.UNSPECIFIED.,.F.,.F.,.F.,(4,4),(4,
1,4),(0.,1.),(0.166194858401647,0.504344050522728,0.955209640017503),
 .UNSPECIFIED.);
#362=B_SPLINE_SURFACE_WITH_KNOTS('',3,3,((#56185,#56186,#56187,#56188,#56189),
(#56190,#56191,#56192,#56193,#56194),(#56195,#56196,#56197,#56198,#56199),
(#56200,#56201,#56202,#56203,#56204)),.UNSPECIFIED.,.F.,.F.,.F.,(4,4),(4,
1,4),(0.,1.),(0.166194858401647,0.504344050522728,0.955209640017503),
 .UNSPECIFIED.);
#363=B_SPLINE_SURFACE_WITH_KNOTS('',3,3,((#56274,#56275,#56276,#56277,#56278),
(#56279,#56280,#56281,#56282,#56283),(#56284,#56285,#56286,#56287,#56288),
(#56289,#56290,#56291,#56292,#56293)),.UNSPECIFIED.,.F.,.F.,.F.,(4,4),(4,
1,4),(0.,1.),(0.166194858401646,0.617060447896421,0.955209640017502),
 .UNSPECIFIED.);
#364=B_SPLINE_SURFACE_WITH_KNOTS('',3,3,((#56370,#56371,#56372,#56373,#56374),
(#56375,#56376,#56377,#56378,#56379),(#56380,#56381,#56382,#56383,#56384),
(#56385,#56386,#56387,#56388,#56389)),.UNSPECIFIED.,.F.,.F.,.F.,(4,4),(4,
1,4),(0.,1.),(0.166194858401647,0.617060447896421,0.955209640017502),
 .UNSPECIFIED.);
#365=B_SPLINE_SURFACE_WITH_KNOTS('',3,3,((#56403,#56404,#56405,#56406,#56407),
(#56408,#56409,#56410,#56411,#56412),(#56413,#56414,#56415,#56416,#56417),
(#56418,#56419,#56420,#56421,#56422)),.UNSPECIFIED.,.F.,.F.,.F.,(4,4),(4,
1,4),(0.,1.),(0.166194858401647,0.504344050522728,0.955209640017502),
 .UNSPECIFIED.);
#366=B_SPLINE_SURFACE_WITH_KNOTS('',3,3,((#56444,#56445,#56446,#56447,#56448),
(#56449,#56450,#56451,#56452,#56453),(#56454,#56455,#56456,#56457,#56458),
(#56459,#56460,#56461,#56462,#56463)),.UNSPECIFIED.,.F.,.F.,.F.,(4,4),(4,
1,4),(0.,1.),(0.166194858401646,0.504344050522728,0.955209640017502),
 .UNSPECIFIED.);
#367=TOROIDAL_SURFACE('',#17234,45.2410588351948,2.);
#368=TOROIDAL_SURFACE('',#17239,45.2410588351948,2.);
#369=TOROIDAL_SURFACE('',#17245,34.2759001296373,2.);
#370=TOROIDAL_SURFACE('',#17254,71.1954923578975,2.);
#371=TOROIDAL_SURFACE('',#17261,71.,2.);
#372=TOROIDAL_SURFACE('',#17269,71.1954923578975,2.);
#373=TOROIDAL_SURFACE('',#17276,71.,2.);
#374=TOROIDAL_SURFACE('',#17277,71.,2.);
#375=TOROIDAL_SURFACE('',#17288,6.,2.);
#376=TOROIDAL_SURFACE('',#17294,6.,2.);
#377=TOROIDAL_SURFACE('',#17306,6.00000000000001,2.);
#378=TOROIDAL_SURFACE('',#17311,6.,2.);
#379=TOROIDAL_SURFACE('',#17316,6.,2.);
#380=TOROIDAL_SURFACE('',#17321,6.,2.);
#381=TOROIDAL_SURFACE('',#17333,6.,2.);
#382=TOROIDAL_SURFACE('',#17335,6.00000000000001,2.);
#383=TOROIDAL_SURFACE('',#17340,51.1654934782503,2.);
#384=TOROIDAL_SURFACE('',#17354,6.,2.);
#385=TOROIDAL_SURFACE('',#17360,6.,2.);
#386=TOROIDAL_SURFACE('',#17371,6.05,2.);
#387=TOROIDAL_SURFACE('',#17373,6.00000000000001,2.);
#388=TOROIDAL_SURFACE('',#17379,6.,2.);
#389=TOROIDAL_SURFACE('',#17384,6.,2.);
#390=TOROIDAL_SURFACE('',#17388,6.,2.);
#391=TOROIDAL_SURFACE('',#17398,6.00000000000001,2.);
#392=TOROIDAL_SURFACE('',#17403,6.,2.);
#393=TOROIDAL_SURFACE('',#17412,6.05,2.);
#394=TOROIDAL_SURFACE('',#17838,15.5,1.5);
#395=TOROIDAL_SURFACE('',#17844,15.5,1.5);
#396=TOROIDAL_SURFACE('',#17849,15.5,1.5);
#397=TOROIDAL_SURFACE('',#17858,15.5,1.5);
#398=TOROIDAL_SURFACE('',#17866,4.5,1.5);
#399=TOROIDAL_SURFACE('',#17872,4.50000000000001,1.5);
#400=TOROIDAL_SURFACE('',#17878,4.50000000000001,1.5);
#401=TOROIDAL_SURFACE('',#17884,4.5,1.5);
#402=TOROIDAL_SURFACE('',#17901,4.5,1.5);
#403=TOROIDAL_SURFACE('',#17906,4.50000000000001,1.5);
#404=TOROIDAL_SURFACE('',#17911,4.50000000000001,1.5);
#405=TOROIDAL_SURFACE('',#17917,4.5,1.5);
#406=TOROIDAL_SURFACE('',#17929,4.50000000000001,1.5);
#407=TOROIDAL_SURFACE('',#17935,4.5,1.5);
#408=TOROIDAL_SURFACE('',#17941,4.5,1.5);
#409=TOROIDAL_SURFACE('',#17947,4.50000000000001,1.5);
#410=TOROIDAL_SURFACE('',#17964,4.50000000000001,1.5);
#411=TOROIDAL_SURFACE('',#17969,4.5,1.5);
#412=TOROIDAL_SURFACE('',#17974,4.5,1.5);
#413=TOROIDAL_SURFACE('',#17980,4.50000000000001,1.5);
#414=FACE_BOUND('',#2788,.T.);
#415=FACE_BOUND('',#2789,.T.);
#416=FACE_BOUND('',#2790,.T.);
#417=FACE_BOUND('',#2794,.T.);
#418=FACE_BOUND('',#2795,.T.);
#419=FACE_BOUND('',#2796,.T.);
#420=FACE_BOUND('',#2807,.T.);
#421=FACE_BOUND('',#2808,.T.);
#422=FACE_BOUND('',#2809,.T.);
#423=FACE_BOUND('',#2810,.T.);
#424=FACE_BOUND('',#2811,.T.);
#425=FACE_BOUND('',#2812,.T.);
#426=FACE_BOUND('',#2815,.T.);
#427=FACE_BOUND('',#2816,.T.);
#428=FACE_BOUND('',#2817,.T.);
#429=FACE_BOUND('',#2822,.T.);
#430=FACE_BOUND('',#2823,.T.);
#431=FACE_BOUND('',#2824,.T.);
#432=FACE_BOUND('',#2828,.T.);
#433=FACE_BOUND('',#2829,.T.);
#434=FACE_BOUND('',#2830,.T.);
#435=FACE_BOUND('',#2831,.T.);
#436=FACE_BOUND('',#2832,.T.);
#437=FACE_BOUND('',#2833,.T.);
#438=FACE_BOUND('',#2834,.T.);
#439=FACE_BOUND('',#2922,.T.);
#440=FACE_BOUND('',#2925,.T.);
#441=FACE_BOUND('',#2927,.T.);
#442=FACE_BOUND('',#2951,.T.);
#443=FACE_BOUND('',#2956,.T.);
#444=FACE_BOUND('',#2958,.T.);
#445=FACE_BOUND('',#2959,.T.);
#446=FACE_BOUND('',#2960,.T.);
#447=FACE_BOUND('',#2961,.T.);
#448=FACE_BOUND('',#2962,.T.);
#449=FACE_BOUND('',#2963,.T.);
#450=FACE_BOUND('',#2964,.T.);
#451=FACE_BOUND('',#2974,.T.);
#452=FACE_BOUND('',#2978,.T.);
#453=FACE_BOUND('',#2979,.T.);
#454=FACE_BOUND('',#2980,.T.);
#455=FACE_BOUND('',#2981,.T.);
#456=FACE_BOUND('',#2982,.T.);
#457=FACE_BOUND('',#2983,.T.);
#458=FACE_BOUND('',#2984,.T.);
#459=FACE_BOUND('',#2990,.T.);
#460=FACE_BOUND('',#2994,.T.);
#461=FACE_BOUND('',#2995,.T.);
#462=FACE_BOUND('',#2996,.T.);
#463=FACE_BOUND('',#2997,.T.);
#464=FACE_BOUND('',#2998,.T.);
#465=FACE_BOUND('',#2999,.T.);
#466=FACE_BOUND('',#3000,.T.);
#467=FACE_BOUND('',#3002,.T.);
#468=FACE_BOUND('',#3015,.T.);
#469=FACE_BOUND('',#3016,.T.);
#470=FACE_BOUND('',#3017,.T.);
#471=FACE_BOUND('',#3018,.T.);
#472=FACE_BOUND('',#3019,.T.);
#473=FACE_BOUND('',#3020,.T.);
#474=FACE_BOUND('',#3021,.T.);
#475=FACE_BOUND('',#3025,.T.);
#476=FACE_BOUND('',#3034,.T.);
#477=FACE_BOUND('',#3035,.T.);
#478=FACE_BOUND('',#3036,.T.);
#479=FACE_BOUND('',#3037,.T.);
#480=FACE_BOUND('',#3038,.T.);
#481=FACE_BOUND('',#3039,.T.);
#482=FACE_BOUND('',#3040,.T.);
#483=FACE_BOUND('',#3043,.T.);
#484=FACE_BOUND('',#3044,.T.);
#485=FACE_BOUND('',#3045,.T.);
#486=FACE_BOUND('',#3046,.T.);
#487=FACE_BOUND('',#3047,.T.);
#488=FACE_BOUND('',#3048,.T.);
#489=FACE_BOUND('',#3049,.T.);
#490=FACE_BOUND('',#3058,.T.);
#491=FACE_BOUND('',#3061,.T.);
#492=FACE_BOUND('',#3062,.T.);
#493=FACE_BOUND('',#3063,.T.);
#494=FACE_BOUND('',#3064,.T.);
#495=FACE_BOUND('',#3065,.T.);
#496=FACE_BOUND('',#3066,.T.);
#497=FACE_BOUND('',#3067,.T.);
#498=FACE_BOUND('',#3070,.T.);
#499=FACE_BOUND('',#3071,.T.);
#500=FACE_BOUND('',#3072,.T.);
#501=FACE_BOUND('',#3073,.T.);
#502=FACE_BOUND('',#3074,.T.);
#503=FACE_BOUND('',#3075,.T.);
#504=FACE_BOUND('',#3076,.T.);
#505=FACE_BOUND('',#3079,.T.);
#506=FACE_BOUND('',#3082,.T.);
#507=FACE_BOUND('',#3087,.T.);
#508=FACE_BOUND('',#3090,.T.);
#509=FACE_BOUND('',#3095,.T.);
#510=FACE_BOUND('',#3171,.T.);
#511=FACE_BOUND('',#3174,.T.);
#512=FACE_BOUND('',#3188,.T.);
#513=FACE_BOUND('',#3215,.T.);
#514=FACE_BOUND('',#3218,.T.);
#515=FACE_BOUND('',#3222,.T.);
#516=FACE_BOUND('',#3228,.T.);
#517=FACE_BOUND('',#3232,.T.);
#518=FACE_BOUND('',#3235,.T.);
#519=FACE_BOUND('',#3248,.T.);
#520=FACE_BOUND('',#3250,.T.);
#521=FACE_BOUND('',#3251,.T.);
#522=FACE_BOUND('',#3252,.T.);
#523=FACE_BOUND('',#3265,.T.);
#524=FACE_BOUND('',#3266,.T.);
#525=FACE_BOUND('',#3279,.T.);
#526=FACE_BOUND('',#3281,.T.);
#527=FACE_BOUND('',#3282,.T.);
#528=FACE_BOUND('',#3283,.T.);
#529=FACE_BOUND('',#3296,.T.);
#530=FACE_BOUND('',#3297,.T.);
#531=FACE_BOUND('',#3310,.T.);
#532=FACE_BOUND('',#3312,.T.);
#533=FACE_BOUND('',#3315,.T.);
#534=FACE_BOUND('',#3333,.T.);
#535=FACE_BOUND('',#3338,.T.);
#536=FACE_BOUND('',#3360,.T.);
#537=FACE_BOUND('',#3383,.T.);
#538=FACE_BOUND('',#3390,.T.);
#539=FACE_BOUND('',#3422,.T.);
#540=FACE_BOUND('',#3431,.T.);
#541=FACE_BOUND('',#3433,.T.);
#542=FACE_BOUND('',#3435,.T.);
#543=FACE_BOUND('',#3439,.T.);
#544=FACE_BOUND('',#3441,.T.);
#545=FACE_BOUND('',#3452,.T.);
#546=FACE_BOUND('',#3457,.T.);
#547=FACE_BOUND('',#3460,.T.);
#548=FACE_BOUND('',#3461,.T.);
#549=FACE_BOUND('',#3462,.T.);
#550=FACE_BOUND('',#3463,.T.);
#551=FACE_BOUND('',#3464,.T.);
#552=FACE_BOUND('',#3465,.T.);
#553=FACE_BOUND('',#3493,.T.);
#554=FACE_BOUND('',#3494,.T.);
#555=FACE_BOUND('',#3495,.T.);
#556=FACE_BOUND('',#3496,.T.);
#557=FACE_BOUND('',#3497,.T.);
#558=FACE_BOUND('',#3498,.T.);
#559=FACE_BOUND('',#3561,.T.);
#560=FACE_BOUND('',#3661,.T.);
#561=FACE_BOUND('',#3854,.T.);
#562=FACE_BOUND('',#3873,.T.);
#563=FACE_BOUND('',#3900,.T.);
#564=CONICAL_SURFACE('',#17208,4.3,0.785398163397448);
#565=CONICAL_SURFACE('',#17217,4.3,0.785398163397448);
#566=CONICAL_SURFACE('',#17218,4.3,0.785398163397439);
#567=CONICAL_SURFACE('',#17230,4.3,0.785398163397439);
#568=CONICAL_SURFACE('',#17237,50.,0.272145890531187);
#569=CONICAL_SURFACE('',#17243,50.,0.272145890531187);
#570=CONICAL_SURFACE('',#17250,41.,0.876058050598193);
#571=CONICAL_SURFACE('',#17344,47.,0.477345382373672);
#572=CONICAL_SURFACE('',#17465,38.,0.785398163397448);
#573=CONICAL_SURFACE('',#17486,10.9267766952966,1.17809724509617);
#574=CONICAL_SURFACE('',#17489,11.5,0.785398163397449);
#575=CONICAL_SURFACE('',#17493,11.8232233047034,0.392699081698727);
#576=CONICAL_SURFACE('',#17496,69.7,0.785398163397444);
#577=CONICAL_SURFACE('',#17528,40.,1.03037682652431);
#578=CONICAL_SURFACE('',#17530,47.5,0.484477929037023);
#579=CONICAL_SURFACE('',#17534,69.5,0.785398163397448);
#580=CONICAL_SURFACE('',#17537,12.9267766952966,1.17809724509617);
#581=CONICAL_SURFACE('',#17540,13.5,0.785398163397451);
#582=CONICAL_SURFACE('',#17544,13.8232233047034,0.392699081698724);
#583=CONICAL_SURFACE('',#17547,69.7,0.785398163397444);
#584=CONICAL_SURFACE('',#17579,69.5,0.785398163397448);
#585=CONICAL_SURFACE('',#17583,47.5,0.484477929037023);
#586=CONICAL_SURFACE('',#17585,40.,1.03037682652431);
#587=CONICAL_SURFACE('',#17639,45.,1.44644133224813);
#588=CONICAL_SURFACE('',#17647,45.,1.44644133224814);
#589=CONICAL_SURFACE('',#17651,28.9663172798365,1.17809724509618);
#590=CONICAL_SURFACE('',#17657,29.5,0.785398163397448);
#591=CONICAL_SURFACE('',#17665,17.9940985792758,1.40992104959658);
#592=CONICAL_SURFACE('',#17671,24.,1.24904577239825);
#593=CONICAL_SURFACE('',#17673,5.215,0.785398163397446);
#594=CONICAL_SURFACE('',#17682,5.215,0.785398163397455);
#595=CONICAL_SURFACE('',#17763,4.75,0.78539816339745);
#596=CONICAL_SURFACE('',#17771,4.75,0.78539816339745);
#597=CONICAL_SURFACE('',#17775,7.580184099288,1.30874388895068);
#598=CONICAL_SURFACE('',#17783,8.83380215351701,1.04669145110647);
#599=CONICAL_SURFACE('',#17784,8.83380215351701,1.04669145110647);
#600=CONICAL_SURFACE('',#17785,8.83380215351701,1.04669145110647);
#601=CONICAL_SURFACE('',#17786,8.83380215351701,1.04669145110647);
#602=CONICAL_SURFACE('',#17787,8.83380215351701,1.04669145110647);
#603=CONICAL_SURFACE('',#17788,8.83380215351701,1.04669145110647);
#604=CONICAL_SURFACE('',#17806,8.83380215351701,1.04669145110647);
#605=CONICAL_SURFACE('',#17808,5.25,0.674740942223553);
#606=CONICAL_SURFACE('',#17813,5.25,0.674740942223554);
#607=CONICAL_SURFACE('',#17819,10.25,0.785398163397459);
#608=CONICAL_SURFACE('',#17831,10.8,0.785398163397442);
#609=CONICAL_SURFACE('',#18026,15.75,0.785398163397442);
#610=CONICAL_SURFACE('',#18035,15.8232233047034,0.392699081698714);
#611=CONICAL_SURFACE('',#18038,15.5,0.785398163397451);
#612=CONICAL_SURFACE('',#18041,14.9267766952966,1.17809724509618);
#613=CONICAL_SURFACE('',#18063,11.75,0.785398163397442);
#614=CONICAL_SURFACE('',#18116,8.5,0.78539816339745);
#615=CONICAL_SURFACE('',#18134,6.65,0.540419500270586);
#616=CONICAL_SURFACE('',#18161,11.8232233047034,0.392699081698714);
#617=CONICAL_SURFACE('',#18166,11.25,0.785398163397447);
#618=CONICAL_SURFACE('',#18171,10.4267766952966,1.17809724509618);
#619=CONICAL_SURFACE('',#18174,11.75,0.785398163397451);
#620=CONICAL_SURFACE('',#18199,8.35,0.540419500270581);
#621=CONICAL_SURFACE('',#18211,12.75,0.785398163397449);
#622=CONICAL_SURFACE('',#18215,12.75,0.78539816339745);
#623=CONICAL_SURFACE('',#18219,3.75,0.785398163397446);
#624=CONICAL_SURFACE('',#18230,3.75,0.785398163397446);
#625=CONICAL_SURFACE('',#18235,0.550000000000001,0.785398163397449);
#626=CONICAL_SURFACE('',#18239,0.550000000000001,0.785398163397449);
#627=CONICAL_SURFACE('',#18243,0.550000000000001,0.785398163397449);
#628=CONICAL_SURFACE('',#18247,1.05,0.785398163397449);
#629=CONICAL_SURFACE('',#18251,1.05,0.785398163397449);
#630=CONICAL_SURFACE('',#18255,0.550000000000001,0.785398163397449);
#631=CONICAL_SURFACE('',#18259,0.550000000000001,0.785398163397449);
#632=CONICAL_SURFACE('',#18263,0.550000000000001,0.785398163397449);
#633=CONICAL_SURFACE('',#18286,0.550000000000001,0.78539816339744);
#634=CONICAL_SURFACE('',#18290,0.550000000000001,0.78539816339744);
#635=CONICAL_SURFACE('',#18294,0.550000000000001,0.78539816339744);
#636=CONICAL_SURFACE('',#18298,1.05,0.78539816339744);
#637=CONICAL_SURFACE('',#18302,1.05,0.78539816339744);
#638=CONICAL_SURFACE('',#18305,0.550000000000001,0.78539816339744);
#639=CONICAL_SURFACE('',#18308,0.550000000000001,0.78539816339744);
#640=CONICAL_SURFACE('',#18311,0.550000000000001,0.78539816339744);
#641=CONICAL_SURFACE('',#18321,3.75,0.785398163397448);
#642=CONICAL_SURFACE('',#18322,3.75,0.785398163397448);
#643=CONICAL_SURFACE('',#18350,9.82322330470336,0.392699081698723);
#644=CONICAL_SURFACE('',#18355,9.5,0.785398163397448);
#645=CONICAL_SURFACE('',#18360,8.92677669529664,1.17809724509617);
#646=CONICAL_SURFACE('',#18369,9.,0.785398163397448);
#647=CONICAL_SURFACE('',#18372,3.75,0.785398163397451);
#648=CONICAL_SURFACE('',#18472,7.25527674973257,1.046630884618);
#649=CONICAL_SURFACE('',#18485,3.75,0.785398163397451);
#650=CONICAL_SURFACE('',#18672,7.25527674973257,1.046630884618);
#651=CONICAL_SURFACE('',#18685,3.75,0.785398163397442);
#652=CONICAL_SURFACE('',#18688,6.15985379710312,1.30871360570645);
#653=CONICAL_SURFACE('',#18696,7.25527674973257,1.046630884618);
#654=CONICAL_SURFACE('',#18697,7.25527674973257,1.046630884618);
#655=CONICAL_SURFACE('',#18698,7.25527674973257,1.046630884618);
#656=CONICAL_SURFACE('',#18699,7.25527674973257,1.046630884618);
#657=CONICAL_SURFACE('',#18700,7.25527674973257,1.046630884618);
#658=CONICAL_SURFACE('',#18701,7.25527674973257,1.046630884618);
#659=CONICAL_SURFACE('',#18719,7.25527674973257,1.046630884618);
#660=CONICAL_SURFACE('',#18721,4.25,0.674740942223553);
#661=CONICAL_SURFACE('',#18726,4.25,0.674740942223553);
#662=CIRCLE('',#17196,4.05);
#663=CIRCLE('',#17197,4.05);
#664=CIRCLE('',#17198,4.05);
#665=CIRCLE('',#17199,4.05);
#666=CIRCLE('',#17204,4.05);
#667=CIRCLE('',#17205,4.05);
#668=CIRCLE('',#17206,4.05);
#669=CIRCLE('',#17207,4.05);
#670=CIRCLE('',#17209,4.55);
#671=CIRCLE('',#17211,6.00000000000001);
#672=CIRCLE('',#17212,6.);
#673=CIRCLE('',#17213,6.);
#674=CIRCLE('',#17214,6.);
#675=CIRCLE('',#17215,4.55);
#676=CIRCLE('',#17216,13.05);
#677=CIRCLE('',#17219,4.55);
#678=CIRCLE('',#17220,4.05);
#679=CIRCLE('',#17222,6.00000000000001);
#680=CIRCLE('',#17223,6.);
#681=CIRCLE('',#17224,6.);
#682=CIRCLE('',#17225,6.);
#683=CIRCLE('',#17226,4.55);
#684=CIRCLE('',#17227,13.05);
#685=CIRCLE('',#17229,4.05);
#686=CIRCLE('',#17231,4.05);
#687=CIRCLE('',#17233,4.05);
#688=CIRCLE('',#17235,47.1674514378614);
#689=CIRCLE('',#17236,46.5214276345237);
#690=CIRCLE('',#17238,53.);
#691=CIRCLE('',#17240,47.1674514378614);
#692=CIRCLE('',#17241,46.5214276345237);
#693=CIRCLE('',#17242,46.5214276345237);
#694=CIRCLE('',#17244,53.);
#695=CIRCLE('',#17246,34.2759001296373);
#696=CIRCLE('',#17247,2.);
#697=CIRCLE('',#17248,35.5562689289663);
#698=CIRCLE('',#17249,35.5562689289663);
#699=CIRCLE('',#17251,38.6);
#700=CIRCLE('',#17252,38.6);
#701=CIRCLE('',#17255,72.4142135623731);
#702=CIRCLE('',#17256,71.1954923578975);
#703=CIRCLE('',#17258,4.5);
#704=CIRCLE('',#17259,4.5);
#705=CIRCLE('',#17260,4.5);
#706=CIRCLE('',#17262,73.);
#707=CIRCLE('',#17263,73.);
#708=CIRCLE('',#17265,73.);
#709=CIRCLE('',#17266,73.);
#710=CIRCLE('',#17267,73.);
#711=CIRCLE('',#17268,73.);
#712=CIRCLE('',#17270,72.4142135623731);
#713=CIRCLE('',#17271,71.1954923578975);
#714=CIRCLE('',#17273,4.5);
#715=CIRCLE('',#17274,4.5);
#716=CIRCLE('',#17275,4.5);
#717=CIRCLE('',#17278,2.);
#718=CIRCLE('',#17279,71.);
#719=CIRCLE('',#17281,4.5);
#720=CIRCLE('',#17282,4.5);
#721=CIRCLE('',#17283,4.5);
#722=CIRCLE('',#17284,4.5);
#723=CIRCLE('',#17285,4.5);
#724=CIRCLE('',#17286,4.5);
#725=CIRCLE('',#17287,51.1654934782503);
#726=CIRCLE('',#17289,6.);
#727=CIRCLE('',#17290,2.);
#728=CIRCLE('',#17291,8.);
#729=CIRCLE('',#17293,2.);
#730=CIRCLE('',#17295,2.);
#731=CIRCLE('',#17296,8.);
#732=CIRCLE('',#17297,6.);
#733=CIRCLE('',#17301,8.);
#734=CIRCLE('',#17302,8.00000000000001);
#735=CIRCLE('',#17304,2.);
#736=CIRCLE('',#17305,2.);
#737=CIRCLE('',#17307,2.);
#738=CIRCLE('',#17308,8.00000000000001);
#739=CIRCLE('',#17310,2.);
#740=CIRCLE('',#17312,2.);
#741=CIRCLE('',#17313,8.);
#742=CIRCLE('',#17315,2.);
#743=CIRCLE('',#17317,2.);
#744=CIRCLE('',#17318,8.);
#745=CIRCLE('',#17320,2.);
#746=CIRCLE('',#17322,8.);
#747=CIRCLE('',#17324,8.);
#748=CIRCLE('',#17327,8.00000000000001);
#749=CIRCLE('',#17329,2.);
#750=CIRCLE('',#17331,2.00000000000001);
#751=CIRCLE('',#17332,2.);
#752=CIRCLE('',#17334,6.);
#753=CIRCLE('',#17336,6.00000000000001);
#754=CIRCLE('',#17338,8.00000000000002);
#755=CIRCLE('',#17339,8.00000000000001);
#756=CIRCLE('',#17341,2.);
#757=CIRCLE('',#17342,49.3890581919384);
#758=CIRCLE('',#17343,49.3890581919384);
#759=CIRCLE('',#17345,44.);
#760=CIRCLE('',#17349,32.);
#761=CIRCLE('',#17350,32.);
#762=CIRCLE('',#17352,7.);
#763=CIRCLE('',#17353,7.);
#764=CIRCLE('',#17355,8.);
#765=CIRCLE('',#17356,2.);
#766=CIRCLE('',#17357,6.);
#767=CIRCLE('',#17359,2.);
#768=CIRCLE('',#17361,1.99999999999999);
#769=CIRCLE('',#17362,6.);
#770=CIRCLE('',#17363,8.);
#771=CIRCLE('',#17367,8.);
#772=CIRCLE('',#17369,6.05);
#773=CIRCLE('',#17370,8.);
#774=CIRCLE('',#17372,6.05);
#775=CIRCLE('',#17374,2.);
#776=CIRCLE('',#17375,2.);
#777=CIRCLE('',#17376,8.00000000000001);
#778=CIRCLE('',#17378,2.);
#779=CIRCLE('',#17380,2.);
#780=CIRCLE('',#17381,8.);
#781=CIRCLE('',#17383,2.);
#782=CIRCLE('',#17385,2.);
#783=CIRCLE('',#17387,2.);
#784=CIRCLE('',#17389,2.);
#785=CIRCLE('',#17390,8.);
#786=CIRCLE('',#17395,8.00000000000001);
#787=CIRCLE('',#17397,2.);
#788=CIRCLE('',#17399,2.);
#789=CIRCLE('',#17400,6.00000000000001);
#790=CIRCLE('',#17402,2.);
#791=CIRCLE('',#17404,6.);
#792=CIRCLE('',#17405,8.);
#793=CIRCLE('',#17407,8.00000000000001);
#794=CIRCLE('',#17408,6.05);
#795=CIRCLE('',#17410,6.05);
#796=CIRCLE('',#17411,8.00000000000002);
#797=CIRCLE('',#17414,2.);
#798=CIRCLE('',#17416,2.);
#799=CIRCLE('',#17418,2.);
#800=CIRCLE('',#17420,2.);
#801=CIRCLE('',#17422,2.);
#802=CIRCLE('',#17424,2.);
#803=CIRCLE('',#17426,2.);
#804=CIRCLE('',#17428,2.);
#805=CIRCLE('',#17430,2.);
#806=CIRCLE('',#17432,2.);
#807=CIRCLE('',#17434,2.);
#808=CIRCLE('',#17436,2.);
#809=CIRCLE('',#17448,8.00000000000001);
#810=CIRCLE('',#17456,13.05);
#811=CIRCLE('',#17458,11.);
#812=CIRCLE('',#17460,11.);
#813=CIRCLE('',#17463,13.05);
#814=CIRCLE('',#17466,32.);
#815=CIRCLE('',#17487,11.3535533905933);
#816=CIRCLE('',#17488,10.5);
#817=CIRCLE('',#17490,11.6464466094067);
#818=CIRCLE('',#17492,6.9);
#819=CIRCLE('',#17494,12.);
#820=CIRCLE('',#17497,69.4);
#821=CIRCLE('',#17498,70.);
#822=CIRCLE('',#17499,70.);
#823=CIRCLE('',#17501,70.);
#824=CIRCLE('',#17503,4.5);
#825=CIRCLE('',#17504,4.5);
#826=CIRCLE('',#17505,4.5);
#827=CIRCLE('',#17506,4.5);
#828=CIRCLE('',#17507,4.5);
#829=CIRCLE('',#17508,4.5);
#830=CIRCLE('',#17509,8.05);
#831=CIRCLE('',#17511,6.9);
#832=CIRCLE('',#17514,4.5);
#833=CIRCLE('',#17516,4.5);
#834=CIRCLE('',#17518,4.5);
#835=CIRCLE('',#17520,4.5);
#836=CIRCLE('',#17522,4.5);
#837=CIRCLE('',#17524,4.5);
#838=CIRCLE('',#17526,35.);
#839=CIRCLE('',#17527,8.05);
#840=CIRCLE('',#17529,45.);
#841=CIRCLE('',#17531,50.);
#842=CIRCLE('',#17533,69.);
#843=CIRCLE('',#17538,13.3535533905933);
#844=CIRCLE('',#17539,12.5);
#845=CIRCLE('',#17541,13.6464466094067);
#846=CIRCLE('',#17543,8.6);
#847=CIRCLE('',#17545,14.);
#848=CIRCLE('',#17546,14.);
#849=CIRCLE('',#17548,70.);
#850=CIRCLE('',#17549,70.);
#851=CIRCLE('',#17550,69.4);
#852=CIRCLE('',#17552,4.5);
#853=CIRCLE('',#17553,4.5);
#854=CIRCLE('',#17554,4.5);
#855=CIRCLE('',#17555,4.5);
#856=CIRCLE('',#17556,4.5);
#857=CIRCLE('',#17557,4.5);
#858=CIRCLE('',#17558,8.05);
#859=CIRCLE('',#17560,70.);
#860=CIRCLE('',#17563,8.6);
#861=CIRCLE('',#17566,4.5);
#862=CIRCLE('',#17568,4.5);
#863=CIRCLE('',#17570,4.5);
#864=CIRCLE('',#17572,4.5);
#865=CIRCLE('',#17574,4.5);
#866=CIRCLE('',#17576,4.5);
#867=CIRCLE('',#17578,8.05);
#868=CIRCLE('',#17580,69.);
#869=CIRCLE('',#17582,50.);
#870=CIRCLE('',#17584,45.);
#871=CIRCLE('',#17586,35.);
#872=CIRCLE('',#17590,4.5);
#873=CIRCLE('',#17591,4.5);
#874=CIRCLE('',#17593,4.5);
#875=CIRCLE('',#17594,4.5);
#876=CIRCLE('',#17596,4.5);
#877=CIRCLE('',#17597,4.5);
#878=CIRCLE('',#17599,4.5);
#879=CIRCLE('',#17600,4.5);
#880=CIRCLE('',#17602,4.5);
#881=CIRCLE('',#17603,4.5);
#882=CIRCLE('',#17605,4.5);
#883=CIRCLE('',#17606,4.5);
#884=CIRCLE('',#17608,8.5);
#885=CIRCLE('',#17609,8.5);
#886=CIRCLE('',#17611,70.);
#887=CIRCLE('',#17613,70.);
#888=CIRCLE('',#17617,4.5);
#889=CIRCLE('',#17618,4.5);
#890=CIRCLE('',#17620,4.5);
#891=CIRCLE('',#17621,4.5);
#892=CIRCLE('',#17623,4.5);
#893=CIRCLE('',#17624,4.5);
#894=CIRCLE('',#17626,4.5);
#895=CIRCLE('',#17627,4.5);
#896=CIRCLE('',#17629,4.5);
#897=CIRCLE('',#17630,4.5);
#898=CIRCLE('',#17632,4.5);
#899=CIRCLE('',#17633,4.5);
#900=CIRCLE('',#17635,5.2);
#901=CIRCLE('',#17636,5.2);
#902=CIRCLE('',#17638,44.);
#903=CIRCLE('',#17640,46.);
#904=CIRCLE('',#17642,70.);
#905=CIRCLE('',#17644,70.);
#906=CIRCLE('',#17646,46.);
#907=CIRCLE('',#17648,44.);
#908=CIRCLE('',#17652,29.1626345596729);
#909=CIRCLE('',#17653,29.1626345596729);
#910=CIRCLE('',#17654,28.77);
#911=CIRCLE('',#17656,5.1);
#912=CIRCLE('',#17658,30.);
#913=CIRCLE('',#17660,5.1);
#914=CIRCLE('',#17662,30.);
#915=CIRCLE('',#17666,17.77);
#916=CIRCLE('',#17667,18.2181971585516);
#917=CIRCLE('',#17668,18.2181971585516);
#918=CIRCLE('',#17670,5.33);
#919=CIRCLE('',#17672,30.);
#920=CIRCLE('',#17674,5.33);
#921=CIRCLE('',#17675,5.1);
#922=CIRCLE('',#17676,5.1);
#923=CIRCLE('',#17678,5.1);
#924=CIRCLE('',#17679,5.1);
#925=CIRCLE('',#17681,30.);
#926=CIRCLE('',#17686,4.925);
#927=CIRCLE('',#17702,4.0705);
#928=CIRCLE('',#17718,4.925);
#929=CIRCLE('',#17734,4.0705);
#930=CIRCLE('',#17750,4.925);
#931=CIRCLE('',#17751,4.925);
#932=CIRCLE('',#17753,4.0705);
#933=CIRCLE('',#17755,4.925);
#934=CIRCLE('',#17757,4.925);
#935=CIRCLE('',#17758,4.925);
#936=CIRCLE('',#17759,4.0705);
#937=CIRCLE('',#17762,4.5);
#938=CIRCLE('',#17765,4.925);
#939=CIRCLE('',#17767,8.);
#940=CIRCLE('',#17769,8.);
#941=CIRCLE('',#17772,4.5);
#942=CIRCLE('',#17776,7.26300281800529);
#943=CIRCLE('',#17777,7.89736538057071);
#944=CIRCLE('',#17778,7.89736538057071);
#945=CIRCLE('',#17779,7.89736538057071);
#946=CIRCLE('',#17780,7.89736538057071);
#947=CIRCLE('',#17781,7.89736538057071);
#948=CIRCLE('',#17782,7.89736538057071);
#949=CIRCLE('',#17790,5.37);
#950=CIRCLE('',#17807,7.60300281800529);
#951=CIRCLE('',#17809,5.37);
#952=CIRCLE('',#17810,5.05);
#953=CIRCLE('',#17812,5.05);
#954=CIRCLE('',#17820,10.5);
#955=CIRCLE('',#17821,10.);
#956=CIRCLE('',#17822,10.);
#957=CIRCLE('',#17824,12.05);
#958=CIRCLE('',#17826,10.);
#959=CIRCLE('',#17832,11.05);
#960=CIRCLE('',#17833,10.55);
#961=CIRCLE('',#17835,15.5);
#962=CIRCLE('',#17837,10.55);
#963=CIRCLE('',#17839,17.);
#964=CIRCLE('',#17840,1.5);
#965=CIRCLE('',#17842,17.);
#966=CIRCLE('',#17843,17.);
#967=CIRCLE('',#17845,1.5);
#968=CIRCLE('',#17846,15.5);
#969=CIRCLE('',#17848,14.);
#970=CIRCLE('',#17850,15.5);
#971=CIRCLE('',#17851,1.5);
#972=CIRCLE('',#17852,17.);
#973=CIRCLE('',#17853,17.);
#974=CIRCLE('',#17855,17.);
#975=CIRCLE('',#17857,14.);
#976=CIRCLE('',#17859,1.5);
#977=CIRCLE('',#17860,15.5);
#978=CIRCLE('',#17862,12.05);
#979=CIRCLE('',#17864,1.5);
#980=CIRCLE('',#17865,1.5);
#981=CIRCLE('',#17867,1.5);
#982=CIRCLE('',#17868,4.5);
#983=CIRCLE('',#17869,6.);
#984=CIRCLE('',#17871,1.5);
#985=CIRCLE('',#17873,1.49999999999999);
#986=CIRCLE('',#17874,4.50000000000001);
#987=CIRCLE('',#17875,6.00000000000001);
#988=CIRCLE('',#17877,1.5);
#989=CIRCLE('',#17879,1.5);
#990=CIRCLE('',#17880,4.50000000000001);
#991=CIRCLE('',#17881,6.00000000000001);
#992=CIRCLE('',#17883,1.5);
#993=CIRCLE('',#17885,4.5);
#994=CIRCLE('',#17886,6.);
#995=CIRCLE('',#17888,6.00000000000001);
#996=CIRCLE('',#17891,6.);
#997=CIRCLE('',#17893,14.);
#998=CIRCLE('',#17895,10.);
#999=CIRCLE('',#17896,4.5);
#1000=CIRCLE('',#17897,4.5);
#1001=CIRCLE('',#17899,1.5);
#1002=CIRCLE('',#17900,1.5);
#1003=CIRCLE('',#17902,1.5);
#1004=CIRCLE('',#17903,4.5);
#1005=CIRCLE('',#17905,1.5);
#1006=CIRCLE('',#17907,1.5);
#1007=CIRCLE('',#17908,4.50000000000001);
#1008=CIRCLE('',#17910,1.5);
#1009=CIRCLE('',#17912,1.5);
#1010=CIRCLE('',#17913,6.00000000000001);
#1011=CIRCLE('',#17914,4.50000000000001);
#1012=CIRCLE('',#17916,1.5);
#1013=CIRCLE('',#17918,6.);
#1014=CIRCLE('',#17919,4.5);
#1015=CIRCLE('',#17924,4.5);
#1016=CIRCLE('',#17925,4.5);
#1017=CIRCLE('',#17927,1.5);
#1018=CIRCLE('',#17928,1.5);
#1019=CIRCLE('',#17930,1.5);
#1020=CIRCLE('',#17931,4.50000000000001);
#1021=CIRCLE('',#17932,6.00000000000001);
#1022=CIRCLE('',#17934,1.5);
#1023=CIRCLE('',#17936,1.49999999999999);
#1024=CIRCLE('',#17937,4.5);
#1025=CIRCLE('',#17938,6.);
#1026=CIRCLE('',#17940,1.5);
#1027=CIRCLE('',#17942,1.5);
#1028=CIRCLE('',#17943,4.5);
#1029=CIRCLE('',#17944,6.);
#1030=CIRCLE('',#17946,1.5);
#1031=CIRCLE('',#17948,4.50000000000001);
#1032=CIRCLE('',#17949,6.00000000000001);
#1033=CIRCLE('',#17951,6.);
#1034=CIRCLE('',#17954,6.00000000000001);
#1035=CIRCLE('',#17956,14.);
#1036=CIRCLE('',#17958,10.);
#1037=CIRCLE('',#17959,4.5);
#1038=CIRCLE('',#17960,4.5);
#1039=CIRCLE('',#17962,1.50000000000001);
#1040=CIRCLE('',#17963,1.5);
#1041=CIRCLE('',#17965,1.5);
#1042=CIRCLE('',#17966,4.50000000000001);
#1043=CIRCLE('',#17968,1.5);
#1044=CIRCLE('',#17970,1.5);
#1045=CIRCLE('',#17971,4.5);
#1046=CIRCLE('',#17973,1.5);
#1047=CIRCLE('',#17975,1.5);
#1048=CIRCLE('',#17976,6.);
#1049=CIRCLE('',#17977,4.5);
#1050=CIRCLE('',#17979,1.5);
#1051=CIRCLE('',#17981,6.00000000000001);
#1052=CIRCLE('',#17982,4.50000000000001);
#1053=CIRCLE('',#17987,4.5);
#1054=CIRCLE('',#17988,4.5);
#1055=CIRCLE('',#18004,14.);
#1056=CIRCLE('',#18007,14.);
#1057=CIRCLE('',#18012,11.925);
#1058=CIRCLE('',#18019,11.06595);
#1059=CIRCLE('',#18021,11.06595);
#1060=CIRCLE('',#18027,15.5);
#1061=CIRCLE('',#18028,16.);
#1062=CIRCLE('',#18029,16.);
#1063=CIRCLE('',#18031,16.);
#1064=CIRCLE('',#18032,16.);
#1065=CIRCLE('',#18034,11.06595);
#1066=CIRCLE('',#18036,15.6464466094067);
#1067=CIRCLE('',#18037,15.6464466094067);
#1068=CIRCLE('',#18039,15.3535533905933);
#1069=CIRCLE('',#18040,15.3535533905933);
#1070=CIRCLE('',#18042,14.5);
#1071=CIRCLE('',#18054,11.925);
#1072=CIRCLE('',#18055,11.925);
#1073=CIRCLE('',#18058,11.925);
#1074=CIRCLE('',#18064,11.5);
#1075=CIRCLE('',#18068,2.99999999999999);
#1076=CIRCLE('',#18069,2.99999999999997);
#1077=CIRCLE('',#18070,2.99999999999999);
#1078=CIRCLE('',#18071,3.00000000000001);
#1079=CIRCLE('',#18072,3.);
#1080=CIRCLE('',#18075,2.99999999999997);
#1081=CIRCLE('',#18078,2.99999999999999);
#1082=CIRCLE('',#18081,3.00000000000001);
#1083=CIRCLE('',#18084,2.99999999999999);
#1084=CIRCLE('',#18092,5.6);
#1085=CIRCLE('',#18094,5.6);
#1086=CIRCLE('',#18096,9.);
#1087=CIRCLE('',#18098,9.);
#1088=CIRCLE('',#18100,9.);
#1089=CIRCLE('',#18102,9.);
#1090=CIRCLE('',#18103,9.);
#1091=CIRCLE('',#18105,9.);
#1092=CIRCLE('',#18107,9.);
#1093=CIRCLE('',#18109,9.);
#1094=CIRCLE('',#18110,9.);
#1095=CIRCLE('',#18111,9.);
#1096=CIRCLE('',#18112,9.);
#1097=CIRCLE('',#18113,9.);
#1098=CIRCLE('',#18114,9.);
#1099=CIRCLE('',#18115,9.);
#1100=CIRCLE('',#18117,8.);
#1101=CIRCLE('',#18125,6.8);
#1102=CIRCLE('',#18133,6.5);
#1103=CIRCLE('',#18135,6.8);
#1104=CIRCLE('',#18160,8.5);
#1105=CIRCLE('',#18162,12.);
#1106=CIRCLE('',#18163,12.);
#1107=CIRCLE('',#18164,11.6464466094067);
#1108=CIRCLE('',#18165,11.6464466094067);
#1109=CIRCLE('',#18167,10.8535533905933);
#1110=CIRCLE('',#18168,10.8535533905933);
#1111=CIRCLE('',#18170,12.);
#1112=CIRCLE('',#18172,10.);
#1113=CIRCLE('',#18175,11.5);
#1114=CIRCLE('',#18176,12.);
#1115=CIRCLE('',#18177,12.);
#1116=CIRCLE('',#18179,12.);
#1117=CIRCLE('',#18182,11.);
#1118=CIRCLE('',#18184,12.);
#1119=CIRCLE('',#18185,11.);
#1120=CIRCLE('',#18188,12.);
#1121=CIRCLE('',#18190,11.);
#1122=CIRCLE('',#18192,11.);
#1123=CIRCLE('',#18198,8.5);
#1124=CIRCLE('',#18200,8.2);
#1125=CIRCLE('',#18204,8.);
#1126=CIRCLE('',#18207,6.);
#1127=CIRCLE('',#18208,6.);
#1128=CIRCLE('',#18210,12.5);
#1129=CIRCLE('',#18212,13.);
#1130=CIRCLE('',#18214,13.);
#1131=CIRCLE('',#18216,12.5);
#1132=CIRCLE('',#18220,3.99999999999999);
#1133=CIRCLE('',#18221,3.5);
#1134=CIRCLE('',#18223,3.99999999999999);
#1135=CIRCLE('',#18224,4.5);
#1136=CIRCLE('',#18225,4.5);
#1137=CIRCLE('',#18226,4.5);
#1138=CIRCLE('',#18227,4.5);
#1139=CIRCLE('',#18229,3.5);
#1140=CIRCLE('',#18231,3.5);
#1141=CIRCLE('',#18233,3.5);
#1142=CIRCLE('',#18236,0.8);
#1143=CIRCLE('',#18237,0.300000000000001);
#1144=CIRCLE('',#18240,0.8);
#1145=CIRCLE('',#18241,0.300000000000001);
#1146=CIRCLE('',#18244,0.8);
#1147=CIRCLE('',#18245,0.300000000000001);
#1148=CIRCLE('',#18248,0.8);
#1149=CIRCLE('',#18249,1.3);
#1150=CIRCLE('',#18252,0.8);
#1151=CIRCLE('',#18253,1.3);
#1152=CIRCLE('',#18256,0.8);
#1153=CIRCLE('',#18257,0.300000000000001);
#1154=CIRCLE('',#18260,0.8);
#1155=CIRCLE('',#18261,0.300000000000001);
#1156=CIRCLE('',#18264,0.8);
#1157=CIRCLE('',#18265,0.300000000000001);
#1158=CIRCLE('',#18267,0.8);
#1159=CIRCLE('',#18270,0.8);
#1160=CIRCLE('',#18273,0.8);
#1161=CIRCLE('',#18276,0.8);
#1162=CIRCLE('',#18278,3.99999999999999);
#1163=CIRCLE('',#18279,4.5);
#1164=CIRCLE('',#18280,4.5);
#1165=CIRCLE('',#18281,4.5);
#1166=CIRCLE('',#18282,4.5);
#1167=CIRCLE('',#18283,3.99999999999999);
#1168=CIRCLE('',#18287,0.8);
#1169=CIRCLE('',#18288,0.300000000000001);
#1170=CIRCLE('',#18291,0.8);
#1171=CIRCLE('',#18292,0.300000000000001);
#1172=CIRCLE('',#18295,0.8);
#1173=CIRCLE('',#18296,0.300000000000001);
#1174=CIRCLE('',#18299,0.8);
#1175=CIRCLE('',#18300,1.3);
#1176=CIRCLE('',#18303,1.3);
#1177=CIRCLE('',#18306,0.300000000000001);
#1178=CIRCLE('',#18309,0.300000000000001);
#1179=CIRCLE('',#18312,0.300000000000001);
#1180=CIRCLE('',#18329,3.933);
#1181=CIRCLE('',#18339,3.933);
#1182=CIRCLE('',#18341,3.22275);
#1183=CIRCLE('',#18351,10.);
#1184=CIRCLE('',#18352,10.);
#1185=CIRCLE('',#18353,9.64644660940673);
#1186=CIRCLE('',#18354,9.64644660940673);
#1187=CIRCLE('',#18356,9.35355339059327);
#1188=CIRCLE('',#18357,9.35355339059327);
#1189=CIRCLE('',#18359,10.);
#1190=CIRCLE('',#18361,8.5);
#1191=CIRCLE('',#18364,3.933);
#1192=CIRCLE('',#18366,3.22275);
#1193=CIRCLE('',#18368,3.933);
#1194=CIRCLE('',#18370,8.);
#1195=CIRCLE('',#18373,3.5);
#1196=CIRCLE('',#18377,3.933);
#1197=CIRCLE('',#18422,3.22275);
#1198=CIRCLE('',#18424,3.22275);
#1199=CIRCLE('',#18468,3.933);
#1200=CIRCLE('',#18469,3.933);
#1201=CIRCLE('',#18470,3.22275);
#1202=CIRCLE('',#18473,6.17797863635533);
#1203=CIRCLE('',#18478,3.933);
#1204=CIRCLE('',#18484,3.5);
#1205=CIRCLE('',#18489,3.933);
#1206=CIRCLE('',#18578,3.22275);
#1207=CIRCLE('',#18580,3.22275);
#1208=CIRCLE('',#18668,3.933);
#1209=CIRCLE('',#18669,3.933);
#1210=CIRCLE('',#18670,3.22275);
#1211=CIRCLE('',#18673,6.17797863635533);
#1212=CIRCLE('',#18678,3.933);
#1213=CIRCLE('',#18684,3.5);
#1214=CIRCLE('',#18689,5.90797863635533);
#1215=CIRCLE('',#18690,6.41172895785092);
#1216=CIRCLE('',#18691,6.41172895785092);
#1217=CIRCLE('',#18692,6.41172895785092);
#1218=CIRCLE('',#18693,6.41172895785092);
#1219=CIRCLE('',#18694,6.41172895785092);
#1220=CIRCLE('',#18695,6.41172895785092);
#1221=CIRCLE('',#18703,4.37);
#1222=CIRCLE('',#18720,6.17797863635533);
#1223=CIRCLE('',#18722,4.37);
#1224=CIRCLE('',#18723,4.05);
#1225=CIRCLE('',#18725,4.05);
#1226=CYLINDRICAL_SURFACE('',#17195,4.05);
#1227=CYLINDRICAL_SURFACE('',#17203,4.05);
#1228=CYLINDRICAL_SURFACE('',#17228,4.05);
#1229=CYLINDRICAL_SURFACE('',#17232,4.05);
#1230=CYLINDRICAL_SURFACE('',#17264,73.);
#1231=CYLINDRICAL_SURFACE('',#17292,2.);
#1232=CYLINDRICAL_SURFACE('',#17298,2.);
#1233=CYLINDRICAL_SURFACE('',#17303,2.);
#1234=CYLINDRICAL_SURFACE('',#17309,2.);
#1235=CYLINDRICAL_SURFACE('',#17314,2.);
#1236=CYLINDRICAL_SURFACE('',#17319,2.);
#1237=CYLINDRICAL_SURFACE('',#17323,8.);
#1238=CYLINDRICAL_SURFACE('',#17326,8.00000000000001);
#1239=CYLINDRICAL_SURFACE('',#17328,2.);
#1240=CYLINDRICAL_SURFACE('',#17330,2.);
#1241=CYLINDRICAL_SURFACE('',#17346,2.);
#1242=CYLINDRICAL_SURFACE('',#17347,2.);
#1243=CYLINDRICAL_SURFACE('',#17351,7.);
#1244=CYLINDRICAL_SURFACE('',#17358,2.);
#1245=CYLINDRICAL_SURFACE('',#17364,2.);
#1246=CYLINDRICAL_SURFACE('',#17366,8.);
#1247=CYLINDRICAL_SURFACE('',#17377,2.);
#1248=CYLINDRICAL_SURFACE('',#17382,2.);
#1249=CYLINDRICAL_SURFACE('',#17386,2.);
#1250=CYLINDRICAL_SURFACE('',#17391,2.);
#1251=CYLINDRICAL_SURFACE('',#17392,8.);
#1252=CYLINDRICAL_SURFACE('',#17394,8.00000000000001);
#1253=CYLINDRICAL_SURFACE('',#17396,2.);
#1254=CYLINDRICAL_SURFACE('',#17401,2.);
#1255=CYLINDRICAL_SURFACE('',#17415,2.);
#1256=CYLINDRICAL_SURFACE('',#17419,2.);
#1257=CYLINDRICAL_SURFACE('',#17423,2.);
#1258=CYLINDRICAL_SURFACE('',#17427,2.);
#1259=CYLINDRICAL_SURFACE('',#17431,2.);
#1260=CYLINDRICAL_SURFACE('',#17435,2.);
#1261=CYLINDRICAL_SURFACE('',#17449,4.5);
#1262=CYLINDRICAL_SURFACE('',#17450,4.5);
#1263=CYLINDRICAL_SURFACE('',#17451,4.5);
#1264=CYLINDRICAL_SURFACE('',#17452,4.5);
#1265=CYLINDRICAL_SURFACE('',#17453,4.5);
#1266=CYLINDRICAL_SURFACE('',#17454,4.5);
#1267=CYLINDRICAL_SURFACE('',#17455,13.05);
#1268=CYLINDRICAL_SURFACE('',#17459,11.);
#1269=CYLINDRICAL_SURFACE('',#17464,13.05);
#1270=CYLINDRICAL_SURFACE('',#17468,8.);
#1271=CYLINDRICAL_SURFACE('',#17470,8.);
#1272=CYLINDRICAL_SURFACE('',#17471,8.);
#1273=CYLINDRICAL_SURFACE('',#17473,8.00000000000001);
#1274=CYLINDRICAL_SURFACE('',#17476,8.);
#1275=CYLINDRICAL_SURFACE('',#17477,8.);
#1276=CYLINDRICAL_SURFACE('',#17478,8.00000000000002);
#1277=CYLINDRICAL_SURFACE('',#17479,8.00000000000001);
#1278=CYLINDRICAL_SURFACE('',#17481,8.00000000000001);
#1279=CYLINDRICAL_SURFACE('',#17483,8.00000000000002);
#1280=CYLINDRICAL_SURFACE('',#17484,8.00000000000001);
#1281=CYLINDRICAL_SURFACE('',#17495,12.);
#1282=CYLINDRICAL_SURFACE('',#17500,70.);
#1283=CYLINDRICAL_SURFACE('',#17510,6.9);
#1284=CYLINDRICAL_SURFACE('',#17513,4.5);
#1285=CYLINDRICAL_SURFACE('',#17515,4.5);
#1286=CYLINDRICAL_SURFACE('',#17517,4.5);
#1287=CYLINDRICAL_SURFACE('',#17519,4.5);
#1288=CYLINDRICAL_SURFACE('',#17521,4.5);
#1289=CYLINDRICAL_SURFACE('',#17523,4.5);
#1290=CYLINDRICAL_SURFACE('',#17535,8.05);
#1291=CYLINDRICAL_SURFACE('',#17559,70.);
#1292=CYLINDRICAL_SURFACE('',#17561,14.);
#1293=CYLINDRICAL_SURFACE('',#17562,8.6);
#1294=CYLINDRICAL_SURFACE('',#17565,4.5);
#1295=CYLINDRICAL_SURFACE('',#17567,4.5);
#1296=CYLINDRICAL_SURFACE('',#17569,4.5);
#1297=CYLINDRICAL_SURFACE('',#17571,4.5);
#1298=CYLINDRICAL_SURFACE('',#17573,4.5);
#1299=CYLINDRICAL_SURFACE('',#17575,4.5);
#1300=CYLINDRICAL_SURFACE('',#17577,8.05);
#1301=CYLINDRICAL_SURFACE('',#17589,4.5);
#1302=CYLINDRICAL_SURFACE('',#17592,4.5);
#1303=CYLINDRICAL_SURFACE('',#17595,4.5);
#1304=CYLINDRICAL_SURFACE('',#17598,4.5);
#1305=CYLINDRICAL_SURFACE('',#17601,4.5);
#1306=CYLINDRICAL_SURFACE('',#17604,4.5);
#1307=CYLINDRICAL_SURFACE('',#17607,8.5);
#1308=CYLINDRICAL_SURFACE('',#17612,70.);
#1309=CYLINDRICAL_SURFACE('',#17616,4.5);
#1310=CYLINDRICAL_SURFACE('',#17619,4.5);
#1311=CYLINDRICAL_SURFACE('',#17622,4.5);
#1312=CYLINDRICAL_SURFACE('',#17625,4.5);
#1313=CYLINDRICAL_SURFACE('',#17628,4.5);
#1314=CYLINDRICAL_SURFACE('',#17631,4.5);
#1315=CYLINDRICAL_SURFACE('',#17634,5.2);
#1316=CYLINDRICAL_SURFACE('',#17643,70.);
#1317=CYLINDRICAL_SURFACE('',#17659,5.1);
#1318=CYLINDRICAL_SURFACE('',#17661,30.);
#1319=CYLINDRICAL_SURFACE('',#17677,5.1);
#1320=CYLINDRICAL_SURFACE('',#17683,30.);
#1321=CYLINDRICAL_SURFACE('',#17685,4.925);
#1322=CYLINDRICAL_SURFACE('',#17687,4.925);
#1323=CYLINDRICAL_SURFACE('',#17688,4.925);
#1324=CYLINDRICAL_SURFACE('',#17689,4.925);
#1325=CYLINDRICAL_SURFACE('',#17690,4.925);
#1326=CYLINDRICAL_SURFACE('',#17691,4.925);
#1327=CYLINDRICAL_SURFACE('',#17692,4.925);
#1328=CYLINDRICAL_SURFACE('',#17693,4.925);
#1329=CYLINDRICAL_SURFACE('',#17694,4.925);
#1330=CYLINDRICAL_SURFACE('',#17695,4.925);
#1331=CYLINDRICAL_SURFACE('',#17696,4.925);
#1332=CYLINDRICAL_SURFACE('',#17697,4.925);
#1333=CYLINDRICAL_SURFACE('',#17698,4.925);
#1334=CYLINDRICAL_SURFACE('',#17699,4.925);
#1335=CYLINDRICAL_SURFACE('',#17700,4.925);
#1336=CYLINDRICAL_SURFACE('',#17701,4.0705);
#1337=CYLINDRICAL_SURFACE('',#17703,4.0705);
#1338=CYLINDRICAL_SURFACE('',#17704,4.0705);
#1339=CYLINDRICAL_SURFACE('',#17705,4.0705);
#1340=CYLINDRICAL_SURFACE('',#17706,4.0705);
#1341=CYLINDRICAL_SURFACE('',#17707,4.0705);
#1342=CYLINDRICAL_SURFACE('',#17708,4.0705);
#1343=CYLINDRICAL_SURFACE('',#17709,4.0705);
#1344=CYLINDRICAL_SURFACE('',#17710,4.0705);
#1345=CYLINDRICAL_SURFACE('',#17711,4.0705);
#1346=CYLINDRICAL_SURFACE('',#17712,4.0705);
#1347=CYLINDRICAL_SURFACE('',#17713,4.0705);
#1348=CYLINDRICAL_SURFACE('',#17714,4.0705);
#1349=CYLINDRICAL_SURFACE('',#17715,4.0705);
#1350=CYLINDRICAL_SURFACE('',#17716,4.0705);
#1351=CYLINDRICAL_SURFACE('',#17717,4.925);
#1352=CYLINDRICAL_SURFACE('',#17719,4.925);
#1353=CYLINDRICAL_SURFACE('',#17720,4.925);
#1354=CYLINDRICAL_SURFACE('',#17721,4.925);
#1355=CYLINDRICAL_SURFACE('',#17722,4.925);
#1356=CYLINDRICAL_SURFACE('',#17723,4.925);
#1357=CYLINDRICAL_SURFACE('',#17724,4.925);
#1358=CYLINDRICAL_SURFACE('',#17725,4.925);
#1359=CYLINDRICAL_SURFACE('',#17726,4.925);
#1360=CYLINDRICAL_SURFACE('',#17727,4.925);
#1361=CYLINDRICAL_SURFACE('',#17728,4.925);
#1362=CYLINDRICAL_SURFACE('',#17729,4.925);
#1363=CYLINDRICAL_SURFACE('',#17730,4.925);
#1364=CYLINDRICAL_SURFACE('',#17731,4.925);
#1365=CYLINDRICAL_SURFACE('',#17732,4.925);
#1366=CYLINDRICAL_SURFACE('',#17733,4.0705);
#1367=CYLINDRICAL_SURFACE('',#17735,4.0705);
#1368=CYLINDRICAL_SURFACE('',#17736,4.0705);
#1369=CYLINDRICAL_SURFACE('',#17737,4.0705);
#1370=CYLINDRICAL_SURFACE('',#17738,4.0705);
#1371=CYLINDRICAL_SURFACE('',#17739,4.0705);
#1372=CYLINDRICAL_SURFACE('',#17740,4.0705);
#1373=CYLINDRICAL_SURFACE('',#17741,4.0705);
#1374=CYLINDRICAL_SURFACE('',#17742,4.0705);
#1375=CYLINDRICAL_SURFACE('',#17743,4.0705);
#1376=CYLINDRICAL_SURFACE('',#17744,4.0705);
#1377=CYLINDRICAL_SURFACE('',#17745,4.0705);
#1378=CYLINDRICAL_SURFACE('',#17746,4.0705);
#1379=CYLINDRICAL_SURFACE('',#17747,4.0705);
#1380=CYLINDRICAL_SURFACE('',#17748,4.0705);
#1381=CYLINDRICAL_SURFACE('',#17752,4.0705);
#1382=CYLINDRICAL_SURFACE('',#17754,4.925);
#1383=CYLINDRICAL_SURFACE('',#17760,4.0705);
#1384=CYLINDRICAL_SURFACE('',#17764,4.925);
#1385=CYLINDRICAL_SURFACE('',#17768,8.);
#1386=CYLINDRICAL_SURFACE('',#17811,5.05);
#1387=CYLINDRICAL_SURFACE('',#17825,10.);
#1388=CYLINDRICAL_SURFACE('',#17836,10.55);
#1389=CYLINDRICAL_SURFACE('',#17841,17.);
#1390=CYLINDRICAL_SURFACE('',#17854,17.);
#1391=CYLINDRICAL_SURFACE('',#17863,1.5);
#1392=CYLINDRICAL_SURFACE('',#17870,1.5);
#1393=CYLINDRICAL_SURFACE('',#17876,1.5);
#1394=CYLINDRICAL_SURFACE('',#17882,1.5);
#1395=CYLINDRICAL_SURFACE('',#17887,6.00000000000001);
#1396=CYLINDRICAL_SURFACE('',#17890,6.);
#1397=CYLINDRICAL_SURFACE('',#17898,1.5);
#1398=CYLINDRICAL_SURFACE('',#17904,1.5);
#1399=CYLINDRICAL_SURFACE('',#17909,1.5);
#1400=CYLINDRICAL_SURFACE('',#17915,1.5);
#1401=CYLINDRICAL_SURFACE('',#17920,6.00000000000001);
#1402=CYLINDRICAL_SURFACE('',#17922,6.);
#1403=CYLINDRICAL_SURFACE('',#17926,1.5);
#1404=CYLINDRICAL_SURFACE('',#17933,1.5);
#1405=CYLINDRICAL_SURFACE('',#17939,1.5);
#1406=CYLINDRICAL_SURFACE('',#17945,1.5);
#1407=CYLINDRICAL_SURFACE('',#17950,6.);
#1408=CYLINDRICAL_SURFACE('',#17953,6.00000000000001);
#1409=CYLINDRICAL_SURFACE('',#17961,1.5);
#1410=CYLINDRICAL_SURFACE('',#17967,1.5);
#1411=CYLINDRICAL_SURFACE('',#17972,1.5);
#1412=CYLINDRICAL_SURFACE('',#17978,1.5);
#1413=CYLINDRICAL_SURFACE('',#17983,6.);
#1414=CYLINDRICAL_SURFACE('',#17985,6.00000000000001);
#1415=CYLINDRICAL_SURFACE('',#17995,4.5);
#1416=CYLINDRICAL_SURFACE('',#17996,4.5);
#1417=CYLINDRICAL_SURFACE('',#17997,4.5);
#1418=CYLINDRICAL_SURFACE('',#17998,4.5);
#1419=CYLINDRICAL_SURFACE('',#17999,10.);
#1420=CYLINDRICAL_SURFACE('',#18000,10.);
#1421=CYLINDRICAL_SURFACE('',#18001,12.05);
#1422=CYLINDRICAL_SURFACE('',#18005,14.);
#1423=CYLINDRICAL_SURFACE('',#18008,14.);
#1424=CYLINDRICAL_SURFACE('',#18009,14.);
#1425=CYLINDRICAL_SURFACE('',#18011,11.925);
#1426=CYLINDRICAL_SURFACE('',#18013,11.925);
#1427=CYLINDRICAL_SURFACE('',#18014,11.925);
#1428=CYLINDRICAL_SURFACE('',#18015,11.925);
#1429=CYLINDRICAL_SURFACE('',#18016,11.925);
#1430=CYLINDRICAL_SURFACE('',#18017,11.925);
#1431=CYLINDRICAL_SURFACE('',#18018,11.06595);
#1432=CYLINDRICAL_SURFACE('',#18020,11.06595);
#1433=CYLINDRICAL_SURFACE('',#18022,11.06595);
#1434=CYLINDRICAL_SURFACE('',#18023,11.06595);
#1435=CYLINDRICAL_SURFACE('',#18024,11.06595);
#1436=CYLINDRICAL_SURFACE('',#18025,11.06595);
#1437=CYLINDRICAL_SURFACE('',#18030,16.);
#1438=CYLINDRICAL_SURFACE('',#18056,11.06595);
#1439=CYLINDRICAL_SURFACE('',#18057,11.925);
#1440=CYLINDRICAL_SURFACE('',#18074,2.99999999999997);
#1441=CYLINDRICAL_SURFACE('',#18077,2.99999999999999);
#1442=CYLINDRICAL_SURFACE('',#18080,3.00000000000001);
#1443=CYLINDRICAL_SURFACE('',#18083,2.99999999999999);
#1444=CYLINDRICAL_SURFACE('',#18086,3.);
#1445=CYLINDRICAL_SURFACE('',#18093,5.6);
#1446=CYLINDRICAL_SURFACE('',#18108,9.);
#1447=CYLINDRICAL_SURFACE('',#18136,6.8);
#1448=CYLINDRICAL_SURFACE('',#18169,12.);
#1449=CYLINDRICAL_SURFACE('',#18178,12.);
#1450=CYLINDRICAL_SURFACE('',#18186,11.);
#1451=CYLINDRICAL_SURFACE('',#18187,12.);
#1452=CYLINDRICAL_SURFACE('',#18193,11.);
#1453=CYLINDRICAL_SURFACE('',#18197,8.5);
#1454=CYLINDRICAL_SURFACE('',#18206,6.);
#1455=CYLINDRICAL_SURFACE('',#18213,13.);
#1456=CYLINDRICAL_SURFACE('',#18228,3.5);
#1457=CYLINDRICAL_SURFACE('',#18232,3.5);
#1458=CYLINDRICAL_SURFACE('',#18266,0.8);
#1459=CYLINDRICAL_SURFACE('',#18269,0.8);
#1460=CYLINDRICAL_SURFACE('',#18272,0.8);
#1461=CYLINDRICAL_SURFACE('',#18275,0.8);
#1462=CYLINDRICAL_SURFACE('',#18313,0.8);
#1463=CYLINDRICAL_SURFACE('',#18315,0.8);
#1464=CYLINDRICAL_SURFACE('',#18317,0.8);
#1465=CYLINDRICAL_SURFACE('',#18319,0.8);
#1466=CYLINDRICAL_SURFACE('',#18323,4.5);
#1467=CYLINDRICAL_SURFACE('',#18324,4.5);
#1468=CYLINDRICAL_SURFACE('',#18325,4.5);
#1469=CYLINDRICAL_SURFACE('',#18326,4.5);
#1470=CYLINDRICAL_SURFACE('',#18328,3.933);
#1471=CYLINDRICAL_SURFACE('',#18330,3.933);
#1472=CYLINDRICAL_SURFACE('',#18331,3.933);
#1473=CYLINDRICAL_SURFACE('',#18332,3.933);
#1474=CYLINDRICAL_SURFACE('',#18333,3.933);
#1475=CYLINDRICAL_SURFACE('',#18334,3.933);
#1476=CYLINDRICAL_SURFACE('',#18335,3.933);
#1477=CYLINDRICAL_SURFACE('',#18336,3.933);
#1478=CYLINDRICAL_SURFACE('',#18337,3.933);
#1479=CYLINDRICAL_SURFACE('',#18338,3.933);
#1480=CYLINDRICAL_SURFACE('',#18340,3.22275);
#1481=CYLINDRICAL_SURFACE('',#18342,3.22275);
#1482=CYLINDRICAL_SURFACE('',#18343,3.22275);
#1483=CYLINDRICAL_SURFACE('',#18344,3.22275);
#1484=CYLINDRICAL_SURFACE('',#18345,3.22275);
#1485=CYLINDRICAL_SURFACE('',#18346,3.22275);
#1486=CYLINDRICAL_SURFACE('',#18347,3.22275);
#1487=CYLINDRICAL_SURFACE('',#18348,3.22275);
#1488=CYLINDRICAL_SURFACE('',#18349,3.22275);
#1489=CYLINDRICAL_SURFACE('',#18358,10.);
#1490=CYLINDRICAL_SURFACE('',#18365,3.22275);
#1491=CYLINDRICAL_SURFACE('',#18367,3.933);
#1492=CYLINDRICAL_SURFACE('',#18376,3.933);
#1493=CYLINDRICAL_SURFACE('',#18378,3.933);
#1494=CYLINDRICAL_SURFACE('',#18379,3.933);
#1495=CYLINDRICAL_SURFACE('',#18380,3.933);
#1496=CYLINDRICAL_SURFACE('',#18381,3.933);
#1497=CYLINDRICAL_SURFACE('',#18382,3.933);
#1498=CYLINDRICAL_SURFACE('',#18383,3.933);
#1499=CYLINDRICAL_SURFACE('',#18384,3.933);
#1500=CYLINDRICAL_SURFACE('',#18385,3.933);
#1501=CYLINDRICAL_SURFACE('',#18386,3.933);
#1502=CYLINDRICAL_SURFACE('',#18387,3.933);
#1503=CYLINDRICAL_SURFACE('',#18388,3.933);
#1504=CYLINDRICAL_SURFACE('',#18389,3.933);
#1505=CYLINDRICAL_SURFACE('',#18390,3.933);
#1506=CYLINDRICAL_SURFACE('',#18391,3.933);
#1507=CYLINDRICAL_SURFACE('',#18392,3.933);
#1508=CYLINDRICAL_SURFACE('',#18393,3.933);
#1509=CYLINDRICAL_SURFACE('',#18394,3.933);
#1510=CYLINDRICAL_SURFACE('',#18395,3.933);
#1511=CYLINDRICAL_SURFACE('',#18396,3.933);
#1512=CYLINDRICAL_SURFACE('',#18397,3.933);
#1513=CYLINDRICAL_SURFACE('',#18398,3.933);
#1514=CYLINDRICAL_SURFACE('',#18399,3.933);
#1515=CYLINDRICAL_SURFACE('',#18400,3.933);
#1516=CYLINDRICAL_SURFACE('',#18401,3.933);
#1517=CYLINDRICAL_SURFACE('',#18402,3.933);
#1518=CYLINDRICAL_SURFACE('',#18403,3.933);
#1519=CYLINDRICAL_SURFACE('',#18404,3.933);
#1520=CYLINDRICAL_SURFACE('',#18405,3.933);
#1521=CYLINDRICAL_SURFACE('',#18406,3.933);
#1522=CYLINDRICAL_SURFACE('',#18407,3.933);
#1523=CYLINDRICAL_SURFACE('',#18408,3.933);
#1524=CYLINDRICAL_SURFACE('',#18409,3.933);
#1525=CYLINDRICAL_SURFACE('',#18410,3.933);
#1526=CYLINDRICAL_SURFACE('',#18411,3.933);
#1527=CYLINDRICAL_SURFACE('',#18412,3.933);
#1528=CYLINDRICAL_SURFACE('',#18413,3.933);
#1529=CYLINDRICAL_SURFACE('',#18414,3.933);
#1530=CYLINDRICAL_SURFACE('',#18415,3.933);
#1531=CYLINDRICAL_SURFACE('',#18416,3.933);
#1532=CYLINDRICAL_SURFACE('',#18417,3.933);
#1533=CYLINDRICAL_SURFACE('',#18418,3.933);
#1534=CYLINDRICAL_SURFACE('',#18419,3.933);
#1535=CYLINDRICAL_SURFACE('',#18420,3.933);
#1536=CYLINDRICAL_SURFACE('',#18421,3.22275);
#1537=CYLINDRICAL_SURFACE('',#18423,3.22275);
#1538=CYLINDRICAL_SURFACE('',#18425,3.22275);
#1539=CYLINDRICAL_SURFACE('',#18426,3.22275);
#1540=CYLINDRICAL_SURFACE('',#18427,3.22275);
#1541=CYLINDRICAL_SURFACE('',#18428,3.22275);
#1542=CYLINDRICAL_SURFACE('',#18429,3.22275);
#1543=CYLINDRICAL_SURFACE('',#18430,3.22275);
#1544=CYLINDRICAL_SURFACE('',#18431,3.22275);
#1545=CYLINDRICAL_SURFACE('',#18432,3.22275);
#1546=CYLINDRICAL_SURFACE('',#18433,3.22275);
#1547=CYLINDRICAL_SURFACE('',#18434,3.22275);
#1548=CYLINDRICAL_SURFACE('',#18435,3.22275);
#1549=CYLINDRICAL_SURFACE('',#18436,3.22275);
#1550=CYLINDRICAL_SURFACE('',#18437,3.22275);
#1551=CYLINDRICAL_SURFACE('',#18438,3.22275);
#1552=CYLINDRICAL_SURFACE('',#18439,3.22275);
#1553=CYLINDRICAL_SURFACE('',#18440,3.22275);
#1554=CYLINDRICAL_SURFACE('',#18441,3.22275);
#1555=CYLINDRICAL_SURFACE('',#18442,3.22275);
#1556=CYLINDRICAL_SURFACE('',#18443,3.22275);
#1557=CYLINDRICAL_SURFACE('',#18444,3.22275);
#1558=CYLINDRICAL_SURFACE('',#18445,3.22275);
#1559=CYLINDRICAL_SURFACE('',#18446,3.22275);
#1560=CYLINDRICAL_SURFACE('',#18447,3.22275);
#1561=CYLINDRICAL_SURFACE('',#18448,3.22275);
#1562=CYLINDRICAL_SURFACE('',#18449,3.22275);
#1563=CYLINDRICAL_SURFACE('',#18450,3.22275);
#1564=CYLINDRICAL_SURFACE('',#18451,3.22275);
#1565=CYLINDRICAL_SURFACE('',#18452,3.22275);
#1566=CYLINDRICAL_SURFACE('',#18453,3.22275);
#1567=CYLINDRICAL_SURFACE('',#18454,3.22275);
#1568=CYLINDRICAL_SURFACE('',#18455,3.22275);
#1569=CYLINDRICAL_SURFACE('',#18456,3.22275);
#1570=CYLINDRICAL_SURFACE('',#18457,3.22275);
#1571=CYLINDRICAL_SURFACE('',#18458,3.22275);
#1572=CYLINDRICAL_SURFACE('',#18459,3.22275);
#1573=CYLINDRICAL_SURFACE('',#18460,3.22275);
#1574=CYLINDRICAL_SURFACE('',#18461,3.22275);
#1575=CYLINDRICAL_SURFACE('',#18462,3.22275);
#1576=CYLINDRICAL_SURFACE('',#18463,3.22275);
#1577=CYLINDRICAL_SURFACE('',#18464,3.22275);
#1578=CYLINDRICAL_SURFACE('',#18465,3.22275);
#1579=CYLINDRICAL_SURFACE('',#18466,3.22275);
#1580=CYLINDRICAL_SURFACE('',#18471,3.22275);
#1581=CYLINDRICAL_SURFACE('',#18486,3.933);
#1582=CYLINDRICAL_SURFACE('',#18488,3.933);
#1583=CYLINDRICAL_SURFACE('',#18490,3.933);
#1584=CYLINDRICAL_SURFACE('',#18491,3.933);
#1585=CYLINDRICAL_SURFACE('',#18492,3.933);
#1586=CYLINDRICAL_SURFACE('',#18493,3.933);
#1587=CYLINDRICAL_SURFACE('',#18494,3.933);
#1588=CYLINDRICAL_SURFACE('',#18495,3.933);
#1589=CYLINDRICAL_SURFACE('',#18496,3.933);
#1590=CYLINDRICAL_SURFACE('',#18497,3.933);
#1591=CYLINDRICAL_SURFACE('',#18498,3.933);
#1592=CYLINDRICAL_SURFACE('',#18499,3.933);
#1593=CYLINDRICAL_SURFACE('',#18500,3.933);
#1594=CYLINDRICAL_SURFACE('',#18501,3.933);
#1595=CYLINDRICAL_SURFACE('',#18502,3.933);
#1596=CYLINDRICAL_SURFACE('',#18503,3.933);
#1597=CYLINDRICAL_SURFACE('',#18504,3.933);
#1598=CYLINDRICAL_SURFACE('',#18505,3.933);
#1599=CYLINDRICAL_SURFACE('',#18506,3.933);
#1600=CYLINDRICAL_SURFACE('',#18507,3.933);
#1601=CYLINDRICAL_SURFACE('',#18508,3.933);
#1602=CYLINDRICAL_SURFACE('',#18509,3.933);
#1603=CYLINDRICAL_SURFACE('',#18510,3.933);
#1604=CYLINDRICAL_SURFACE('',#18511,3.933);
#1605=CYLINDRICAL_SURFACE('',#18512,3.933);
#1606=CYLINDRICAL_SURFACE('',#18513,3.933);
#1607=CYLINDRICAL_SURFACE('',#18514,3.933);
#1608=CYLINDRICAL_SURFACE('',#18515,3.933);
#1609=CYLINDRICAL_SURFACE('',#18516,3.933);
#1610=CYLINDRICAL_SURFACE('',#18517,3.933);
#1611=CYLINDRICAL_SURFACE('',#18518,3.933);
#1612=CYLINDRICAL_SURFACE('',#18519,3.933);
#1613=CYLINDRICAL_SURFACE('',#18520,3.933);
#1614=CYLINDRICAL_SURFACE('',#18521,3.933);
#1615=CYLINDRICAL_SURFACE('',#18522,3.933);
#1616=CYLINDRICAL_SURFACE('',#18523,3.933);
#1617=CYLINDRICAL_SURFACE('',#18524,3.933);
#1618=CYLINDRICAL_SURFACE('',#18525,3.933);
#1619=CYLINDRICAL_SURFACE('',#18526,3.933);
#1620=CYLINDRICAL_SURFACE('',#18527,3.933);
#1621=CYLINDRICAL_SURFACE('',#18528,3.933);
#1622=CYLINDRICAL_SURFACE('',#18529,3.933);
#1623=CYLINDRICAL_SURFACE('',#18530,3.933);
#1624=CYLINDRICAL_SURFACE('',#18531,3.933);
#1625=CYLINDRICAL_SURFACE('',#18532,3.933);
#1626=CYLINDRICAL_SURFACE('',#18533,3.933);
#1627=CYLINDRICAL_SURFACE('',#18534,3.933);
#1628=CYLINDRICAL_SURFACE('',#18535,3.933);
#1629=CYLINDRICAL_SURFACE('',#18536,3.933);
#1630=CYLINDRICAL_SURFACE('',#18537,3.933);
#1631=CYLINDRICAL_SURFACE('',#18538,3.933);
#1632=CYLINDRICAL_SURFACE('',#18539,3.933);
#1633=CYLINDRICAL_SURFACE('',#18540,3.933);
#1634=CYLINDRICAL_SURFACE('',#18541,3.933);
#1635=CYLINDRICAL_SURFACE('',#18542,3.933);
#1636=CYLINDRICAL_SURFACE('',#18543,3.933);
#1637=CYLINDRICAL_SURFACE('',#18544,3.933);
#1638=CYLINDRICAL_SURFACE('',#18545,3.933);
#1639=CYLINDRICAL_SURFACE('',#18546,3.933);
#1640=CYLINDRICAL_SURFACE('',#18547,3.933);
#1641=CYLINDRICAL_SURFACE('',#18548,3.933);
#1642=CYLINDRICAL_SURFACE('',#18549,3.933);
#1643=CYLINDRICAL_SURFACE('',#18550,3.933);
#1644=CYLINDRICAL_SURFACE('',#18551,3.933);
#1645=CYLINDRICAL_SURFACE('',#18552,3.933);
#1646=CYLINDRICAL_SURFACE('',#18553,3.933);
#1647=CYLINDRICAL_SURFACE('',#18554,3.933);
#1648=CYLINDRICAL_SURFACE('',#18555,3.933);
#1649=CYLINDRICAL_SURFACE('',#18556,3.933);
#1650=CYLINDRICAL_SURFACE('',#18557,3.933);
#1651=CYLINDRICAL_SURFACE('',#18558,3.933);
#1652=CYLINDRICAL_SURFACE('',#18559,3.933);
#1653=CYLINDRICAL_SURFACE('',#18560,3.933);
#1654=CYLINDRICAL_SURFACE('',#18561,3.933);
#1655=CYLINDRICAL_SURFACE('',#18562,3.933);
#1656=CYLINDRICAL_SURFACE('',#18563,3.933);
#1657=CYLINDRICAL_SURFACE('',#18564,3.933);
#1658=CYLINDRICAL_SURFACE('',#18565,3.933);
#1659=CYLINDRICAL_SURFACE('',#18566,3.933);
#1660=CYLINDRICAL_SURFACE('',#18567,3.933);
#1661=CYLINDRICAL_SURFACE('',#18568,3.933);
#1662=CYLINDRICAL_SURFACE('',#18569,3.933);
#1663=CYLINDRICAL_SURFACE('',#18570,3.933);
#1664=CYLINDRICAL_SURFACE('',#18571,3.933);
#1665=CYLINDRICAL_SURFACE('',#18572,3.933);
#1666=CYLINDRICAL_SURFACE('',#18573,3.933);
#1667=CYLINDRICAL_SURFACE('',#18574,3.933);
#1668=CYLINDRICAL_SURFACE('',#18575,3.933);
#1669=CYLINDRICAL_SURFACE('',#18576,3.933);
#1670=CYLINDRICAL_SURFACE('',#18577,3.22275);
#1671=CYLINDRICAL_SURFACE('',#18579,3.22275);
#1672=CYLINDRICAL_SURFACE('',#18581,3.22275);
#1673=CYLINDRICAL_SURFACE('',#18582,3.22275);
#1674=CYLINDRICAL_SURFACE('',#18583,3.22275);
#1675=CYLINDRICAL_SURFACE('',#18584,3.22275);
#1676=CYLINDRICAL_SURFACE('',#18585,3.22275);
#1677=CYLINDRICAL_SURFACE('',#18586,3.22275);
#1678=CYLINDRICAL_SURFACE('',#18587,3.22275);
#1679=CYLINDRICAL_SURFACE('',#18588,3.22275);
#1680=CYLINDRICAL_SURFACE('',#18589,3.22275);
#1681=CYLINDRICAL_SURFACE('',#18590,3.22275);
#1682=CYLINDRICAL_SURFACE('',#18591,3.22275);
#1683=CYLINDRICAL_SURFACE('',#18592,3.22275);
#1684=CYLINDRICAL_SURFACE('',#18593,3.22275);
#1685=CYLINDRICAL_SURFACE('',#18594,3.22275);
#1686=CYLINDRICAL_SURFACE('',#18595,3.22275);
#1687=CYLINDRICAL_SURFACE('',#18596,3.22275);
#1688=CYLINDRICAL_SURFACE('',#18597,3.22275);
#1689=CYLINDRICAL_SURFACE('',#18598,3.22275);
#1690=CYLINDRICAL_SURFACE('',#18599,3.22275);
#1691=CYLINDRICAL_SURFACE('',#18600,3.22275);
#1692=CYLINDRICAL_SURFACE('',#18601,3.22275);
#1693=CYLINDRICAL_SURFACE('',#18602,3.22275);
#1694=CYLINDRICAL_SURFACE('',#18603,3.22275);
#1695=CYLINDRICAL_SURFACE('',#18604,3.22275);
#1696=CYLINDRICAL_SURFACE('',#18605,3.22275);
#1697=CYLINDRICAL_SURFACE('',#18606,3.22275);
#1698=CYLINDRICAL_SURFACE('',#18607,3.22275);
#1699=CYLINDRICAL_SURFACE('',#18608,3.22275);
#1700=CYLINDRICAL_SURFACE('',#18609,3.22275);
#1701=CYLINDRICAL_SURFACE('',#18610,3.22275);
#1702=CYLINDRICAL_SURFACE('',#18611,3.22275);
#1703=CYLINDRICAL_SURFACE('',#18612,3.22275);
#1704=CYLINDRICAL_SURFACE('',#18613,3.22275);
#1705=CYLINDRICAL_SURFACE('',#18614,3.22275);
#1706=CYLINDRICAL_SURFACE('',#18615,3.22275);
#1707=CYLINDRICAL_SURFACE('',#18616,3.22275);
#1708=CYLINDRICAL_SURFACE('',#18617,3.22275);
#1709=CYLINDRICAL_SURFACE('',#18618,3.22275);
#1710=CYLINDRICAL_SURFACE('',#18619,3.22275);
#1711=CYLINDRICAL_SURFACE('',#18620,3.22275);
#1712=CYLINDRICAL_SURFACE('',#18621,3.22275);
#1713=CYLINDRICAL_SURFACE('',#18622,3.22275);
#1714=CYLINDRICAL_SURFACE('',#18623,3.22275);
#1715=CYLINDRICAL_SURFACE('',#18624,3.22275);
#1716=CYLINDRICAL_SURFACE('',#18625,3.22275);
#1717=CYLINDRICAL_SURFACE('',#18626,3.22275);
#1718=CYLINDRICAL_SURFACE('',#18627,3.22275);
#1719=CYLINDRICAL_SURFACE('',#18628,3.22275);
#1720=CYLINDRICAL_SURFACE('',#18629,3.22275);
#1721=CYLINDRICAL_SURFACE('',#18630,3.22275);
#1722=CYLINDRICAL_SURFACE('',#18631,3.22275);
#1723=CYLINDRICAL_SURFACE('',#18632,3.22275);
#1724=CYLINDRICAL_SURFACE('',#18633,3.22275);
#1725=CYLINDRICAL_SURFACE('',#18634,3.22275);
#1726=CYLINDRICAL_SURFACE('',#18635,3.22275);
#1727=CYLINDRICAL_SURFACE('',#18636,3.22275);
#1728=CYLINDRICAL_SURFACE('',#18637,3.22275);
#1729=CYLINDRICAL_SURFACE('',#18638,3.22275);
#1730=CYLINDRICAL_SURFACE('',#18639,3.22275);
#1731=CYLINDRICAL_SURFACE('',#18640,3.22275);
#1732=CYLINDRICAL_SURFACE('',#18641,3.22275);
#1733=CYLINDRICAL_SURFACE('',#18642,3.22275);
#1734=CYLINDRICAL_SURFACE('',#18643,3.22275);
#1735=CYLINDRICAL_SURFACE('',#18644,3.22275);
#1736=CYLINDRICAL_SURFACE('',#18645,3.22275);
#1737=CYLINDRICAL_SURFACE('',#18646,3.22275);
#1738=CYLINDRICAL_SURFACE('',#18647,3.22275);
#1739=CYLINDRICAL_SURFACE('',#18648,3.22275);
#1740=CYLINDRICAL_SURFACE('',#18649,3.22275);
#1741=CYLINDRICAL_SURFACE('',#18650,3.22275);
#1742=CYLINDRICAL_SURFACE('',#18651,3.22275);
#1743=CYLINDRICAL_SURFACE('',#18652,3.22275);
#1744=CYLINDRICAL_SURFACE('',#18653,3.22275);
#1745=CYLINDRICAL_SURFACE('',#18654,3.22275);
#1746=CYLINDRICAL_SURFACE('',#18655,3.22275);
#1747=CYLINDRICAL_SURFACE('',#18656,3.22275);
#1748=CYLINDRICAL_SURFACE('',#18657,3.22275);
#1749=CYLINDRICAL_SURFACE('',#18658,3.22275);
#1750=CYLINDRICAL_SURFACE('',#18659,3.22275);
#1751=CYLINDRICAL_SURFACE('',#18660,3.22275);
#1752=CYLINDRICAL_SURFACE('',#18661,3.22275);
#1753=CYLINDRICAL_SURFACE('',#18662,3.22275);
#1754=CYLINDRICAL_SURFACE('',#18663,3.22275);
#1755=CYLINDRICAL_SURFACE('',#18664,3.22275);
#1756=CYLINDRICAL_SURFACE('',#18665,3.22275);
#1757=CYLINDRICAL_SURFACE('',#18666,3.22275);
#1758=CYLINDRICAL_SURFACE('',#18671,3.22275);
#1759=CYLINDRICAL_SURFACE('',#18686,3.933);
#1760=CYLINDRICAL_SURFACE('',#18724,4.05);
#1761=(
BOUNDED_CURVE()
B_SPLINE_CURVE(2,(#22976,#22977,#22978),.UNSPECIFIED.,.F.,.F.)
B_SPLINE_CURVE_WITH_KNOTS((3,3),(0.,1.67588266328234),.UNSPECIFIED.)
CURVE()
GEOMETRIC_REPRESENTATION_ITEM()
RATIONAL_B_SPLINE_CURVE((1.,1.00126993326289,1.))
REPRESENTATION_ITEM('')
);
#1762=(
BOUNDED_CURVE()
B_SPLINE_CURVE(2,(#23047,#23048,#23049),.UNSPECIFIED.,.F.,.F.)
B_SPLINE_CURVE_WITH_KNOTS((3,3),(0.,1.67588266328234),.UNSPECIFIED.)
CURVE()
GEOMETRIC_REPRESENTATION_ITEM()
RATIONAL_B_SPLINE_CURVE((1.,1.00126993326289,1.))
REPRESENTATION_ITEM('')
);
#1763=(
BOUNDED_CURVE()
B_SPLINE_CURVE(2,(#23196,#23197,#23198),.UNSPECIFIED.,.F.,.F.)
B_SPLINE_CURVE_WITH_KNOTS((3,3),(0.,1.67588266328234),.UNSPECIFIED.)
CURVE()
GEOMETRIC_REPRESENTATION_ITEM()
RATIONAL_B_SPLINE_CURVE((1.,1.00126993326289,1.))
REPRESENTATION_ITEM('')
);
#1764=(
BOUNDED_CURVE()
B_SPLINE_CURVE(2,(#23235,#23236,#23237),.UNSPECIFIED.,.F.,.F.)
B_SPLINE_CURVE_WITH_KNOTS((3,3),(0.,1.67588266328234),.UNSPECIFIED.)
CURVE()
GEOMETRIC_REPRESENTATION_ITEM()
RATIONAL_B_SPLINE_CURVE((1.,1.00126993326289,1.))
REPRESENTATION_ITEM('')
);
#1765=(
BOUNDED_CURVE()
B_SPLINE_CURVE(2,(#33362,#33363,#33364),.UNSPECIFIED.,.F.,.F.)
B_SPLINE_CURVE_WITH_KNOTS((3,3),(0.146919729838694,0.206437955014875),
 .UNSPECIFIED.)
CURVE()
GEOMETRIC_REPRESENTATION_ITEM()
RATIONAL_B_SPLINE_CURVE((1.00910808226728,1.00963997887916,1.00910808226728))
REPRESENTATION_ITEM('')
);
#1766=(
BOUNDED_CURVE()
B_SPLINE_CURVE(2,(#33395,#33396,#33397),.UNSPECIFIED.,.F.,.F.)
B_SPLINE_CURVE_WITH_KNOTS((3,3),(0.146919729838686,0.206437955014868),
 .UNSPECIFIED.)
CURVE()
GEOMETRIC_REPRESENTATION_ITEM()
RATIONAL_B_SPLINE_CURVE((1.00910808226729,1.00963997887916,1.00910808226729))
REPRESENTATION_ITEM('')
);
#1767=(
BOUNDED_CURVE()
B_SPLINE_CURVE(2,(#33403,#33404,#33405),.UNSPECIFIED.,.F.,.F.)
B_SPLINE_CURVE_WITH_KNOTS((3,3),(0.146919729838689,0.206437955014871),
 .UNSPECIFIED.)
CURVE()
GEOMETRIC_REPRESENTATION_ITEM()
RATIONAL_B_SPLINE_CURVE((1.00910808226729,1.00963997887917,1.00910808226729))
REPRESENTATION_ITEM('')
);
#1768=(
BOUNDED_CURVE()
B_SPLINE_CURVE(2,(#33436,#33437,#33438),.UNSPECIFIED.,.F.,.F.)
B_SPLINE_CURVE_WITH_KNOTS((3,3),(0.146919729838686,0.206437955014869),
 .UNSPECIFIED.)
CURVE()
GEOMETRIC_REPRESENTATION_ITEM()
RATIONAL_B_SPLINE_CURVE((1.00910808226729,1.00963997887916,1.00910808226729))
REPRESENTATION_ITEM('')
);
#1769=(
BOUNDED_CURVE()
B_SPLINE_CURVE(2,(#33444,#33445,#33446),.UNSPECIFIED.,.F.,.F.)
B_SPLINE_CURVE_WITH_KNOTS((3,3),(0.146919729838686,0.206437955014868),
 .UNSPECIFIED.)
CURVE()
GEOMETRIC_REPRESENTATION_ITEM()
RATIONAL_B_SPLINE_CURVE((1.00910808226729,1.00963997887916,1.00910808226729))
REPRESENTATION_ITEM('')
);
#1770=(
BOUNDED_CURVE()
B_SPLINE_CURVE(2,(#33452,#33453,#33454),.UNSPECIFIED.,.F.,.F.)
B_SPLINE_CURVE_WITH_KNOTS((3,3),(0.146919729838688,0.20643795501487),
 .UNSPECIFIED.)
CURVE()
GEOMETRIC_REPRESENTATION_ITEM()
RATIONAL_B_SPLINE_CURVE((1.00910808226729,1.00963997887916,1.00910808226729))
REPRESENTATION_ITEM('')
);
#1771=(
BOUNDED_CURVE()
B_SPLINE_CURVE(2,(#33458,#33459,#33460),.UNSPECIFIED.,.F.,.F.)
B_SPLINE_CURVE_WITH_KNOTS((3,3),(0.18541928992188,1.11813591586374),
 .UNSPECIFIED.)
CURVE()
GEOMETRIC_REPRESENTATION_ITEM()
RATIONAL_B_SPLINE_CURVE((1.06825177535134,1.21144876302791,1.06825177535134))
REPRESENTATION_ITEM('')
);
#1772=(
BOUNDED_CURVE()
B_SPLINE_CURVE(2,(#33462,#33463,#33464),.UNSPECIFIED.,.F.,.F.)
B_SPLINE_CURVE_WITH_KNOTS((3,3),(0.18541928992188,1.11813591586374),
 .UNSPECIFIED.)
CURVE()
GEOMETRIC_REPRESENTATION_ITEM()
RATIONAL_B_SPLINE_CURVE((1.06825177535134,1.21144876302791,1.06825177535134))
REPRESENTATION_ITEM('')
);
#1773=(
BOUNDED_CURVE()
B_SPLINE_CURVE(2,(#33466,#33467,#33468),.UNSPECIFIED.,.F.,.F.)
B_SPLINE_CURVE_WITH_KNOTS((3,3),(0.18541928992188,1.11813591586374),
 .UNSPECIFIED.)
CURVE()
GEOMETRIC_REPRESENTATION_ITEM()
RATIONAL_B_SPLINE_CURVE((1.06825177535134,1.21144876302791,1.06825177535134))
REPRESENTATION_ITEM('')
);
#1774=(
BOUNDED_CURVE()
B_SPLINE_CURVE(2,(#33474,#33475,#33476),.UNSPECIFIED.,.F.,.F.)
B_SPLINE_CURVE_WITH_KNOTS((3,3),(0.18541928992188,0.651777602892792),
 .UNSPECIFIED.)
CURVE()
GEOMETRIC_REPRESENTATION_ITEM()
RATIONAL_B_SPLINE_CURVE((1.06825177535134,1.13985026918962,1.13985026918963))
REPRESENTATION_ITEM('')
);
#1775=(
BOUNDED_CURVE()
B_SPLINE_CURVE(2,(#33477,#33478,#33479),.UNSPECIFIED.,.F.,.F.)
B_SPLINE_CURVE_WITH_KNOTS((3,3),(0.18541928992188,1.11813591586374),
 .UNSPECIFIED.)
CURVE()
GEOMETRIC_REPRESENTATION_ITEM()
RATIONAL_B_SPLINE_CURVE((1.06825177535134,1.21144876302791,1.06825177535134))
REPRESENTATION_ITEM('')
);
#1776=(
BOUNDED_CURVE()
B_SPLINE_CURVE(2,(#33480,#33481,#33482),.UNSPECIFIED.,.F.,.F.)
B_SPLINE_CURVE_WITH_KNOTS((3,3),(0.18541928992188,1.11813591586374),
 .UNSPECIFIED.)
CURVE()
GEOMETRIC_REPRESENTATION_ITEM()
RATIONAL_B_SPLINE_CURVE((1.06825177535134,1.21144876302791,1.06825177535134))
REPRESENTATION_ITEM('')
);
#1777=(
BOUNDED_CURVE()
B_SPLINE_CURVE(2,(#33483,#33484,#33485),.UNSPECIFIED.,.F.,.F.)
B_SPLINE_CURVE_WITH_KNOTS((3,3),(0.651777602892792,1.11813591586374),
 .UNSPECIFIED.)
CURVE()
GEOMETRIC_REPRESENTATION_ITEM()
RATIONAL_B_SPLINE_CURVE((1.13985026918963,1.13985026918963,1.06825177535134))
REPRESENTATION_ITEM('')
);
#1778=(
BOUNDED_CURVE()
B_SPLINE_CURVE(2,(#44307,#44308,#44309),.UNSPECIFIED.,.F.,.F.)
B_SPLINE_CURVE_WITH_KNOTS((3,3),(0.149747849205877,0.971656649213287),
 .UNSPECIFIED.)
CURVE()
GEOMETRIC_REPRESENTATION_ITEM()
RATIONAL_B_SPLINE_CURVE((1.07140024848293,1.23714644374248,1.07140024848293))
REPRESENTATION_ITEM('')
);
#1779=(
BOUNDED_CURVE()
B_SPLINE_CURVE(2,(#44311,#44312,#44313),.UNSPECIFIED.,.F.,.F.)
B_SPLINE_CURVE_WITH_KNOTS((3,3),(0.149747849205876,0.971656649213287),
 .UNSPECIFIED.)
CURVE()
GEOMETRIC_REPRESENTATION_ITEM()
RATIONAL_B_SPLINE_CURVE((1.07140024848293,1.23714644374248,1.07140024848293))
REPRESENTATION_ITEM('')
);
#1780=(
BOUNDED_CURVE()
B_SPLINE_CURVE(2,(#44315,#44316,#44317),.UNSPECIFIED.,.F.,.F.)
B_SPLINE_CURVE_WITH_KNOTS((3,3),(0.149747849205877,0.971656649213287),
 .UNSPECIFIED.)
CURVE()
GEOMETRIC_REPRESENTATION_ITEM()
RATIONAL_B_SPLINE_CURVE((1.07140024848293,1.23714644374248,1.07140024848293))
REPRESENTATION_ITEM('')
);
#1781=(
BOUNDED_CURVE()
B_SPLINE_CURVE(2,(#44319,#44320,#44321),.UNSPECIFIED.,.F.,.F.)
B_SPLINE_CURVE_WITH_KNOTS((3,3),(0.149747849205876,0.971656649213287),
 .UNSPECIFIED.)
CURVE()
GEOMETRIC_REPRESENTATION_ITEM()
RATIONAL_B_SPLINE_CURVE((1.07140024848293,1.23714644374248,1.07140024848293))
REPRESENTATION_ITEM('')
);
#1782=(
BOUNDED_CURVE()
B_SPLINE_CURVE(2,(#44323,#44324,#44325),.UNSPECIFIED.,.F.,.F.)
B_SPLINE_CURVE_WITH_KNOTS((3,3),(0.560702249209475,0.971656649213286),
 .UNSPECIFIED.)
CURVE()
GEOMETRIC_REPRESENTATION_ITEM()
RATIONAL_B_SPLINE_CURVE((1.1542733461127,1.15427334611272,1.07140024848293))
REPRESENTATION_ITEM('')
);
#1783=(
BOUNDED_CURVE()
B_SPLINE_CURVE(2,(#44330,#44331,#44332),.UNSPECIFIED.,.F.,.F.)
B_SPLINE_CURVE_WITH_KNOTS((3,3),(0.149747849205877,0.560702249209475),
 .UNSPECIFIED.)
CURVE()
GEOMETRIC_REPRESENTATION_ITEM()
RATIONAL_B_SPLINE_CURVE((1.07140024848293,1.15427334611268,1.1542733461127))
REPRESENTATION_ITEM('')
);
#1784=(
BOUNDED_CURVE()
B_SPLINE_CURVE(2,(#44333,#44334,#44335),.UNSPECIFIED.,.F.,.F.)
B_SPLINE_CURVE_WITH_KNOTS((3,3),(0.149747849205877,0.971656649213287),
 .UNSPECIFIED.)
CURVE()
GEOMETRIC_REPRESENTATION_ITEM()
RATIONAL_B_SPLINE_CURVE((1.07140024848293,1.23714644374248,1.07140024848293))
REPRESENTATION_ITEM('')
);
#1785=(
BOUNDED_CURVE()
B_SPLINE_CURVE(2,(#55860,#55861,#55862),.UNSPECIFIED.,.F.,.F.)
B_SPLINE_CURVE_WITH_KNOTS((3,3),(0.149747849205877,0.971656649213287),
 .UNSPECIFIED.)
CURVE()
GEOMETRIC_REPRESENTATION_ITEM()
RATIONAL_B_SPLINE_CURVE((1.07140024848293,1.23714644374248,1.07140024848293))
REPRESENTATION_ITEM('')
);
#1786=(
BOUNDED_CURVE()
B_SPLINE_CURVE(2,(#55864,#55865,#55866),.UNSPECIFIED.,.F.,.F.)
B_SPLINE_CURVE_WITH_KNOTS((3,3),(0.149747849205876,0.971656649213287),
 .UNSPECIFIED.)
CURVE()
GEOMETRIC_REPRESENTATION_ITEM()
RATIONAL_B_SPLINE_CURVE((1.07140024848293,1.23714644374248,1.07140024848293))
REPRESENTATION_ITEM('')
);
#1787=(
BOUNDED_CURVE()
B_SPLINE_CURVE(2,(#55868,#55869,#55870),.UNSPECIFIED.,.F.,.F.)
B_SPLINE_CURVE_WITH_KNOTS((3,3),(0.149747849205877,0.971656649213287),
 .UNSPECIFIED.)
CURVE()
GEOMETRIC_REPRESENTATION_ITEM()
RATIONAL_B_SPLINE_CURVE((1.07140024848293,1.23714644374248,1.07140024848293))
REPRESENTATION_ITEM('')
);
#1788=(
BOUNDED_CURVE()
B_SPLINE_CURVE(2,(#55872,#55873,#55874),.UNSPECIFIED.,.F.,.F.)
B_SPLINE_CURVE_WITH_KNOTS((3,3),(0.149747849205876,0.971656649213287),
 .UNSPECIFIED.)
CURVE()
GEOMETRIC_REPRESENTATION_ITEM()
RATIONAL_B_SPLINE_CURVE((1.07140024848293,1.23714644374248,1.07140024848293))
REPRESENTATION_ITEM('')
);
#1789=(
BOUNDED_CURVE()
B_SPLINE_CURVE(2,(#55876,#55877,#55878),.UNSPECIFIED.,.F.,.F.)
B_SPLINE_CURVE_WITH_KNOTS((3,3),(0.560702249209475,0.971656649213286),
 .UNSPECIFIED.)
CURVE()
GEOMETRIC_REPRESENTATION_ITEM()
RATIONAL_B_SPLINE_CURVE((1.1542733461127,1.15427334611272,1.07140024848293))
REPRESENTATION_ITEM('')
);
#1790=(
BOUNDED_CURVE()
B_SPLINE_CURVE(2,(#55883,#55884,#55885),.UNSPECIFIED.,.F.,.F.)
B_SPLINE_CURVE_WITH_KNOTS((3,3),(0.149747849205877,0.560702249209475),
 .UNSPECIFIED.)
CURVE()
GEOMETRIC_REPRESENTATION_ITEM()
RATIONAL_B_SPLINE_CURVE((1.07140024848293,1.15427334611268,1.1542733461127))
REPRESENTATION_ITEM('')
);
#1791=(
BOUNDED_CURVE()
B_SPLINE_CURVE(2,(#55886,#55887,#55888),.UNSPECIFIED.,.F.,.F.)
B_SPLINE_CURVE_WITH_KNOTS((3,3),(0.149747849205877,0.971656649213287),
 .UNSPECIFIED.)
CURVE()
GEOMETRIC_REPRESENTATION_ITEM()
RATIONAL_B_SPLINE_CURVE((1.07140024848293,1.23714644374248,1.07140024848293))
REPRESENTATION_ITEM('')
);
#1792=(
BOUNDED_CURVE()
B_SPLINE_CURVE(2,(#56398,#56399,#56400),.UNSPECIFIED.,.F.,.F.)
B_SPLINE_CURVE_WITH_KNOTS((3,3),(0.118301700433499,0.165554978945076),
 .UNSPECIFIED.)
CURVE()
GEOMETRIC_REPRESENTATION_ITEM()
RATIONAL_B_SPLINE_CURVE((1.0089042769369,1.00941185088304,1.0089042769369))
REPRESENTATION_ITEM('')
);
#1793=(
BOUNDED_CURVE()
B_SPLINE_CURVE(2,(#56431,#56432,#56433),.UNSPECIFIED.,.F.,.F.)
B_SPLINE_CURVE_WITH_KNOTS((3,3),(0.118301700433498,0.165554978945076),
 .UNSPECIFIED.)
CURVE()
GEOMETRIC_REPRESENTATION_ITEM()
RATIONAL_B_SPLINE_CURVE((1.00890427693691,1.00941185088304,1.00890427693691))
REPRESENTATION_ITEM('')
);
#1794=(
BOUNDED_CURVE()
B_SPLINE_CURVE(2,(#56439,#56440,#56441),.UNSPECIFIED.,.F.,.F.)
B_SPLINE_CURVE_WITH_KNOTS((3,3),(0.118301700433499,0.165554978945077),
 .UNSPECIFIED.)
CURVE()
GEOMETRIC_REPRESENTATION_ITEM()
RATIONAL_B_SPLINE_CURVE((1.0089042769369,1.00941185088304,1.0089042769369))
REPRESENTATION_ITEM('')
);
#1795=(
BOUNDED_CURVE()
B_SPLINE_CURVE(2,(#56472,#56473,#56474),.UNSPECIFIED.,.F.,.F.)
B_SPLINE_CURVE_WITH_KNOTS((3,3),(0.118301700433496,0.165554978945074),
 .UNSPECIFIED.)
CURVE()
GEOMETRIC_REPRESENTATION_ITEM()
RATIONAL_B_SPLINE_CURVE((1.0089042769369,1.00941185088304,1.0089042769369))
REPRESENTATION_ITEM('')
);
#1796=(
BOUNDED_CURVE()
B_SPLINE_CURVE(2,(#56480,#56481,#56482),.UNSPECIFIED.,.F.,.F.)
B_SPLINE_CURVE_WITH_KNOTS((3,3),(0.118301700433498,0.165554978945076),
 .UNSPECIFIED.)
CURVE()
GEOMETRIC_REPRESENTATION_ITEM()
RATIONAL_B_SPLINE_CURVE((1.00890427693691,1.00941185088304,1.00890427693691))
REPRESENTATION_ITEM('')
);
#1797=(
BOUNDED_CURVE()
B_SPLINE_CURVE(2,(#56488,#56489,#56490),.UNSPECIFIED.,.F.,.F.)
B_SPLINE_CURVE_WITH_KNOTS((3,3),(0.118301700433497,0.165554978945074),
 .UNSPECIFIED.)
CURVE()
GEOMETRIC_REPRESENTATION_ITEM()
RATIONAL_B_SPLINE_CURVE((1.00890427693689,1.00941185088303,1.00890427693689))
REPRESENTATION_ITEM('')
);
#1798=(
BOUNDED_CURVE()
B_SPLINE_CURVE(2,(#56494,#56495,#56496),.UNSPECIFIED.,.F.,.F.)
B_SPLINE_CURVE_WITH_KNOTS((3,3),(0.17570560818583,0.94569889023331),
 .UNSPECIFIED.)
CURVE()
GEOMETRIC_REPRESENTATION_ITEM()
RATIONAL_B_SPLINE_CURVE((1.0815388920082,1.2270078002172,1.08153889200821))
REPRESENTATION_ITEM('')
);
#1799=(
BOUNDED_CURVE()
B_SPLINE_CURVE(2,(#56498,#56499,#56500),.UNSPECIFIED.,.F.,.F.)
B_SPLINE_CURVE_WITH_KNOTS((3,3),(0.17570560818583,0.945698890233311),
 .UNSPECIFIED.)
CURVE()
GEOMETRIC_REPRESENTATION_ITEM()
RATIONAL_B_SPLINE_CURVE((1.0815388920082,1.2270078002172,1.08153889200821))
REPRESENTATION_ITEM('')
);
#1800=(
BOUNDED_CURVE()
B_SPLINE_CURVE(2,(#56502,#56503,#56504),.UNSPECIFIED.,.F.,.F.)
B_SPLINE_CURVE_WITH_KNOTS((3,3),(0.17570560818583,0.94569889023331),
 .UNSPECIFIED.)
CURVE()
GEOMETRIC_REPRESENTATION_ITEM()
RATIONAL_B_SPLINE_CURVE((1.0815388920082,1.2270078002172,1.08153889200821))
REPRESENTATION_ITEM('')
);
#1801=(
BOUNDED_CURVE()
B_SPLINE_CURVE(2,(#56510,#56511,#56512),.UNSPECIFIED.,.F.,.F.)
B_SPLINE_CURVE_WITH_KNOTS((3,3),(0.17570560818583,0.560702249209475),
 .UNSPECIFIED.)
CURVE()
GEOMETRIC_REPRESENTATION_ITEM()
RATIONAL_B_SPLINE_CURVE((1.0815388920082,1.15427334611268,1.1542733461127))
REPRESENTATION_ITEM('')
);
#1802=(
BOUNDED_CURVE()
B_SPLINE_CURVE(2,(#56513,#56514,#56515),.UNSPECIFIED.,.F.,.F.)
B_SPLINE_CURVE_WITH_KNOTS((3,3),(0.17570560818583,0.945698890233311),
 .UNSPECIFIED.)
CURVE()
GEOMETRIC_REPRESENTATION_ITEM()
RATIONAL_B_SPLINE_CURVE((1.0815388920082,1.2270078002172,1.08153889200821))
REPRESENTATION_ITEM('')
);
#1803=(
BOUNDED_CURVE()
B_SPLINE_CURVE(2,(#56516,#56517,#56518),.UNSPECIFIED.,.F.,.F.)
B_SPLINE_CURVE_WITH_KNOTS((3,3),(0.17570560818583,0.945698890233311),
 .UNSPECIFIED.)
CURVE()
GEOMETRIC_REPRESENTATION_ITEM()
RATIONAL_B_SPLINE_CURVE((1.0815388920082,1.2270078002172,1.08153889200821))
REPRESENTATION_ITEM('')
);
#1804=(
BOUNDED_CURVE()
B_SPLINE_CURVE(2,(#56519,#56520,#56521),.UNSPECIFIED.,.F.,.F.)
B_SPLINE_CURVE_WITH_KNOTS((3,3),(0.560702249209475,0.94569889023331),
 .UNSPECIFIED.)
CURVE()
GEOMETRIC_REPRESENTATION_ITEM()
RATIONAL_B_SPLINE_CURVE((1.1542733461127,1.15427334611272,1.08153889200821))
REPRESENTATION_ITEM('')
);
#1805=FACE_OUTER_BOUND('',#2778,.T.);
#1806=FACE_OUTER_BOUND('',#2779,.T.);
#1807=FACE_OUTER_BOUND('',#2780,.T.);
#1808=FACE_OUTER_BOUND('',#2781,.T.);
#1809=FACE_OUTER_BOUND('',#2782,.T.);
#1810=FACE_OUTER_BOUND('',#2783,.T.);
#1811=FACE_OUTER_BOUND('',#2784,.T.);
#1812=FACE_OUTER_BOUND('',#2785,.T.);
#1813=FACE_OUTER_BOUND('',#2786,.T.);
#1814=FACE_OUTER_BOUND('',#2787,.T.);
#1815=FACE_OUTER_BOUND('',#2791,.T.);
#1816=FACE_OUTER_BOUND('',#2792,.T.);
#1817=FACE_OUTER_BOUND('',#2793,.T.);
#1818=FACE_OUTER_BOUND('',#2797,.T.);
#1819=FACE_OUTER_BOUND('',#2798,.T.);
#1820=FACE_OUTER_BOUND('',#2799,.T.);
#1821=FACE_OUTER_BOUND('',#2800,.T.);
#1822=FACE_OUTER_BOUND('',#2801,.T.);
#1823=FACE_OUTER_BOUND('',#2802,.T.);
#1824=FACE_OUTER_BOUND('',#2803,.T.);
#1825=FACE_OUTER_BOUND('',#2804,.T.);
#1826=FACE_OUTER_BOUND('',#2805,.T.);
#1827=FACE_OUTER_BOUND('',#2806,.T.);
#1828=FACE_OUTER_BOUND('',#2813,.T.);
#1829=FACE_OUTER_BOUND('',#2814,.T.);
#1830=FACE_OUTER_BOUND('',#2818,.T.);
#1831=FACE_OUTER_BOUND('',#2819,.T.);
#1832=FACE_OUTER_BOUND('',#2820,.T.);
#1833=FACE_OUTER_BOUND('',#2821,.T.);
#1834=FACE_OUTER_BOUND('',#2825,.T.);
#1835=FACE_OUTER_BOUND('',#2826,.T.);
#1836=FACE_OUTER_BOUND('',#2827,.T.);
#1837=FACE_OUTER_BOUND('',#2835,.T.);
#1838=FACE_OUTER_BOUND('',#2836,.T.);
#1839=FACE_OUTER_BOUND('',#2837,.T.);
#1840=FACE_OUTER_BOUND('',#2838,.T.);
#1841=FACE_OUTER_BOUND('',#2839,.T.);
#1842=FACE_OUTER_BOUND('',#2840,.T.);
#1843=FACE_OUTER_BOUND('',#2841,.T.);
#1844=FACE_OUTER_BOUND('',#2842,.T.);
#1845=FACE_OUTER_BOUND('',#2843,.T.);
#1846=FACE_OUTER_BOUND('',#2844,.T.);
#1847=FACE_OUTER_BOUND('',#2845,.T.);
#1848=FACE_OUTER_BOUND('',#2846,.T.);
#1849=FACE_OUTER_BOUND('',#2847,.T.);
#1850=FACE_OUTER_BOUND('',#2848,.T.);
#1851=FACE_OUTER_BOUND('',#2849,.T.);
#1852=FACE_OUTER_BOUND('',#2850,.T.);
#1853=FACE_OUTER_BOUND('',#2851,.T.);
#1854=FACE_OUTER_BOUND('',#2852,.T.);
#1855=FACE_OUTER_BOUND('',#2853,.T.);
#1856=FACE_OUTER_BOUND('',#2854,.T.);
#1857=FACE_OUTER_BOUND('',#2855,.T.);
#1858=FACE_OUTER_BOUND('',#2856,.T.);
#1859=FACE_OUTER_BOUND('',#2857,.T.);
#1860=FACE_OUTER_BOUND('',#2858,.T.);
#1861=FACE_OUTER_BOUND('',#2859,.T.);
#1862=FACE_OUTER_BOUND('',#2860,.T.);
#1863=FACE_OUTER_BOUND('',#2861,.T.);
#1864=FACE_OUTER_BOUND('',#2862,.T.);
#1865=FACE_OUTER_BOUND('',#2863,.T.);
#1866=FACE_OUTER_BOUND('',#2864,.T.);
#1867=FACE_OUTER_BOUND('',#2865,.T.);
#1868=FACE_OUTER_BOUND('',#2866,.T.);
#1869=FACE_OUTER_BOUND('',#2867,.T.);
#1870=FACE_OUTER_BOUND('',#2868,.T.);
#1871=FACE_OUTER_BOUND('',#2869,.T.);
#1872=FACE_OUTER_BOUND('',#2870,.T.);
#1873=FACE_OUTER_BOUND('',#2871,.T.);
#1874=FACE_OUTER_BOUND('',#2872,.T.);
#1875=FACE_OUTER_BOUND('',#2873,.T.);
#1876=FACE_OUTER_BOUND('',#2874,.T.);
#1877=FACE_OUTER_BOUND('',#2875,.T.);
#1878=FACE_OUTER_BOUND('',#2876,.T.);
#1879=FACE_OUTER_BOUND('',#2877,.T.);
#1880=FACE_OUTER_BOUND('',#2878,.T.);
#1881=FACE_OUTER_BOUND('',#2879,.T.);
#1882=FACE_OUTER_BOUND('',#2880,.T.);
#1883=FACE_OUTER_BOUND('',#2881,.T.);
#1884=FACE_OUTER_BOUND('',#2882,.T.);
#1885=FACE_OUTER_BOUND('',#2883,.T.);
#1886=FACE_OUTER_BOUND('',#2884,.T.);
#1887=FACE_OUTER_BOUND('',#2885,.T.);
#1888=FACE_OUTER_BOUND('',#2886,.T.);
#1889=FACE_OUTER_BOUND('',#2887,.T.);
#1890=FACE_OUTER_BOUND('',#2888,.T.);
#1891=FACE_OUTER_BOUND('',#2889,.T.);
#1892=FACE_OUTER_BOUND('',#2890,.T.);
#1893=FACE_OUTER_BOUND('',#2891,.T.);
#1894=FACE_OUTER_BOUND('',#2892,.T.);
#1895=FACE_OUTER_BOUND('',#2893,.T.);
#1896=FACE_OUTER_BOUND('',#2894,.T.);
#1897=FACE_OUTER_BOUND('',#2895,.T.);
#1898=FACE_OUTER_BOUND('',#2896,.T.);
#1899=FACE_OUTER_BOUND('',#2897,.T.);
#1900=FACE_OUTER_BOUND('',#2898,.T.);
#1901=FACE_OUTER_BOUND('',#2899,.T.);
#1902=FACE_OUTER_BOUND('',#2900,.T.);
#1903=FACE_OUTER_BOUND('',#2901,.T.);
#1904=FACE_OUTER_BOUND('',#2902,.T.);
#1905=FACE_OUTER_BOUND('',#2903,.T.);
#1906=FACE_OUTER_BOUND('',#2904,.T.);
#1907=FACE_OUTER_BOUND('',#2905,.T.);
#1908=FACE_OUTER_BOUND('',#2906,.T.);
#1909=FACE_OUTER_BOUND('',#2907,.T.);
#1910=FACE_OUTER_BOUND('',#2908,.T.);
#1911=FACE_OUTER_BOUND('',#2909,.T.);
#1912=FACE_OUTER_BOUND('',#2910,.T.);
#1913=FACE_OUTER_BOUND('',#2911,.T.);
#1914=FACE_OUTER_BOUND('',#2912,.T.);
#1915=FACE_OUTER_BOUND('',#2913,.T.);
#1916=FACE_OUTER_BOUND('',#2914,.T.);
#1917=FACE_OUTER_BOUND('',#2915,.T.);
#1918=FACE_OUTER_BOUND('',#2916,.T.);
#1919=FACE_OUTER_BOUND('',#2917,.T.);
#1920=FACE_OUTER_BOUND('',#2918,.T.);
#1921=FACE_OUTER_BOUND('',#2919,.T.);
#1922=FACE_OUTER_BOUND('',#2920,.T.);
#1923=FACE_OUTER_BOUND('',#2921,.T.);
#1924=FACE_OUTER_BOUND('',#2923,.T.);
#1925=FACE_OUTER_BOUND('',#2924,.T.);
#1926=FACE_OUTER_BOUND('',#2926,.T.);
#1927=FACE_OUTER_BOUND('',#2928,.T.);
#1928=FACE_OUTER_BOUND('',#2929,.T.);
#1929=FACE_OUTER_BOUND('',#2930,.T.);
#1930=FACE_OUTER_BOUND('',#2931,.T.);
#1931=FACE_OUTER_BOUND('',#2932,.T.);
#1932=FACE_OUTER_BOUND('',#2933,.T.);
#1933=FACE_OUTER_BOUND('',#2934,.T.);
#1934=FACE_OUTER_BOUND('',#2935,.T.);
#1935=FACE_OUTER_BOUND('',#2936,.T.);
#1936=FACE_OUTER_BOUND('',#2937,.T.);
#1937=FACE_OUTER_BOUND('',#2938,.T.);
#1938=FACE_OUTER_BOUND('',#2939,.T.);
#1939=FACE_OUTER_BOUND('',#2940,.T.);
#1940=FACE_OUTER_BOUND('',#2941,.T.);
#1941=FACE_OUTER_BOUND('',#2942,.T.);
#1942=FACE_OUTER_BOUND('',#2943,.T.);
#1943=FACE_OUTER_BOUND('',#2944,.T.);
#1944=FACE_OUTER_BOUND('',#2945,.T.);
#1945=FACE_OUTER_BOUND('',#2946,.T.);
#1946=FACE_OUTER_BOUND('',#2947,.T.);
#1947=FACE_OUTER_BOUND('',#2948,.T.);
#1948=FACE_OUTER_BOUND('',#2949,.T.);
#1949=FACE_OUTER_BOUND('',#2950,.T.);
#1950=FACE_OUTER_BOUND('',#2952,.T.);
#1951=FACE_OUTER_BOUND('',#2953,.T.);
#1952=FACE_OUTER_BOUND('',#2954,.T.);
#1953=FACE_OUTER_BOUND('',#2955,.T.);
#1954=FACE_OUTER_BOUND('',#2957,.T.);
#1955=FACE_OUTER_BOUND('',#2965,.T.);
#1956=FACE_OUTER_BOUND('',#2966,.T.);
#1957=FACE_OUTER_BOUND('',#2967,.T.);
#1958=FACE_OUTER_BOUND('',#2968,.T.);
#1959=FACE_OUTER_BOUND('',#2969,.T.);
#1960=FACE_OUTER_BOUND('',#2970,.T.);
#1961=FACE_OUTER_BOUND('',#2971,.T.);
#1962=FACE_OUTER_BOUND('',#2972,.T.);
#1963=FACE_OUTER_BOUND('',#2973,.T.);
#1964=FACE_OUTER_BOUND('',#2975,.T.);
#1965=FACE_OUTER_BOUND('',#2976,.T.);
#1966=FACE_OUTER_BOUND('',#2977,.T.);
#1967=FACE_OUTER_BOUND('',#2985,.T.);
#1968=FACE_OUTER_BOUND('',#2986,.T.);
#1969=FACE_OUTER_BOUND('',#2987,.T.);
#1970=FACE_OUTER_BOUND('',#2988,.T.);
#1971=FACE_OUTER_BOUND('',#2989,.T.);
#1972=FACE_OUTER_BOUND('',#2991,.T.);
#1973=FACE_OUTER_BOUND('',#2992,.T.);
#1974=FACE_OUTER_BOUND('',#2993,.T.);
#1975=FACE_OUTER_BOUND('',#3001,.T.);
#1976=FACE_OUTER_BOUND('',#3003,.T.);
#1977=FACE_OUTER_BOUND('',#3004,.T.);
#1978=FACE_OUTER_BOUND('',#3005,.T.);
#1979=FACE_OUTER_BOUND('',#3006,.T.);
#1980=FACE_OUTER_BOUND('',#3007,.T.);
#1981=FACE_OUTER_BOUND('',#3008,.T.);
#1982=FACE_OUTER_BOUND('',#3009,.T.);
#1983=FACE_OUTER_BOUND('',#3010,.T.);
#1984=FACE_OUTER_BOUND('',#3011,.T.);
#1985=FACE_OUTER_BOUND('',#3012,.T.);
#1986=FACE_OUTER_BOUND('',#3013,.T.);
#1987=FACE_OUTER_BOUND('',#3014,.T.);
#1988=FACE_OUTER_BOUND('',#3022,.T.);
#1989=FACE_OUTER_BOUND('',#3023,.T.);
#1990=FACE_OUTER_BOUND('',#3024,.T.);
#1991=FACE_OUTER_BOUND('',#3026,.T.);
#1992=FACE_OUTER_BOUND('',#3027,.T.);
#1993=FACE_OUTER_BOUND('',#3028,.T.);
#1994=FACE_OUTER_BOUND('',#3029,.T.);
#1995=FACE_OUTER_BOUND('',#3030,.T.);
#1996=FACE_OUTER_BOUND('',#3031,.T.);
#1997=FACE_OUTER_BOUND('',#3032,.T.);
#1998=FACE_OUTER_BOUND('',#3033,.T.);
#1999=FACE_OUTER_BOUND('',#3041,.T.);
#2000=FACE_OUTER_BOUND('',#3042,.T.);
#2001=FACE_OUTER_BOUND('',#3050,.T.);
#2002=FACE_OUTER_BOUND('',#3051,.T.);
#2003=FACE_OUTER_BOUND('',#3052,.T.);
#2004=FACE_OUTER_BOUND('',#3053,.T.);
#2005=FACE_OUTER_BOUND('',#3054,.T.);
#2006=FACE_OUTER_BOUND('',#3055,.T.);
#2007=FACE_OUTER_BOUND('',#3056,.T.);
#2008=FACE_OUTER_BOUND('',#3057,.T.);
#2009=FACE_OUTER_BOUND('',#3059,.T.);
#2010=FACE_OUTER_BOUND('',#3060,.T.);
#2011=FACE_OUTER_BOUND('',#3068,.T.);
#2012=FACE_OUTER_BOUND('',#3069,.T.);
#2013=FACE_OUTER_BOUND('',#3077,.T.);
#2014=FACE_OUTER_BOUND('',#3078,.T.);
#2015=FACE_OUTER_BOUND('',#3080,.T.);
#2016=FACE_OUTER_BOUND('',#3081,.T.);
#2017=FACE_OUTER_BOUND('',#3083,.T.);
#2018=FACE_OUTER_BOUND('',#3084,.T.);
#2019=FACE_OUTER_BOUND('',#3085,.T.);
#2020=FACE_OUTER_BOUND('',#3086,.T.);
#2021=FACE_OUTER_BOUND('',#3088,.T.);
#2022=FACE_OUTER_BOUND('',#3089,.T.);
#2023=FACE_OUTER_BOUND('',#3091,.T.);
#2024=FACE_OUTER_BOUND('',#3092,.T.);
#2025=FACE_OUTER_BOUND('',#3093,.T.);
#2026=FACE_OUTER_BOUND('',#3094,.T.);
#2027=FACE_OUTER_BOUND('',#3096,.T.);
#2028=FACE_OUTER_BOUND('',#3097,.T.);
#2029=FACE_OUTER_BOUND('',#3098,.T.);
#2030=FACE_OUTER_BOUND('',#3099,.T.);
#2031=FACE_OUTER_BOUND('',#3100,.T.);
#2032=FACE_OUTER_BOUND('',#3101,.T.);
#2033=FACE_OUTER_BOUND('',#3102,.T.);
#2034=FACE_OUTER_BOUND('',#3103,.T.);
#2035=FACE_OUTER_BOUND('',#3104,.T.);
#2036=FACE_OUTER_BOUND('',#3105,.T.);
#2037=FACE_OUTER_BOUND('',#3106,.T.);
#2038=FACE_OUTER_BOUND('',#3107,.T.);
#2039=FACE_OUTER_BOUND('',#3108,.T.);
#2040=FACE_OUTER_BOUND('',#3109,.T.);
#2041=FACE_OUTER_BOUND('',#3110,.T.);
#2042=FACE_OUTER_BOUND('',#3111,.T.);
#2043=FACE_OUTER_BOUND('',#3112,.T.);
#2044=FACE_OUTER_BOUND('',#3113,.T.);
#2045=FACE_OUTER_BOUND('',#3114,.T.);
#2046=FACE_OUTER_BOUND('',#3115,.T.);
#2047=FACE_OUTER_BOUND('',#3116,.T.);
#2048=FACE_OUTER_BOUND('',#3117,.T.);
#2049=FACE_OUTER_BOUND('',#3118,.T.);
#2050=FACE_OUTER_BOUND('',#3119,.T.);
#2051=FACE_OUTER_BOUND('',#3120,.T.);
#2052=FACE_OUTER_BOUND('',#3121,.T.);
#2053=FACE_OUTER_BOUND('',#3122,.T.);
#2054=FACE_OUTER_BOUND('',#3123,.T.);
#2055=FACE_OUTER_BOUND('',#3124,.T.);
#2056=FACE_OUTER_BOUND('',#3125,.T.);
#2057=FACE_OUTER_BOUND('',#3126,.T.);
#2058=FACE_OUTER_BOUND('',#3127,.T.);
#2059=FACE_OUTER_BOUND('',#3128,.T.);
#2060=FACE_OUTER_BOUND('',#3129,.T.);
#2061=FACE_OUTER_BOUND('',#3130,.T.);
#2062=FACE_OUTER_BOUND('',#3131,.T.);
#2063=FACE_OUTER_BOUND('',#3132,.T.);
#2064=FACE_OUTER_BOUND('',#3133,.T.);
#2065=FACE_OUTER_BOUND('',#3134,.T.);
#2066=FACE_OUTER_BOUND('',#3135,.T.);
#2067=FACE_OUTER_BOUND('',#3136,.T.);
#2068=FACE_OUTER_BOUND('',#3137,.T.);
#2069=FACE_OUTER_BOUND('',#3138,.T.);
#2070=FACE_OUTER_BOUND('',#3139,.T.);
#2071=FACE_OUTER_BOUND('',#3140,.T.);
#2072=FACE_OUTER_BOUND('',#3141,.T.);
#2073=FACE_OUTER_BOUND('',#3142,.T.);
#2074=FACE_OUTER_BOUND('',#3143,.T.);
#2075=FACE_OUTER_BOUND('',#3144,.T.);
#2076=FACE_OUTER_BOUND('',#3145,.T.);
#2077=FACE_OUTER_BOUND('',#3146,.T.);
#2078=FACE_OUTER_BOUND('',#3147,.T.);
#2079=FACE_OUTER_BOUND('',#3148,.T.);
#2080=FACE_OUTER_BOUND('',#3149,.T.);
#2081=FACE_OUTER_BOUND('',#3150,.T.);
#2082=FACE_OUTER_BOUND('',#3151,.T.);
#2083=FACE_OUTER_BOUND('',#3152,.T.);
#2084=FACE_OUTER_BOUND('',#3153,.T.);
#2085=FACE_OUTER_BOUND('',#3154,.T.);
#2086=FACE_OUTER_BOUND('',#3155,.T.);
#2087=FACE_OUTER_BOUND('',#3156,.T.);
#2088=FACE_OUTER_BOUND('',#3157,.T.);
#2089=FACE_OUTER_BOUND('',#3158,.T.);
#2090=FACE_OUTER_BOUND('',#3159,.T.);
#2091=FACE_OUTER_BOUND('',#3160,.T.);
#2092=FACE_OUTER_BOUND('',#3161,.T.);
#2093=FACE_OUTER_BOUND('',#3162,.T.);
#2094=FACE_OUTER_BOUND('',#3163,.T.);
#2095=FACE_OUTER_BOUND('',#3164,.T.);
#2096=FACE_OUTER_BOUND('',#3165,.T.);
#2097=FACE_OUTER_BOUND('',#3166,.T.);
#2098=FACE_OUTER_BOUND('',#3167,.T.);
#2099=FACE_OUTER_BOUND('',#3168,.T.);
#2100=FACE_OUTER_BOUND('',#3169,.T.);
#2101=FACE_OUTER_BOUND('',#3170,.T.);
#2102=FACE_OUTER_BOUND('',#3172,.T.);
#2103=FACE_OUTER_BOUND('',#3173,.T.);
#2104=FACE_OUTER_BOUND('',#3175,.T.);
#2105=FACE_OUTER_BOUND('',#3176,.T.);
#2106=FACE_OUTER_BOUND('',#3177,.T.);
#2107=FACE_OUTER_BOUND('',#3178,.T.);
#2108=FACE_OUTER_BOUND('',#3179,.T.);
#2109=FACE_OUTER_BOUND('',#3180,.T.);
#2110=FACE_OUTER_BOUND('',#3181,.T.);
#2111=FACE_OUTER_BOUND('',#3182,.T.);
#2112=FACE_OUTER_BOUND('',#3183,.T.);
#2113=FACE_OUTER_BOUND('',#3184,.T.);
#2114=FACE_OUTER_BOUND('',#3185,.T.);
#2115=FACE_OUTER_BOUND('',#3186,.T.);
#2116=FACE_OUTER_BOUND('',#3187,.T.);
#2117=FACE_OUTER_BOUND('',#3189,.T.);
#2118=FACE_OUTER_BOUND('',#3190,.T.);
#2119=FACE_OUTER_BOUND('',#3191,.T.);
#2120=FACE_OUTER_BOUND('',#3192,.T.);
#2121=FACE_OUTER_BOUND('',#3193,.T.);
#2122=FACE_OUTER_BOUND('',#3194,.T.);
#2123=FACE_OUTER_BOUND('',#3195,.T.);
#2124=FACE_OUTER_BOUND('',#3196,.T.);
#2125=FACE_OUTER_BOUND('',#3197,.T.);
#2126=FACE_OUTER_BOUND('',#3198,.T.);
#2127=FACE_OUTER_BOUND('',#3199,.T.);
#2128=FACE_OUTER_BOUND('',#3200,.T.);
#2129=FACE_OUTER_BOUND('',#3201,.T.);
#2130=FACE_OUTER_BOUND('',#3202,.T.);
#2131=FACE_OUTER_BOUND('',#3203,.T.);
#2132=FACE_OUTER_BOUND('',#3204,.T.);
#2133=FACE_OUTER_BOUND('',#3205,.T.);
#2134=FACE_OUTER_BOUND('',#3206,.T.);
#2135=FACE_OUTER_BOUND('',#3207,.T.);
#2136=FACE_OUTER_BOUND('',#3208,.T.);
#2137=FACE_OUTER_BOUND('',#3209,.T.);
#2138=FACE_OUTER_BOUND('',#3210,.T.);
#2139=FACE_OUTER_BOUND('',#3211,.T.);
#2140=FACE_OUTER_BOUND('',#3212,.T.);
#2141=FACE_OUTER_BOUND('',#3213,.T.);
#2142=FACE_OUTER_BOUND('',#3214,.T.);
#2143=FACE_OUTER_BOUND('',#3216,.T.);
#2144=FACE_OUTER_BOUND('',#3217,.T.);
#2145=FACE_OUTER_BOUND('',#3219,.T.);
#2146=FACE_OUTER_BOUND('',#3220,.T.);
#2147=FACE_OUTER_BOUND('',#3221,.T.);
#2148=FACE_OUTER_BOUND('',#3223,.T.);
#2149=FACE_OUTER_BOUND('',#3224,.T.);
#2150=FACE_OUTER_BOUND('',#3225,.T.);
#2151=FACE_OUTER_BOUND('',#3226,.T.);
#2152=FACE_OUTER_BOUND('',#3227,.T.);
#2153=FACE_OUTER_BOUND('',#3229,.T.);
#2154=FACE_OUTER_BOUND('',#3230,.T.);
#2155=FACE_OUTER_BOUND('',#3231,.T.);
#2156=FACE_OUTER_BOUND('',#3233,.T.);
#2157=FACE_OUTER_BOUND('',#3234,.T.);
#2158=FACE_OUTER_BOUND('',#3236,.T.);
#2159=FACE_OUTER_BOUND('',#3237,.T.);
#2160=FACE_OUTER_BOUND('',#3238,.T.);
#2161=FACE_OUTER_BOUND('',#3239,.T.);
#2162=FACE_OUTER_BOUND('',#3240,.T.);
#2163=FACE_OUTER_BOUND('',#3241,.T.);
#2164=FACE_OUTER_BOUND('',#3242,.T.);
#2165=FACE_OUTER_BOUND('',#3243,.T.);
#2166=FACE_OUTER_BOUND('',#3244,.T.);
#2167=FACE_OUTER_BOUND('',#3245,.T.);
#2168=FACE_OUTER_BOUND('',#3246,.T.);
#2169=FACE_OUTER_BOUND('',#3247,.T.);
#2170=FACE_OUTER_BOUND('',#3249,.T.);
#2171=FACE_OUTER_BOUND('',#3253,.T.);
#2172=FACE_OUTER_BOUND('',#3254,.T.);
#2173=FACE_OUTER_BOUND('',#3255,.T.);
#2174=FACE_OUTER_BOUND('',#3256,.T.);
#2175=FACE_OUTER_BOUND('',#3257,.T.);
#2176=FACE_OUTER_BOUND('',#3258,.T.);
#2177=FACE_OUTER_BOUND('',#3259,.T.);
#2178=FACE_OUTER_BOUND('',#3260,.T.);
#2179=FACE_OUTER_BOUND('',#3261,.T.);
#2180=FACE_OUTER_BOUND('',#3262,.T.);
#2181=FACE_OUTER_BOUND('',#3263,.T.);
#2182=FACE_OUTER_BOUND('',#3264,.T.);
#2183=FACE_OUTER_BOUND('',#3267,.T.);
#2184=FACE_OUTER_BOUND('',#3268,.T.);
#2185=FACE_OUTER_BOUND('',#3269,.T.);
#2186=FACE_OUTER_BOUND('',#3270,.T.);
#2187=FACE_OUTER_BOUND('',#3271,.T.);
#2188=FACE_OUTER_BOUND('',#3272,.T.);
#2189=FACE_OUTER_BOUND('',#3273,.T.);
#2190=FACE_OUTER_BOUND('',#3274,.T.);
#2191=FACE_OUTER_BOUND('',#3275,.T.);
#2192=FACE_OUTER_BOUND('',#3276,.T.);
#2193=FACE_OUTER_BOUND('',#3277,.T.);
#2194=FACE_OUTER_BOUND('',#3278,.T.);
#2195=FACE_OUTER_BOUND('',#3280,.T.);
#2196=FACE_OUTER_BOUND('',#3284,.T.);
#2197=FACE_OUTER_BOUND('',#3285,.T.);
#2198=FACE_OUTER_BOUND('',#3286,.T.);
#2199=FACE_OUTER_BOUND('',#3287,.T.);
#2200=FACE_OUTER_BOUND('',#3288,.T.);
#2201=FACE_OUTER_BOUND('',#3289,.T.);
#2202=FACE_OUTER_BOUND('',#3290,.T.);
#2203=FACE_OUTER_BOUND('',#3291,.T.);
#2204=FACE_OUTER_BOUND('',#3292,.T.);
#2205=FACE_OUTER_BOUND('',#3293,.T.);
#2206=FACE_OUTER_BOUND('',#3294,.T.);
#2207=FACE_OUTER_BOUND('',#3295,.T.);
#2208=FACE_OUTER_BOUND('',#3298,.T.);
#2209=FACE_OUTER_BOUND('',#3299,.T.);
#2210=FACE_OUTER_BOUND('',#3300,.T.);
#2211=FACE_OUTER_BOUND('',#3301,.T.);
#2212=FACE_OUTER_BOUND('',#3302,.T.);
#2213=FACE_OUTER_BOUND('',#3303,.T.);
#2214=FACE_OUTER_BOUND('',#3304,.T.);
#2215=FACE_OUTER_BOUND('',#3305,.T.);
#2216=FACE_OUTER_BOUND('',#3306,.T.);
#2217=FACE_OUTER_BOUND('',#3307,.T.);
#2218=FACE_OUTER_BOUND('',#3308,.T.);
#2219=FACE_OUTER_BOUND('',#3309,.T.);
#2220=FACE_OUTER_BOUND('',#3311,.T.);
#2221=FACE_OUTER_BOUND('',#3313,.T.);
#2222=FACE_OUTER_BOUND('',#3314,.T.);
#2223=FACE_OUTER_BOUND('',#3316,.T.);
#2224=FACE_OUTER_BOUND('',#3317,.T.);
#2225=FACE_OUTER_BOUND('',#3318,.T.);
#2226=FACE_OUTER_BOUND('',#3319,.T.);
#2227=FACE_OUTER_BOUND('',#3320,.T.);
#2228=FACE_OUTER_BOUND('',#3321,.T.);
#2229=FACE_OUTER_BOUND('',#3322,.T.);
#2230=FACE_OUTER_BOUND('',#3323,.T.);
#2231=FACE_OUTER_BOUND('',#3324,.T.);
#2232=FACE_OUTER_BOUND('',#3325,.T.);
#2233=FACE_OUTER_BOUND('',#3326,.T.);
#2234=FACE_OUTER_BOUND('',#3327,.T.);
#2235=FACE_OUTER_BOUND('',#3328,.T.);
#2236=FACE_OUTER_BOUND('',#3329,.T.);
#2237=FACE_OUTER_BOUND('',#3330,.T.);
#2238=FACE_OUTER_BOUND('',#3331,.T.);
#2239=FACE_OUTER_BOUND('',#3332,.T.);
#2240=FACE_OUTER_BOUND('',#3334,.T.);
#2241=FACE_OUTER_BOUND('',#3335,.T.);
#2242=FACE_OUTER_BOUND('',#3336,.T.);
#2243=FACE_OUTER_BOUND('',#3337,.T.);
#2244=FACE_OUTER_BOUND('',#3339,.T.);
#2245=FACE_OUTER_BOUND('',#3340,.T.);
#2246=FACE_OUTER_BOUND('',#3341,.T.);
#2247=FACE_OUTER_BOUND('',#3342,.T.);
#2248=FACE_OUTER_BOUND('',#3343,.T.);
#2249=FACE_OUTER_BOUND('',#3344,.T.);
#2250=FACE_OUTER_BOUND('',#3345,.T.);
#2251=FACE_OUTER_BOUND('',#3346,.T.);
#2252=FACE_OUTER_BOUND('',#3347,.T.);
#2253=FACE_OUTER_BOUND('',#3348,.T.);
#2254=FACE_OUTER_BOUND('',#3349,.T.);
#2255=FACE_OUTER_BOUND('',#3350,.T.);
#2256=FACE_OUTER_BOUND('',#3351,.T.);
#2257=FACE_OUTER_BOUND('',#3352,.T.);
#2258=FACE_OUTER_BOUND('',#3353,.T.);
#2259=FACE_OUTER_BOUND('',#3354,.T.);
#2260=FACE_OUTER_BOUND('',#3355,.T.);
#2261=FACE_OUTER_BOUND('',#3356,.T.);
#2262=FACE_OUTER_BOUND('',#3357,.T.);
#2263=FACE_OUTER_BOUND('',#3358,.T.);
#2264=FACE_OUTER_BOUND('',#3359,.T.);
#2265=FACE_OUTER_BOUND('',#3361,.T.);
#2266=FACE_OUTER_BOUND('',#3362,.T.);
#2267=FACE_OUTER_BOUND('',#3363,.T.);
#2268=FACE_OUTER_BOUND('',#3364,.T.);
#2269=FACE_OUTER_BOUND('',#3365,.T.);
#2270=FACE_OUTER_BOUND('',#3366,.T.);
#2271=FACE_OUTER_BOUND('',#3367,.T.);
#2272=FACE_OUTER_BOUND('',#3368,.T.);
#2273=FACE_OUTER_BOUND('',#3369,.T.);
#2274=FACE_OUTER_BOUND('',#3370,.T.);
#2275=FACE_OUTER_BOUND('',#3371,.T.);
#2276=FACE_OUTER_BOUND('',#3372,.T.);
#2277=FACE_OUTER_BOUND('',#3373,.T.);
#2278=FACE_OUTER_BOUND('',#3374,.T.);
#2279=FACE_OUTER_BOUND('',#3375,.T.);
#2280=FACE_OUTER_BOUND('',#3376,.T.);
#2281=FACE_OUTER_BOUND('',#3377,.T.);
#2282=FACE_OUTER_BOUND('',#3378,.T.);
#2283=FACE_OUTER_BOUND('',#3379,.T.);
#2284=FACE_OUTER_BOUND('',#3380,.T.);
#2285=FACE_OUTER_BOUND('',#3381,.T.);
#2286=FACE_OUTER_BOUND('',#3382,.T.);
#2287=FACE_OUTER_BOUND('',#3384,.T.);
#2288=FACE_OUTER_BOUND('',#3385,.T.);
#2289=FACE_OUTER_BOUND('',#3386,.T.);
#2290=FACE_OUTER_BOUND('',#3387,.T.);
#2291=FACE_OUTER_BOUND('',#3388,.T.);
#2292=FACE_OUTER_BOUND('',#3389,.T.);
#2293=FACE_OUTER_BOUND('',#3391,.T.);
#2294=FACE_OUTER_BOUND('',#3392,.T.);
#2295=FACE_OUTER_BOUND('',#3393,.T.);
#2296=FACE_OUTER_BOUND('',#3394,.T.);
#2297=FACE_OUTER_BOUND('',#3395,.T.);
#2298=FACE_OUTER_BOUND('',#3396,.T.);
#2299=FACE_OUTER_BOUND('',#3397,.T.);
#2300=FACE_OUTER_BOUND('',#3398,.T.);
#2301=FACE_OUTER_BOUND('',#3399,.T.);
#2302=FACE_OUTER_BOUND('',#3400,.T.);
#2303=FACE_OUTER_BOUND('',#3401,.T.);
#2304=FACE_OUTER_BOUND('',#3402,.T.);
#2305=FACE_OUTER_BOUND('',#3403,.T.);
#2306=FACE_OUTER_BOUND('',#3404,.T.);
#2307=FACE_OUTER_BOUND('',#3405,.T.);
#2308=FACE_OUTER_BOUND('',#3406,.T.);
#2309=FACE_OUTER_BOUND('',#3407,.T.);
#2310=FACE_OUTER_BOUND('',#3408,.T.);
#2311=FACE_OUTER_BOUND('',#3409,.T.);
#2312=FACE_OUTER_BOUND('',#3410,.T.);
#2313=FACE_OUTER_BOUND('',#3411,.T.);
#2314=FACE_OUTER_BOUND('',#3412,.T.);
#2315=FACE_OUTER_BOUND('',#3413,.T.);
#2316=FACE_OUTER_BOUND('',#3414,.T.);
#2317=FACE_OUTER_BOUND('',#3415,.T.);
#2318=FACE_OUTER_BOUND('',#3416,.T.);
#2319=FACE_OUTER_BOUND('',#3417,.T.);
#2320=FACE_OUTER_BOUND('',#3418,.T.);
#2321=FACE_OUTER_BOUND('',#3419,.T.);
#2322=FACE_OUTER_BOUND('',#3420,.T.);
#2323=FACE_OUTER_BOUND('',#3421,.T.);
#2324=FACE_OUTER_BOUND('',#3423,.T.);
#2325=FACE_OUTER_BOUND('',#3424,.T.);
#2326=FACE_OUTER_BOUND('',#3425,.T.);
#2327=FACE_OUTER_BOUND('',#3426,.T.);
#2328=FACE_OUTER_BOUND('',#3427,.T.);
#2329=FACE_OUTER_BOUND('',#3428,.T.);
#2330=FACE_OUTER_BOUND('',#3429,.T.);
#2331=FACE_OUTER_BOUND('',#3430,.T.);
#2332=FACE_OUTER_BOUND('',#3432,.T.);
#2333=FACE_OUTER_BOUND('',#3434,.T.);
#2334=FACE_OUTER_BOUND('',#3436,.T.);
#2335=FACE_OUTER_BOUND('',#3437,.T.);
#2336=FACE_OUTER_BOUND('',#3438,.T.);
#2337=FACE_OUTER_BOUND('',#3440,.T.);
#2338=FACE_OUTER_BOUND('',#3442,.T.);
#2339=FACE_OUTER_BOUND('',#3443,.T.);
#2340=FACE_OUTER_BOUND('',#3444,.T.);
#2341=FACE_OUTER_BOUND('',#3445,.T.);
#2342=FACE_OUTER_BOUND('',#3446,.T.);
#2343=FACE_OUTER_BOUND('',#3447,.T.);
#2344=FACE_OUTER_BOUND('',#3448,.T.);
#2345=FACE_OUTER_BOUND('',#3449,.T.);
#2346=FACE_OUTER_BOUND('',#3450,.T.);
#2347=FACE_OUTER_BOUND('',#3451,.T.);
#2348=FACE_OUTER_BOUND('',#3453,.T.);
#2349=FACE_OUTER_BOUND('',#3454,.T.);
#2350=FACE_OUTER_BOUND('',#3455,.T.);
#2351=FACE_OUTER_BOUND('',#3456,.T.);
#2352=FACE_OUTER_BOUND('',#3458,.T.);
#2353=FACE_OUTER_BOUND('',#3459,.T.);
#2354=FACE_OUTER_BOUND('',#3466,.T.);
#2355=FACE_OUTER_BOUND('',#3467,.T.);
#2356=FACE_OUTER_BOUND('',#3468,.T.);
#2357=FACE_OUTER_BOUND('',#3469,.T.);
#2358=FACE_OUTER_BOUND('',#3470,.T.);
#2359=FACE_OUTER_BOUND('',#3471,.T.);
#2360=FACE_OUTER_BOUND('',#3472,.T.);
#2361=FACE_OUTER_BOUND('',#3473,.T.);
#2362=FACE_OUTER_BOUND('',#3474,.T.);
#2363=FACE_OUTER_BOUND('',#3475,.T.);
#2364=FACE_OUTER_BOUND('',#3476,.T.);
#2365=FACE_OUTER_BOUND('',#3477,.T.);
#2366=FACE_OUTER_BOUND('',#3478,.T.);
#2367=FACE_OUTER_BOUND('',#3479,.T.);
#2368=FACE_OUTER_BOUND('',#3480,.T.);
#2369=FACE_OUTER_BOUND('',#3481,.T.);
#2370=FACE_OUTER_BOUND('',#3482,.T.);
#2371=FACE_OUTER_BOUND('',#3483,.T.);
#2372=FACE_OUTER_BOUND('',#3484,.T.);
#2373=FACE_OUTER_BOUND('',#3485,.T.);
#2374=FACE_OUTER_BOUND('',#3486,.T.);
#2375=FACE_OUTER_BOUND('',#3487,.T.);
#2376=FACE_OUTER_BOUND('',#3488,.T.);
#2377=FACE_OUTER_BOUND('',#3489,.T.);
#2378=FACE_OUTER_BOUND('',#3490,.T.);
#2379=FACE_OUTER_BOUND('',#3491,.T.);
#2380=FACE_OUTER_BOUND('',#3492,.T.);
#2381=FACE_OUTER_BOUND('',#3499,.T.);
#2382=FACE_OUTER_BOUND('',#3500,.T.);
#2383=FACE_OUTER_BOUND('',#3501,.T.);
#2384=FACE_OUTER_BOUND('',#3502,.T.);
#2385=FACE_OUTER_BOUND('',#3503,.T.);
#2386=FACE_OUTER_BOUND('',#3504,.T.);
#2387=FACE_OUTER_BOUND('',#3505,.T.);
#2388=FACE_OUTER_BOUND('',#3506,.T.);
#2389=FACE_OUTER_BOUND('',#3507,.T.);
#2390=FACE_OUTER_BOUND('',#3508,.T.);
#2391=FACE_OUTER_BOUND('',#3509,.T.);
#2392=FACE_OUTER_BOUND('',#3510,.T.);
#2393=FACE_OUTER_BOUND('',#3511,.T.);
#2394=FACE_OUTER_BOUND('',#3512,.T.);
#2395=FACE_OUTER_BOUND('',#3513,.T.);
#2396=FACE_OUTER_BOUND('',#3514,.T.);
#2397=FACE_OUTER_BOUND('',#3515,.T.);
#2398=FACE_OUTER_BOUND('',#3516,.T.);
#2399=FACE_OUTER_BOUND('',#3517,.T.);
#2400=FACE_OUTER_BOUND('',#3518,.T.);
#2401=FACE_OUTER_BOUND('',#3519,.T.);
#2402=FACE_OUTER_BOUND('',#3520,.T.);
#2403=FACE_OUTER_BOUND('',#3521,.T.);
#2404=FACE_OUTER_BOUND('',#3522,.T.);
#2405=FACE_OUTER_BOUND('',#3523,.T.);
#2406=FACE_OUTER_BOUND('',#3524,.T.);
#2407=FACE_OUTER_BOUND('',#3525,.T.);
#2408=FACE_OUTER_BOUND('',#3526,.T.);
#2409=FACE_OUTER_BOUND('',#3527,.T.);
#2410=FACE_OUTER_BOUND('',#3528,.T.);
#2411=FACE_OUTER_BOUND('',#3529,.T.);
#2412=FACE_OUTER_BOUND('',#3530,.T.);
#2413=FACE_OUTER_BOUND('',#3531,.T.);
#2414=FACE_OUTER_BOUND('',#3532,.T.);
#2415=FACE_OUTER_BOUND('',#3533,.T.);
#2416=FACE_OUTER_BOUND('',#3534,.T.);
#2417=FACE_OUTER_BOUND('',#3535,.T.);
#2418=FACE_OUTER_BOUND('',#3536,.T.);
#2419=FACE_OUTER_BOUND('',#3537,.T.);
#2420=FACE_OUTER_BOUND('',#3538,.T.);
#2421=FACE_OUTER_BOUND('',#3539,.T.);
#2422=FACE_OUTER_BOUND('',#3540,.T.);
#2423=FACE_OUTER_BOUND('',#3541,.T.);
#2424=FACE_OUTER_BOUND('',#3542,.T.);
#2425=FACE_OUTER_BOUND('',#3543,.T.);
#2426=FACE_OUTER_BOUND('',#3544,.T.);
#2427=FACE_OUTER_BOUND('',#3545,.T.);
#2428=FACE_OUTER_BOUND('',#3546,.T.);
#2429=FACE_OUTER_BOUND('',#3547,.T.);
#2430=FACE_OUTER_BOUND('',#3548,.T.);
#2431=FACE_OUTER_BOUND('',#3549,.T.);
#2432=FACE_OUTER_BOUND('',#3550,.T.);
#2433=FACE_OUTER_BOUND('',#3551,.T.);
#2434=FACE_OUTER_BOUND('',#3552,.T.);
#2435=FACE_OUTER_BOUND('',#3553,.T.);
#2436=FACE_OUTER_BOUND('',#3554,.T.);
#2437=FACE_OUTER_BOUND('',#3555,.T.);
#2438=FACE_OUTER_BOUND('',#3556,.T.);
#2439=FACE_OUTER_BOUND('',#3557,.T.);
#2440=FACE_OUTER_BOUND('',#3558,.T.);
#2441=FACE_OUTER_BOUND('',#3559,.T.);
#2442=FACE_OUTER_BOUND('',#3560,.T.);
#2443=FACE_OUTER_BOUND('',#3562,.T.);
#2444=FACE_OUTER_BOUND('',#3563,.T.);
#2445=FACE_OUTER_BOUND('',#3564,.T.);
#2446=FACE_OUTER_BOUND('',#3565,.T.);
#2447=FACE_OUTER_BOUND('',#3566,.T.);
#2448=FACE_OUTER_BOUND('',#3567,.T.);
#2449=FACE_OUTER_BOUND('',#3568,.T.);
#2450=FACE_OUTER_BOUND('',#3569,.T.);
#2451=FACE_OUTER_BOUND('',#3570,.T.);
#2452=FACE_OUTER_BOUND('',#3571,.T.);
#2453=FACE_OUTER_BOUND('',#3572,.T.);
#2454=FACE_OUTER_BOUND('',#3573,.T.);
#2455=FACE_OUTER_BOUND('',#3574,.T.);
#2456=FACE_OUTER_BOUND('',#3575,.T.);
#2457=FACE_OUTER_BOUND('',#3576,.T.);
#2458=FACE_OUTER_BOUND('',#3577,.T.);
#2459=FACE_OUTER_BOUND('',#3578,.T.);
#2460=FACE_OUTER_BOUND('',#3579,.T.);
#2461=FACE_OUTER_BOUND('',#3580,.T.);
#2462=FACE_OUTER_BOUND('',#3581,.T.);
#2463=FACE_OUTER_BOUND('',#3582,.T.);
#2464=FACE_OUTER_BOUND('',#3583,.T.);
#2465=FACE_OUTER_BOUND('',#3584,.T.);
#2466=FACE_OUTER_BOUND('',#3585,.T.);
#2467=FACE_OUTER_BOUND('',#3586,.T.);
#2468=FACE_OUTER_BOUND('',#3587,.T.);
#2469=FACE_OUTER_BOUND('',#3588,.T.);
#2470=FACE_OUTER_BOUND('',#3589,.T.);
#2471=FACE_OUTER_BOUND('',#3590,.T.);
#2472=FACE_OUTER_BOUND('',#3591,.T.);
#2473=FACE_OUTER_BOUND('',#3592,.T.);
#2474=FACE_OUTER_BOUND('',#3593,.T.);
#2475=FACE_OUTER_BOUND('',#3594,.T.);
#2476=FACE_OUTER_BOUND('',#3595,.T.);
#2477=FACE_OUTER_BOUND('',#3596,.T.);
#2478=FACE_OUTER_BOUND('',#3597,.T.);
#2479=FACE_OUTER_BOUND('',#3598,.T.);
#2480=FACE_OUTER_BOUND('',#3599,.T.);
#2481=FACE_OUTER_BOUND('',#3600,.T.);
#2482=FACE_OUTER_BOUND('',#3601,.T.);
#2483=FACE_OUTER_BOUND('',#3602,.T.);
#2484=FACE_OUTER_BOUND('',#3603,.T.);
#2485=FACE_OUTER_BOUND('',#3604,.T.);
#2486=FACE_OUTER_BOUND('',#3605,.T.);
#2487=FACE_OUTER_BOUND('',#3606,.T.);
#2488=FACE_OUTER_BOUND('',#3607,.T.);
#2489=FACE_OUTER_BOUND('',#3608,.T.);
#2490=FACE_OUTER_BOUND('',#3609,.T.);
#2491=FACE_OUTER_BOUND('',#3610,.T.);
#2492=FACE_OUTER_BOUND('',#3611,.T.);
#2493=FACE_OUTER_BOUND('',#3612,.T.);
#2494=FACE_OUTER_BOUND('',#3613,.T.);
#2495=FACE_OUTER_BOUND('',#3614,.T.);
#2496=FACE_OUTER_BOUND('',#3615,.T.);
#2497=FACE_OUTER_BOUND('',#3616,.T.);
#2498=FACE_OUTER_BOUND('',#3617,.T.);
#2499=FACE_OUTER_BOUND('',#3618,.T.);
#2500=FACE_OUTER_BOUND('',#3619,.T.);
#2501=FACE_OUTER_BOUND('',#3620,.T.);
#2502=FACE_OUTER_BOUND('',#3621,.T.);
#2503=FACE_OUTER_BOUND('',#3622,.T.);
#2504=FACE_OUTER_BOUND('',#3623,.T.);
#2505=FACE_OUTER_BOUND('',#3624,.T.);
#2506=FACE_OUTER_BOUND('',#3625,.T.);
#2507=FACE_OUTER_BOUND('',#3626,.T.);
#2508=FACE_OUTER_BOUND('',#3627,.T.);
#2509=FACE_OUTER_BOUND('',#3628,.T.);
#2510=FACE_OUTER_BOUND('',#3629,.T.);
#2511=FACE_OUTER_BOUND('',#3630,.T.);
#2512=FACE_OUTER_BOUND('',#3631,.T.);
#2513=FACE_OUTER_BOUND('',#3632,.T.);
#2514=FACE_OUTER_BOUND('',#3633,.T.);
#2515=FACE_OUTER_BOUND('',#3634,.T.);
#2516=FACE_OUTER_BOUND('',#3635,.T.);
#2517=FACE_OUTER_BOUND('',#3636,.T.);
#2518=FACE_OUTER_BOUND('',#3637,.T.);
#2519=FACE_OUTER_BOUND('',#3638,.T.);
#2520=FACE_OUTER_BOUND('',#3639,.T.);
#2521=FACE_OUTER_BOUND('',#3640,.T.);
#2522=FACE_OUTER_BOUND('',#3641,.T.);
#2523=FACE_OUTER_BOUND('',#3642,.T.);
#2524=FACE_OUTER_BOUND('',#3643,.T.);
#2525=FACE_OUTER_BOUND('',#3644,.T.);
#2526=FACE_OUTER_BOUND('',#3645,.T.);
#2527=FACE_OUTER_BOUND('',#3646,.T.);
#2528=FACE_OUTER_BOUND('',#3647,.T.);
#2529=FACE_OUTER_BOUND('',#3648,.T.);
#2530=FACE_OUTER_BOUND('',#3649,.T.);
#2531=FACE_OUTER_BOUND('',#3650,.T.);
#2532=FACE_OUTER_BOUND('',#3651,.T.);
#2533=FACE_OUTER_BOUND('',#3652,.T.);
#2534=FACE_OUTER_BOUND('',#3653,.T.);
#2535=FACE_OUTER_BOUND('',#3654,.T.);
#2536=FACE_OUTER_BOUND('',#3655,.T.);
#2537=FACE_OUTER_BOUND('',#3656,.T.);
#2538=FACE_OUTER_BOUND('',#3657,.T.);
#2539=FACE_OUTER_BOUND('',#3658,.T.);
#2540=FACE_OUTER_BOUND('',#3659,.T.);
#2541=FACE_OUTER_BOUND('',#3660,.T.);
#2542=FACE_OUTER_BOUND('',#3662,.T.);
#2543=FACE_OUTER_BOUND('',#3663,.T.);
#2544=FACE_OUTER_BOUND('',#3664,.T.);
#2545=FACE_OUTER_BOUND('',#3665,.T.);
#2546=FACE_OUTER_BOUND('',#3666,.T.);
#2547=FACE_OUTER_BOUND('',#3667,.T.);
#2548=FACE_OUTER_BOUND('',#3668,.T.);
#2549=FACE_OUTER_BOUND('',#3669,.T.);
#2550=FACE_OUTER_BOUND('',#3670,.T.);
#2551=FACE_OUTER_BOUND('',#3671,.T.);
#2552=FACE_OUTER_BOUND('',#3672,.T.);
#2553=FACE_OUTER_BOUND('',#3673,.T.);
#2554=FACE_OUTER_BOUND('',#3674,.T.);
#2555=FACE_OUTER_BOUND('',#3675,.T.);
#2556=FACE_OUTER_BOUND('',#3676,.T.);
#2557=FACE_OUTER_BOUND('',#3677,.T.);
#2558=FACE_OUTER_BOUND('',#3678,.T.);
#2559=FACE_OUTER_BOUND('',#3679,.T.);
#2560=FACE_OUTER_BOUND('',#3680,.T.);
#2561=FACE_OUTER_BOUND('',#3681,.T.);
#2562=FACE_OUTER_BOUND('',#3682,.T.);
#2563=FACE_OUTER_BOUND('',#3683,.T.);
#2564=FACE_OUTER_BOUND('',#3684,.T.);
#2565=FACE_OUTER_BOUND('',#3685,.T.);
#2566=FACE_OUTER_BOUND('',#3686,.T.);
#2567=FACE_OUTER_BOUND('',#3687,.T.);
#2568=FACE_OUTER_BOUND('',#3688,.T.);
#2569=FACE_OUTER_BOUND('',#3689,.T.);
#2570=FACE_OUTER_BOUND('',#3690,.T.);
#2571=FACE_OUTER_BOUND('',#3691,.T.);
#2572=FACE_OUTER_BOUND('',#3692,.T.);
#2573=FACE_OUTER_BOUND('',#3693,.T.);
#2574=FACE_OUTER_BOUND('',#3694,.T.);
#2575=FACE_OUTER_BOUND('',#3695,.T.);
#2576=FACE_OUTER_BOUND('',#3696,.T.);
#2577=FACE_OUTER_BOUND('',#3697,.T.);
#2578=FACE_OUTER_BOUND('',#3698,.T.);
#2579=FACE_OUTER_BOUND('',#3699,.T.);
#2580=FACE_OUTER_BOUND('',#3700,.T.);
#2581=FACE_OUTER_BOUND('',#3701,.T.);
#2582=FACE_OUTER_BOUND('',#3702,.T.);
#2583=FACE_OUTER_BOUND('',#3703,.T.);
#2584=FACE_OUTER_BOUND('',#3704,.T.);
#2585=FACE_OUTER_BOUND('',#3705,.T.);
#2586=FACE_OUTER_BOUND('',#3706,.T.);
#2587=FACE_OUTER_BOUND('',#3707,.T.);
#2588=FACE_OUTER_BOUND('',#3708,.T.);
#2589=FACE_OUTER_BOUND('',#3709,.T.);
#2590=FACE_OUTER_BOUND('',#3710,.T.);
#2591=FACE_OUTER_BOUND('',#3711,.T.);
#2592=FACE_OUTER_BOUND('',#3712,.T.);
#2593=FACE_OUTER_BOUND('',#3713,.T.);
#2594=FACE_OUTER_BOUND('',#3714,.T.);
#2595=FACE_OUTER_BOUND('',#3715,.T.);
#2596=FACE_OUTER_BOUND('',#3716,.T.);
#2597=FACE_OUTER_BOUND('',#3717,.T.);
#2598=FACE_OUTER_BOUND('',#3718,.T.);
#2599=FACE_OUTER_BOUND('',#3719,.T.);
#2600=FACE_OUTER_BOUND('',#3720,.T.);
#2601=FACE_OUTER_BOUND('',#3721,.T.);
#2602=FACE_OUTER_BOUND('',#3722,.T.);
#2603=FACE_OUTER_BOUND('',#3723,.T.);
#2604=FACE_OUTER_BOUND('',#3724,.T.);
#2605=FACE_OUTER_BOUND('',#3725,.T.);
#2606=FACE_OUTER_BOUND('',#3726,.T.);
#2607=FACE_OUTER_BOUND('',#3727,.T.);
#2608=FACE_OUTER_BOUND('',#3728,.T.);
#2609=FACE_OUTER_BOUND('',#3729,.T.);
#2610=FACE_OUTER_BOUND('',#3730,.T.);
#2611=FACE_OUTER_BOUND('',#3731,.T.);
#2612=FACE_OUTER_BOUND('',#3732,.T.);
#2613=FACE_OUTER_BOUND('',#3733,.T.);
#2614=FACE_OUTER_BOUND('',#3734,.T.);
#2615=FACE_OUTER_BOUND('',#3735,.T.);
#2616=FACE_OUTER_BOUND('',#3736,.T.);
#2617=FACE_OUTER_BOUND('',#3737,.T.);
#2618=FACE_OUTER_BOUND('',#3738,.T.);
#2619=FACE_OUTER_BOUND('',#3739,.T.);
#2620=FACE_OUTER_BOUND('',#3740,.T.);
#2621=FACE_OUTER_BOUND('',#3741,.T.);
#2622=FACE_OUTER_BOUND('',#3742,.T.);
#2623=FACE_OUTER_BOUND('',#3743,.T.);
#2624=FACE_OUTER_BOUND('',#3744,.T.);
#2625=FACE_OUTER_BOUND('',#3745,.T.);
#2626=FACE_OUTER_BOUND('',#3746,.T.);
#2627=FACE_OUTER_BOUND('',#3747,.T.);
#2628=FACE_OUTER_BOUND('',#3748,.T.);
#2629=FACE_OUTER_BOUND('',#3749,.T.);
#2630=FACE_OUTER_BOUND('',#3750,.T.);
#2631=FACE_OUTER_BOUND('',#3751,.T.);
#2632=FACE_OUTER_BOUND('',#3752,.T.);
#2633=FACE_OUTER_BOUND('',#3753,.T.);
#2634=FACE_OUTER_BOUND('',#3754,.T.);
#2635=FACE_OUTER_BOUND('',#3755,.T.);
#2636=FACE_OUTER_BOUND('',#3756,.T.);
#2637=FACE_OUTER_BOUND('',#3757,.T.);
#2638=FACE_OUTER_BOUND('',#3758,.T.);
#2639=FACE_OUTER_BOUND('',#3759,.T.);
#2640=FACE_OUTER_BOUND('',#3760,.T.);
#2641=FACE_OUTER_BOUND('',#3761,.T.);
#2642=FACE_OUTER_BOUND('',#3762,.T.);
#2643=FACE_OUTER_BOUND('',#3763,.T.);
#2644=FACE_OUTER_BOUND('',#3764,.T.);
#2645=FACE_OUTER_BOUND('',#3765,.T.);
#2646=FACE_OUTER_BOUND('',#3766,.T.);
#2647=FACE_OUTER_BOUND('',#3767,.T.);
#2648=FACE_OUTER_BOUND('',#3768,.T.);
#2649=FACE_OUTER_BOUND('',#3769,.T.);
#2650=FACE_OUTER_BOUND('',#3770,.T.);
#2651=FACE_OUTER_BOUND('',#3771,.T.);
#2652=FACE_OUTER_BOUND('',#3772,.T.);
#2653=FACE_OUTER_BOUND('',#3773,.T.);
#2654=FACE_OUTER_BOUND('',#3774,.T.);
#2655=FACE_OUTER_BOUND('',#3775,.T.);
#2656=FACE_OUTER_BOUND('',#3776,.T.);
#2657=FACE_OUTER_BOUND('',#3777,.T.);
#2658=FACE_OUTER_BOUND('',#3778,.T.);
#2659=FACE_OUTER_BOUND('',#3779,.T.);
#2660=FACE_OUTER_BOUND('',#3780,.T.);
#2661=FACE_OUTER_BOUND('',#3781,.T.);
#2662=FACE_OUTER_BOUND('',#3782,.T.);
#2663=FACE_OUTER_BOUND('',#3783,.T.);
#2664=FACE_OUTER_BOUND('',#3784,.T.);
#2665=FACE_OUTER_BOUND('',#3785,.T.);
#2666=FACE_OUTER_BOUND('',#3786,.T.);
#2667=FACE_OUTER_BOUND('',#3787,.T.);
#2668=FACE_OUTER_BOUND('',#3788,.T.);
#2669=FACE_OUTER_BOUND('',#3789,.T.);
#2670=FACE_OUTER_BOUND('',#3790,.T.);
#2671=FACE_OUTER_BOUND('',#3791,.T.);
#2672=FACE_OUTER_BOUND('',#3792,.T.);
#2673=FACE_OUTER_BOUND('',#3793,.T.);
#2674=FACE_OUTER_BOUND('',#3794,.T.);
#2675=FACE_OUTER_BOUND('',#3795,.T.);
#2676=FACE_OUTER_BOUND('',#3796,.T.);
#2677=FACE_OUTER_BOUND('',#3797,.T.);
#2678=FACE_OUTER_BOUND('',#3798,.T.);
#2679=FACE_OUTER_BOUND('',#3799,.T.);
#2680=FACE_OUTER_BOUND('',#3800,.T.);
#2681=FACE_OUTER_BOUND('',#3801,.T.);
#2682=FACE_OUTER_BOUND('',#3802,.T.);
#2683=FACE_OUTER_BOUND('',#3803,.T.);
#2684=FACE_OUTER_BOUND('',#3804,.T.);
#2685=FACE_OUTER_BOUND('',#3805,.T.);
#2686=FACE_OUTER_BOUND('',#3806,.T.);
#2687=FACE_OUTER_BOUND('',#3807,.T.);
#2688=FACE_OUTER_BOUND('',#3808,.T.);
#2689=FACE_OUTER_BOUND('',#3809,.T.);
#2690=FACE_OUTER_BOUND('',#3810,.T.);
#2691=FACE_OUTER_BOUND('',#3811,.T.);
#2692=FACE_OUTER_BOUND('',#3812,.T.);
#2693=FACE_OUTER_BOUND('',#3813,.T.);
#2694=FACE_OUTER_BOUND('',#3814,.T.);
#2695=FACE_OUTER_BOUND('',#3815,.T.);
#2696=FACE_OUTER_BOUND('',#3816,.T.);
#2697=FACE_OUTER_BOUND('',#3817,.T.);
#2698=FACE_OUTER_BOUND('',#3818,.T.);
#2699=FACE_OUTER_BOUND('',#3819,.T.);
#2700=FACE_OUTER_BOUND('',#3820,.T.);
#2701=FACE_OUTER_BOUND('',#3821,.T.);
#2702=FACE_OUTER_BOUND('',#3822,.T.);
#2703=FACE_OUTER_BOUND('',#3823,.T.);
#2704=FACE_OUTER_BOUND('',#3824,.T.);
#2705=FACE_OUTER_BOUND('',#3825,.T.);
#2706=FACE_OUTER_BOUND('',#3826,.T.);
#2707=FACE_OUTER_BOUND('',#3827,.T.);
#2708=FACE_OUTER_BOUND('',#3828,.T.);
#2709=FACE_OUTER_BOUND('',#3829,.T.);
#2710=FACE_OUTER_BOUND('',#3830,.T.);
#2711=FACE_OUTER_BOUND('',#3831,.T.);
#2712=FACE_OUTER_BOUND('',#3832,.T.);
#2713=FACE_OUTER_BOUND('',#3833,.T.);
#2714=FACE_OUTER_BOUND('',#3834,.T.);
#2715=FACE_OUTER_BOUND('',#3835,.T.);
#2716=FACE_OUTER_BOUND('',#3836,.T.);
#2717=FACE_OUTER_BOUND('',#3837,.T.);
#2718=FACE_OUTER_BOUND('',#3838,.T.);
#2719=FACE_OUTER_BOUND('',#3839,.T.);
#2720=FACE_OUTER_BOUND('',#3840,.T.);
#2721=FACE_OUTER_BOUND('',#3841,.T.);
#2722=FACE_OUTER_BOUND('',#3842,.T.);
#2723=FACE_OUTER_BOUND('',#3843,.T.);
#2724=FACE_OUTER_BOUND('',#3844,.T.);
#2725=FACE_OUTER_BOUND('',#3845,.T.);
#2726=FACE_OUTER_BOUND('',#3846,.T.);
#2727=FACE_OUTER_BOUND('',#3847,.T.);
#2728=FACE_OUTER_BOUND('',#3848,.T.);
#2729=FACE_OUTER_BOUND('',#3849,.T.);
#2730=FACE_OUTER_BOUND('',#3850,.T.);
#2731=FACE_OUTER_BOUND('',#3851,.T.);
#2732=FACE_OUTER_BOUND('',#3852,.T.);
#2733=FACE_OUTER_BOUND('',#3853,.T.);
#2734=FACE_OUTER_BOUND('',#3855,.T.);
#2735=FACE_OUTER_BOUND('',#3856,.T.);
#2736=FACE_OUTER_BOUND('',#3857,.T.);
#2737=FACE_OUTER_BOUND('',#3858,.T.);
#2738=FACE_OUTER_BOUND('',#3859,.T.);
#2739=FACE_OUTER_BOUND('',#3860,.T.);
#2740=FACE_OUTER_BOUND('',#3861,.T.);
#2741=FACE_OUTER_BOUND('',#3862,.T.);
#2742=FACE_OUTER_BOUND('',#3863,.T.);
#2743=FACE_OUTER_BOUND('',#3864,.T.);
#2744=FACE_OUTER_BOUND('',#3865,.T.);
#2745=FACE_OUTER_BOUND('',#3866,.T.);
#2746=FACE_OUTER_BOUND('',#3867,.T.);
#2747=FACE_OUTER_BOUND('',#3868,.T.);
#2748=FACE_OUTER_BOUND('',#3869,.T.);
#2749=FACE_OUTER_BOUND('',#3870,.T.);
#2750=FACE_OUTER_BOUND('',#3871,.T.);
#2751=FACE_OUTER_BOUND('',#3872,.T.);
#2752=FACE_OUTER_BOUND('',#3874,.T.);
#2753=FACE_OUTER_BOUND('',#3875,.T.);
#2754=FACE_OUTER_BOUND('',#3876,.T.);
#2755=FACE_OUTER_BOUND('',#3877,.T.);
#2756=FACE_OUTER_BOUND('',#3878,.T.);
#2757=FACE_OUTER_BOUND('',#3879,.T.);
#2758=FACE_OUTER_BOUND('',#3880,.T.);
#2759=FACE_OUTER_BOUND('',#3881,.T.);
#2760=FACE_OUTER_BOUND('',#3882,.T.);
#2761=FACE_OUTER_BOUND('',#3883,.T.);
#2762=FACE_OUTER_BOUND('',#3884,.T.);
#2763=FACE_OUTER_BOUND('',#3885,.T.);
#2764=FACE_OUTER_BOUND('',#3886,.T.);
#2765=FACE_OUTER_BOUND('',#3887,.T.);
#2766=FACE_OUTER_BOUND('',#3888,.T.);
#2767=FACE_OUTER_BOUND('',#3889,.T.);
#2768=FACE_OUTER_BOUND('',#3890,.T.);
#2769=FACE_OUTER_BOUND('',#3891,.T.);
#2770=FACE_OUTER_BOUND('',#3892,.T.);
#2771=FACE_OUTER_BOUND('',#3893,.T.);
#2772=FACE_OUTER_BOUND('',#3894,.T.);
#2773=FACE_OUTER_BOUND('',#3895,.T.);
#2774=FACE_OUTER_BOUND('',#3896,.T.);
#2775=FACE_OUTER_BOUND('',#3897,.T.);
#2776=FACE_OUTER_BOUND('',#3898,.T.);
#2777=FACE_OUTER_BOUND('',#3899,.T.);
#2778=EDGE_LOOP('',(#10764,#10765,#10766,#10767));
#2779=EDGE_LOOP('',(#10768,#10769,#10770,#10771,#10772,#10773,#10774,#10775,
#10776,#10777));
#2780=EDGE_LOOP('',(#10778,#10779,#10780,#10781));
#2781=EDGE_LOOP('',(#10782,#10783,#10784,#10785,#10786,#10787,#10788,#10789));
#2782=EDGE_LOOP('',(#10790,#10791,#10792,#10793));
#2783=EDGE_LOOP('',(#10794,#10795,#10796,#10797,#10798,#10799,#10800,#10801,
#10802,#10803));
#2784=EDGE_LOOP('',(#10804,#10805,#10806,#10807));
#2785=EDGE_LOOP('',(#10808,#10809,#10810,#10811,#10812,#10813,#10814,#10815));
#2786=EDGE_LOOP('',(#10816,#10817,#10818,#10819));
#2787=EDGE_LOOP('',(#10820,#10821,#10822,#10823,#10824,#10825,#10826,#10827));
#2788=EDGE_LOOP('',(#10828));
#2789=EDGE_LOOP('',(#10829));
#2790=EDGE_LOOP('',(#10830));
#2791=EDGE_LOOP('',(#10831,#10832,#10833,#10834));
#2792=EDGE_LOOP('',(#10835,#10836,#10837,#10838));
#2793=EDGE_LOOP('',(#10839,#10840,#10841,#10842,#10843,#10844,#10845,#10846));
#2794=EDGE_LOOP('',(#10847));
#2795=EDGE_LOOP('',(#10848));
#2796=EDGE_LOOP('',(#10849));
#2797=EDGE_LOOP('',(#10850,#10851,#10852,#10853));
#2798=EDGE_LOOP('',(#10854,#10855,#10856,#10857));
#2799=EDGE_LOOP('',(#10858,#10859,#10860,#10861));
#2800=EDGE_LOOP('',(#10862,#10863,#10864,#10865));
#2801=EDGE_LOOP('',(#10866,#10867,#10868,#10869,#10870,#10871,#10872,#10873));
#2802=EDGE_LOOP('',(#10874,#10875,#10876,#10877,#10878));
#2803=EDGE_LOOP('',(#10879,#10880,#10881,#10882,#10883,#10884,#10885,#10886));
#2804=EDGE_LOOP('',(#10887,#10888,#10889,#10890,#10891));
#2805=EDGE_LOOP('',(#10892,#10893,#10894,#10895,#10896,#10897,#10898,#10899,
#10900,#10901,#10902,#10903,#10904));
#2806=EDGE_LOOP('',(#10905));
#2807=EDGE_LOOP('',(#10906,#10907,#10908,#10909));
#2808=EDGE_LOOP('',(#10910,#10911,#10912,#10913));
#2809=EDGE_LOOP('',(#10914,#10915,#10916,#10917));
#2810=EDGE_LOOP('',(#10918,#10919,#10920,#10921));
#2811=EDGE_LOOP('',(#10922,#10923,#10924,#10925));
#2812=EDGE_LOOP('',(#10926,#10927,#10928,#10929));
#2813=EDGE_LOOP('',(#10930,#10931,#10932,#10933,#10934));
#2814=EDGE_LOOP('',(#10935,#10936,#10937,#10938,#10939,#10940,#10941,#10942));
#2815=EDGE_LOOP('',(#10943));
#2816=EDGE_LOOP('',(#10944));
#2817=EDGE_LOOP('',(#10945));
#2818=EDGE_LOOP('',(#10946,#10947,#10948,#10949,#10950));
#2819=EDGE_LOOP('',(#10951,#10952,#10953,#10954,#10955,#10956,#10957,#10958,
#10959,#10960,#10961,#10962,#10963,#10964));
#2820=EDGE_LOOP('',(#10965,#10966,#10967,#10968,#10969));
#2821=EDGE_LOOP('',(#10970,#10971,#10972,#10973,#10974,#10975,#10976,#10977));
#2822=EDGE_LOOP('',(#10978));
#2823=EDGE_LOOP('',(#10979));
#2824=EDGE_LOOP('',(#10980));
#2825=EDGE_LOOP('',(#10981,#10982,#10983,#10984));
#2826=EDGE_LOOP('',(#10985,#10986,#10987,#10988));
#2827=EDGE_LOOP('',(#10989));
#2828=EDGE_LOOP('',(#10990));
#2829=EDGE_LOOP('',(#10991));
#2830=EDGE_LOOP('',(#10992));
#2831=EDGE_LOOP('',(#10993));
#2832=EDGE_LOOP('',(#10994));
#2833=EDGE_LOOP('',(#10995));
#2834=EDGE_LOOP('',(#10996));
#2835=EDGE_LOOP('',(#10997,#10998,#10999,#11000,#11001,#11002,#11003));
#2836=EDGE_LOOP('',(#11004,#11005,#11006,#11007));
#2837=EDGE_LOOP('',(#11008,#11009,#11010,#11011));
#2838=EDGE_LOOP('',(#11012,#11013,#11014,#11015));
#2839=EDGE_LOOP('',(#11016,#11017,#11018,#11019,#11020,#11021,#11022,#11023));
#2840=EDGE_LOOP('',(#11024,#11025,#11026,#11027,#11028,#11029,#11030,#11031));
#2841=EDGE_LOOP('',(#11032,#11033,#11034,#11035));
#2842=EDGE_LOOP('',(#11036,#11037,#11038,#11039));
#2843=EDGE_LOOP('',(#11040,#11041,#11042,#11043));
#2844=EDGE_LOOP('',(#11044,#11045,#11046,#11047));
#2845=EDGE_LOOP('',(#11048,#11049,#11050,#11051));
#2846=EDGE_LOOP('',(#11052,#11053,#11054,#11055));
#2847=EDGE_LOOP('',(#11056,#11057,#11058,#11059));
#2848=EDGE_LOOP('',(#11060,#11061,#11062,#11063));
#2849=EDGE_LOOP('',(#11064,#11065,#11066,#11067,#11068));
#2850=EDGE_LOOP('',(#11069,#11070,#11071,#11072));
#2851=EDGE_LOOP('',(#11073,#11074,#11075,#11076));
#2852=EDGE_LOOP('',(#11077,#11078,#11079,#11080));
#2853=EDGE_LOOP('',(#11081,#11082,#11083,#11084));
#2854=EDGE_LOOP('',(#11085,#11086,#11087,#11088,#11089,#11090,#11091));
#2855=EDGE_LOOP('',(#11092,#11093,#11094,#11095));
#2856=EDGE_LOOP('',(#11096,#11097,#11098,#11099,#11100,#11101,#11102,#11103));
#2857=EDGE_LOOP('',(#11104,#11105,#11106,#11107,#11108));
#2858=EDGE_LOOP('',(#11109,#11110,#11111,#11112,#11113));
#2859=EDGE_LOOP('',(#11114,#11115,#11116,#11117,#11118,#11119,#11120));
#2860=EDGE_LOOP('',(#11121,#11122,#11123,#11124,#11125,#11126));
#2861=EDGE_LOOP('',(#11127,#11128,#11129,#11130,#11131,#11132));
#2862=EDGE_LOOP('',(#11133,#11134,#11135,#11136,#11137,#11138,#11139));
#2863=EDGE_LOOP('',(#11140,#11141,#11142));
#2864=EDGE_LOOP('',(#11143,#11144,#11145,#11146,#11147,#11148,#11149,#11150,
#11151,#11152,#11153,#11154));
#2865=EDGE_LOOP('',(#11155,#11156,#11157,#11158,#11159));
#2866=EDGE_LOOP('',(#11160,#11161,#11162,#11163,#11164,#11165));
#2867=EDGE_LOOP('',(#11166,#11167,#11168,#11169));
#2868=EDGE_LOOP('',(#11170,#11171,#11172,#11173));
#2869=EDGE_LOOP('',(#11174,#11175,#11176,#11177));
#2870=EDGE_LOOP('',(#11178,#11179,#11180,#11181,#11182,#11183,#11184));
#2871=EDGE_LOOP('',(#11185,#11186,#11187,#11188,#11189,#11190));
#2872=EDGE_LOOP('',(#11191,#11192,#11193,#11194,#11195,#11196,#11197,#11198,
#11199));
#2873=EDGE_LOOP('',(#11200,#11201,#11202,#11203));
#2874=EDGE_LOOP('',(#11204,#11205,#11206,#11207));
#2875=EDGE_LOOP('',(#11208,#11209,#11210,#11211));
#2876=EDGE_LOOP('',(#11212,#11213,#11214,#11215));
#2877=EDGE_LOOP('',(#11216,#11217,#11218,#11219));
#2878=EDGE_LOOP('',(#11220,#11221,#11222,#11223));
#2879=EDGE_LOOP('',(#11224,#11225,#11226,#11227));
#2880=EDGE_LOOP('',(#11228,#11229,#11230,#11231));
#2881=EDGE_LOOP('',(#11232,#11233,#11234,#11235));
#2882=EDGE_LOOP('',(#11236,#11237,#11238,#11239,#11240,#11241,#11242,#11243));
#2883=EDGE_LOOP('',(#11244,#11245,#11246,#11247));
#2884=EDGE_LOOP('',(#11248,#11249,#11250,#11251));
#2885=EDGE_LOOP('',(#11252,#11253,#11254,#11255));
#2886=EDGE_LOOP('',(#11256,#11257,#11258,#11259,#11260,#11261));
#2887=EDGE_LOOP('',(#11262,#11263,#11264,#11265,#11266));
#2888=EDGE_LOOP('',(#11267,#11268,#11269,#11270,#11271,#11272));
#2889=EDGE_LOOP('',(#11273,#11274,#11275,#11276,#11277,#11278));
#2890=EDGE_LOOP('',(#11279,#11280,#11281,#11282,#11283,#11284,#11285,#11286,
#11287));
#2891=EDGE_LOOP('',(#11288,#11289));
#2892=EDGE_LOOP('',(#11290,#11291,#11292,#11293));
#2893=EDGE_LOOP('',(#11294,#11295));
#2894=EDGE_LOOP('',(#11296,#11297,#11298,#11299));
#2895=EDGE_LOOP('',(#11300,#11301));
#2896=EDGE_LOOP('',(#11302,#11303,#11304,#11305));
#2897=EDGE_LOOP('',(#11306,#11307));
#2898=EDGE_LOOP('',(#11308,#11309,#11310,#11311));
#2899=EDGE_LOOP('',(#11312,#11313));
#2900=EDGE_LOOP('',(#11314,#11315,#11316,#11317));
#2901=EDGE_LOOP('',(#11318,#11319));
#2902=EDGE_LOOP('',(#11320,#11321,#11322,#11323));
#2903=EDGE_LOOP('',(#11324,#11325));
#2904=EDGE_LOOP('',(#11326,#11327));
#2905=EDGE_LOOP('',(#11328,#11329));
#2906=EDGE_LOOP('',(#11330,#11331));
#2907=EDGE_LOOP('',(#11332,#11333));
#2908=EDGE_LOOP('',(#11334,#11335));
#2909=EDGE_LOOP('',(#11336));
#2910=EDGE_LOOP('',(#11337));
#2911=EDGE_LOOP('',(#11338,#11339,#11340,#11341));
#2912=EDGE_LOOP('',(#11342,#11343,#11344,#11345));
#2913=EDGE_LOOP('',(#11346,#11347,#11348,#11349,#11350,#11351));
#2914=EDGE_LOOP('',(#11352,#11353,#11354,#11355));
#2915=EDGE_LOOP('',(#11356,#11357,#11358,#11359));
#2916=EDGE_LOOP('',(#11360,#11361,#11362,#11363));
#2917=EDGE_LOOP('',(#11364,#11365,#11366,#11367));
#2918=EDGE_LOOP('',(#11368,#11369,#11370,#11371));
#2919=EDGE_LOOP('',(#11372,#11373,#11374,#11375));
#2920=EDGE_LOOP('',(#11376,#11377,#11378,#11379));
#2921=EDGE_LOOP('',(#11380));
#2922=EDGE_LOOP('',(#11381));
#2923=EDGE_LOOP('',(#11382,#11383,#11384,#11385));
#2924=EDGE_LOOP('',(#11386));
#2925=EDGE_LOOP('',(#11387));
#2926=EDGE_LOOP('',(#11388));
#2927=EDGE_LOOP('',(#11389));
#2928=EDGE_LOOP('',(#11390,#11391,#11392,#11393));
#2929=EDGE_LOOP('',(#11394,#11395,#11396,#11397,#11398,#11399,#11400,#11401,
#11402,#11403,#11404,#11405,#11406,#11407,#11408,#11409));
#2930=EDGE_LOOP('',(#11410,#11411));
#2931=EDGE_LOOP('',(#11412,#11413,#11414,#11415));
#2932=EDGE_LOOP('',(#11416,#11417,#11418,#11419));
#2933=EDGE_LOOP('',(#11420,#11421,#11422,#11423,#11424));
#2934=EDGE_LOOP('',(#11425,#11426,#11427,#11428,#11429,#11430,#11431));
#2935=EDGE_LOOP('',(#11432,#11433,#11434,#11435));
#2936=EDGE_LOOP('',(#11436,#11437,#11438,#11439));
#2937=EDGE_LOOP('',(#11440,#11441,#11442,#11443));
#2938=EDGE_LOOP('',(#11444,#11445,#11446,#11447));
#2939=EDGE_LOOP('',(#11448,#11449,#11450,#11451));
#2940=EDGE_LOOP('',(#11452,#11453,#11454,#11455));
#2941=EDGE_LOOP('',(#11456,#11457,#11458,#11459,#11460,#11461,#11462));
#2942=EDGE_LOOP('',(#11463,#11464,#11465,#11466,#11467,#11468,#11469));
#2943=EDGE_LOOP('',(#11470,#11471,#11472,#11473));
#2944=EDGE_LOOP('',(#11474,#11475,#11476,#11477));
#2945=EDGE_LOOP('',(#11478,#11479,#11480,#11481));
#2946=EDGE_LOOP('',(#11482,#11483,#11484,#11485,#11486,#11487,#11488));
#2947=EDGE_LOOP('',(#11489,#11490,#11491,#11492,#11493,#11494,#11495));
#2948=EDGE_LOOP('',(#11496,#11497,#11498,#11499));
#2949=EDGE_LOOP('',(#11500,#11501,#11502,#11503));
#2950=EDGE_LOOP('',(#11504));
#2951=EDGE_LOOP('',(#11505));
#2952=EDGE_LOOP('',(#11506,#11507,#11508,#11509));
#2953=EDGE_LOOP('',(#11510,#11511,#11512,#11513,#11514));
#2954=EDGE_LOOP('',(#11515,#11516,#11517,#11518,#11519));
#2955=EDGE_LOOP('',(#11520,#11521,#11522,#11523,#11524));
#2956=EDGE_LOOP('',(#11525,#11526));
#2957=EDGE_LOOP('',(#11527));
#2958=EDGE_LOOP('',(#11528));
#2959=EDGE_LOOP('',(#11529));
#2960=EDGE_LOOP('',(#11530));
#2961=EDGE_LOOP('',(#11531));
#2962=EDGE_LOOP('',(#11532));
#2963=EDGE_LOOP('',(#11533));
#2964=EDGE_LOOP('',(#11534));
#2965=EDGE_LOOP('',(#11535,#11536,#11537,#11538));
#2966=EDGE_LOOP('',(#11539));
#2967=EDGE_LOOP('',(#11540,#11541,#11542,#11543));
#2968=EDGE_LOOP('',(#11544,#11545,#11546,#11547));
#2969=EDGE_LOOP('',(#11548,#11549,#11550,#11551));
#2970=EDGE_LOOP('',(#11552,#11553,#11554,#11555));
#2971=EDGE_LOOP('',(#11556,#11557,#11558,#11559));
#2972=EDGE_LOOP('',(#11560,#11561,#11562,#11563));
#2973=EDGE_LOOP('',(#11564));
#2974=EDGE_LOOP('',(#11565));
#2975=EDGE_LOOP('',(#11566,#11567,#11568,#11569));
#2976=EDGE_LOOP('',(#11570,#11571,#11572,#11573));
#2977=EDGE_LOOP('',(#11574));
#2978=EDGE_LOOP('',(#11575));
#2979=EDGE_LOOP('',(#11576));
#2980=EDGE_LOOP('',(#11577));
#2981=EDGE_LOOP('',(#11578));
#2982=EDGE_LOOP('',(#11579));
#2983=EDGE_LOOP('',(#11580));
#2984=EDGE_LOOP('',(#11581));
#2985=EDGE_LOOP('',(#11582,#11583,#11584,#11585));
#2986=EDGE_LOOP('',(#11586,#11587,#11588,#11589));
#2987=EDGE_LOOP('',(#11590,#11591,#11592,#11593));
#2988=EDGE_LOOP('',(#11594,#11595,#11596,#11597));
#2989=EDGE_LOOP('',(#11598));
#2990=EDGE_LOOP('',(#11599));
#2991=EDGE_LOOP('',(#11600,#11601,#11602,#11603,#11604,#11605));
#2992=EDGE_LOOP('',(#11606,#11607,#11608,#11609,#11610));
#2993=EDGE_LOOP('',(#11611));
#2994=EDGE_LOOP('',(#11612));
#2995=EDGE_LOOP('',(#11613));
#2996=EDGE_LOOP('',(#11614));
#2997=EDGE_LOOP('',(#11615));
#2998=EDGE_LOOP('',(#11616));
#2999=EDGE_LOOP('',(#11617));
#3000=EDGE_LOOP('',(#11618));
#3001=EDGE_LOOP('',(#11619,#11620,#11621,#11622,#11623));
#3002=EDGE_LOOP('',(#11624,#11625));
#3003=EDGE_LOOP('',(#11626,#11627,#11628));
#3004=EDGE_LOOP('',(#11629,#11630,#11631,#11632));
#3005=EDGE_LOOP('',(#11633));
#3006=EDGE_LOOP('',(#11634,#11635,#11636,#11637));
#3007=EDGE_LOOP('',(#11638,#11639,#11640,#11641));
#3008=EDGE_LOOP('',(#11642,#11643,#11644,#11645));
#3009=EDGE_LOOP('',(#11646,#11647,#11648,#11649));
#3010=EDGE_LOOP('',(#11650,#11651,#11652,#11653));
#3011=EDGE_LOOP('',(#11654,#11655,#11656,#11657));
#3012=EDGE_LOOP('',(#11658,#11659,#11660,#11661));
#3013=EDGE_LOOP('',(#11662,#11663,#11664,#11665));
#3014=EDGE_LOOP('',(#11666));
#3015=EDGE_LOOP('',(#11667));
#3016=EDGE_LOOP('',(#11668));
#3017=EDGE_LOOP('',(#11669));
#3018=EDGE_LOOP('',(#11670));
#3019=EDGE_LOOP('',(#11671));
#3020=EDGE_LOOP('',(#11672));
#3021=EDGE_LOOP('',(#11673));
#3022=EDGE_LOOP('',(#11674,#11675,#11676,#11677));
#3023=EDGE_LOOP('',(#11678,#11679,#11680,#11681));
#3024=EDGE_LOOP('',(#11682));
#3025=EDGE_LOOP('',(#11683));
#3026=EDGE_LOOP('',(#11684,#11685,#11686,#11687));
#3027=EDGE_LOOP('',(#11688,#11689,#11690,#11691));
#3028=EDGE_LOOP('',(#11692,#11693,#11694,#11695));
#3029=EDGE_LOOP('',(#11696,#11697,#11698,#11699));
#3030=EDGE_LOOP('',(#11700,#11701,#11702,#11703));
#3031=EDGE_LOOP('',(#11704,#11705,#11706,#11707));
#3032=EDGE_LOOP('',(#11708,#11709,#11710,#11711));
#3033=EDGE_LOOP('',(#11712));
#3034=EDGE_LOOP('',(#11713));
#3035=EDGE_LOOP('',(#11714));
#3036=EDGE_LOOP('',(#11715));
#3037=EDGE_LOOP('',(#11716));
#3038=EDGE_LOOP('',(#11717));
#3039=EDGE_LOOP('',(#11718));
#3040=EDGE_LOOP('',(#11719));
#3041=EDGE_LOOP('',(#11720,#11721,#11722,#11723));
#3042=EDGE_LOOP('',(#11724));
#3043=EDGE_LOOP('',(#11725));
#3044=EDGE_LOOP('',(#11726));
#3045=EDGE_LOOP('',(#11727));
#3046=EDGE_LOOP('',(#11728));
#3047=EDGE_LOOP('',(#11729));
#3048=EDGE_LOOP('',(#11730));
#3049=EDGE_LOOP('',(#11731));
#3050=EDGE_LOOP('',(#11732,#11733,#11734,#11735));
#3051=EDGE_LOOP('',(#11736,#11737,#11738,#11739));
#3052=EDGE_LOOP('',(#11740,#11741,#11742,#11743));
#3053=EDGE_LOOP('',(#11744,#11745,#11746,#11747));
#3054=EDGE_LOOP('',(#11748,#11749,#11750,#11751));
#3055=EDGE_LOOP('',(#11752,#11753,#11754,#11755));
#3056=EDGE_LOOP('',(#11756,#11757,#11758,#11759));
#3057=EDGE_LOOP('',(#11760));
#3058=EDGE_LOOP('',(#11761));
#3059=EDGE_LOOP('',(#11762,#11763,#11764,#11765));
#3060=EDGE_LOOP('',(#11766));
#3061=EDGE_LOOP('',(#11767));
#3062=EDGE_LOOP('',(#11768));
#3063=EDGE_LOOP('',(#11769));
#3064=EDGE_LOOP('',(#11770));
#3065=EDGE_LOOP('',(#11771));
#3066=EDGE_LOOP('',(#11772));
#3067=EDGE_LOOP('',(#11773));
#3068=EDGE_LOOP('',(#11774,#11775,#11776,#11777));
#3069=EDGE_LOOP('',(#11778));
#3070=EDGE_LOOP('',(#11779));
#3071=EDGE_LOOP('',(#11780));
#3072=EDGE_LOOP('',(#11781));
#3073=EDGE_LOOP('',(#11782));
#3074=EDGE_LOOP('',(#11783));
#3075=EDGE_LOOP('',(#11784));
#3076=EDGE_LOOP('',(#11785));
#3077=EDGE_LOOP('',(#11786,#11787,#11788,#11789));
#3078=EDGE_LOOP('',(#11790));
#3079=EDGE_LOOP('',(#11791));
#3080=EDGE_LOOP('',(#11792,#11793,#11794,#11795,#11796));
#3081=EDGE_LOOP('',(#11797));
#3082=EDGE_LOOP('',(#11798));
#3083=EDGE_LOOP('',(#11799,#11800,#11801,#11802,#11803));
#3084=EDGE_LOOP('',(#11804,#11805,#11806,#11807));
#3085=EDGE_LOOP('',(#11808,#11809,#11810,#11811));
#3086=EDGE_LOOP('',(#11812));
#3087=EDGE_LOOP('',(#11813));
#3088=EDGE_LOOP('',(#11814,#11815,#11816,#11817,#11818));
#3089=EDGE_LOOP('',(#11819));
#3090=EDGE_LOOP('',(#11820));
#3091=EDGE_LOOP('',(#11821,#11822,#11823,#11824,#11825));
#3092=EDGE_LOOP('',(#11826,#11827,#11828,#11829,#11830));
#3093=EDGE_LOOP('',(#11831,#11832,#11833,#11834,#11835,#11836));
#3094=EDGE_LOOP('',(#11837));
#3095=EDGE_LOOP('',(#11838));
#3096=EDGE_LOOP('',(#11839,#11840,#11841,#11842,#11843));
#3097=EDGE_LOOP('',(#11844,#11845,#11846,#11847));
#3098=EDGE_LOOP('',(#11848,#11849,#11850,#11851));
#3099=EDGE_LOOP('',(#11852,#11853,#11854,#11855));
#3100=EDGE_LOOP('',(#11856,#11857,#11858,#11859));
#3101=EDGE_LOOP('',(#11860,#11861,#11862,#11863));
#3102=EDGE_LOOP('',(#11864,#11865,#11866,#11867));
#3103=EDGE_LOOP('',(#11868,#11869,#11870,#11871));
#3104=EDGE_LOOP('',(#11872,#11873,#11874,#11875));
#3105=EDGE_LOOP('',(#11876,#11877,#11878,#11879));
#3106=EDGE_LOOP('',(#11880,#11881,#11882,#11883));
#3107=EDGE_LOOP('',(#11884,#11885,#11886,#11887));
#3108=EDGE_LOOP('',(#11888,#11889,#11890,#11891));
#3109=EDGE_LOOP('',(#11892,#11893,#11894,#11895));
#3110=EDGE_LOOP('',(#11896,#11897,#11898,#11899));
#3111=EDGE_LOOP('',(#11900,#11901,#11902,#11903));
#3112=EDGE_LOOP('',(#11904,#11905,#11906,#11907));
#3113=EDGE_LOOP('',(#11908,#11909,#11910,#11911));
#3114=EDGE_LOOP('',(#11912,#11913,#11914,#11915));
#3115=EDGE_LOOP('',(#11916,#11917,#11918,#11919));
#3116=EDGE_LOOP('',(#11920,#11921,#11922,#11923));
#3117=EDGE_LOOP('',(#11924,#11925,#11926,#11927));
#3118=EDGE_LOOP('',(#11928,#11929,#11930,#11931));
#3119=EDGE_LOOP('',(#11932,#11933,#11934,#11935));
#3120=EDGE_LOOP('',(#11936,#11937,#11938,#11939));
#3121=EDGE_LOOP('',(#11940,#11941,#11942,#11943));
#3122=EDGE_LOOP('',(#11944,#11945,#11946,#11947));
#3123=EDGE_LOOP('',(#11948,#11949,#11950,#11951));
#3124=EDGE_LOOP('',(#11952,#11953,#11954,#11955));
#3125=EDGE_LOOP('',(#11956,#11957,#11958,#11959));
#3126=EDGE_LOOP('',(#11960,#11961,#11962,#11963));
#3127=EDGE_LOOP('',(#11964,#11965,#11966,#11967));
#3128=EDGE_LOOP('',(#11968,#11969,#11970,#11971));
#3129=EDGE_LOOP('',(#11972,#11973,#11974,#11975));
#3130=EDGE_LOOP('',(#11976,#11977,#11978,#11979));
#3131=EDGE_LOOP('',(#11980,#11981,#11982,#11983));
#3132=EDGE_LOOP('',(#11984,#11985,#11986,#11987));
#3133=EDGE_LOOP('',(#11988,#11989,#11990,#11991));
#3134=EDGE_LOOP('',(#11992,#11993,#11994,#11995));
#3135=EDGE_LOOP('',(#11996,#11997,#11998,#11999));
#3136=EDGE_LOOP('',(#12000,#12001,#12002,#12003));
#3137=EDGE_LOOP('',(#12004,#12005,#12006,#12007));
#3138=EDGE_LOOP('',(#12008,#12009,#12010,#12011));
#3139=EDGE_LOOP('',(#12012,#12013,#12014,#12015));
#3140=EDGE_LOOP('',(#12016,#12017,#12018,#12019));
#3141=EDGE_LOOP('',(#12020,#12021,#12022,#12023));
#3142=EDGE_LOOP('',(#12024,#12025,#12026,#12027));
#3143=EDGE_LOOP('',(#12028,#12029,#12030,#12031));
#3144=EDGE_LOOP('',(#12032,#12033,#12034,#12035));
#3145=EDGE_LOOP('',(#12036,#12037,#12038,#12039));
#3146=EDGE_LOOP('',(#12040,#12041,#12042,#12043));
#3147=EDGE_LOOP('',(#12044,#12045,#12046,#12047));
#3148=EDGE_LOOP('',(#12048,#12049,#12050,#12051));
#3149=EDGE_LOOP('',(#12052,#12053,#12054,#12055));
#3150=EDGE_LOOP('',(#12056,#12057,#12058,#12059));
#3151=EDGE_LOOP('',(#12060,#12061,#12062,#12063));
#3152=EDGE_LOOP('',(#12064,#12065,#12066,#12067));
#3153=EDGE_LOOP('',(#12068,#12069,#12070,#12071));
#3154=EDGE_LOOP('',(#12072,#12073,#12074,#12075));
#3155=EDGE_LOOP('',(#12076,#12077,#12078,#12079));
#3156=EDGE_LOOP('',(#12080,#12081,#12082,#12083));
#3157=EDGE_LOOP('',(#12084,#12085,#12086,#12087));
#3158=EDGE_LOOP('',(#12088,#12089,#12090,#12091,#12092));
#3159=EDGE_LOOP('',(#12093,#12094,#12095,#12096,#12097,#12098,#12099,#12100,
#12101,#12102,#12103,#12104,#12105,#12106,#12107,#12108,#12109,#12110,#12111,
#12112,#12113,#12114,#12115,#12116,#12117,#12118,#12119,#12120,#12121,#12122,
#12123,#12124,#12125,#12126));
#3160=EDGE_LOOP('',(#12127,#12128,#12129,#12130));
#3161=EDGE_LOOP('',(#12131,#12132,#12133,#12134,#12135,#12136,#12137,#12138,
#12139,#12140,#12141,#12142,#12143,#12144,#12145,#12146,#12147,#12148,#12149,
#12150,#12151,#12152,#12153,#12154,#12155,#12156,#12157,#12158,#12159,#12160,
#12161,#12162,#12163,#12164));
#3162=EDGE_LOOP('',(#12165,#12166,#12167,#12168));
#3163=EDGE_LOOP('',(#12169,#12170,#12171,#12172,#12173,#12174,#12175,#12176,
#12177,#12178,#12179,#12180,#12181,#12182,#12183,#12184,#12185,#12186,#12187,
#12188,#12189,#12190,#12191,#12192,#12193,#12194,#12195,#12196,#12197,#12198,
#12199,#12200,#12201,#12202));
#3164=EDGE_LOOP('',(#12203,#12204,#12205,#12206,#12207));
#3165=EDGE_LOOP('',(#12208,#12209,#12210,#12211));
#3166=EDGE_LOOP('',(#12212,#12213,#12214,#12215,#12216,#12217,#12218,#12219,
#12220,#12221,#12222,#12223,#12224,#12225,#12226,#12227,#12228,#12229,#12230,
#12231,#12232,#12233,#12234,#12235,#12236,#12237,#12238,#12239,#12240,#12241,
#12242,#12243,#12244,#12245));
#3167=EDGE_LOOP('',(#12246));
#3168=EDGE_LOOP('',(#12247,#12248,#12249,#12250,#12251,#12252));
#3169=EDGE_LOOP('',(#12253,#12254,#12255,#12256));
#3170=EDGE_LOOP('',(#12257));
#3171=EDGE_LOOP('',(#12258,#12259,#12260,#12261));
#3172=EDGE_LOOP('',(#12262,#12263,#12264,#12265));
#3173=EDGE_LOOP('',(#12266));
#3174=EDGE_LOOP('',(#12267,#12268,#12269,#12270));
#3175=EDGE_LOOP('',(#12271,#12272,#12273,#12274,#12275,#12276));
#3176=EDGE_LOOP('',(#12277));
#3177=EDGE_LOOP('',(#12278,#12279,#12280,#12281,#12282,#12283,#12284,#12285,
#12286,#12287,#12288,#12289,#12290,#12291,#12292,#12293));
#3178=EDGE_LOOP('',(#12294,#12295,#12296,#12297,#12298,#12299));
#3179=EDGE_LOOP('',(#12300,#12301,#12302,#12303,#12304,#12305));
#3180=EDGE_LOOP('',(#12306,#12307,#12308));
#3181=EDGE_LOOP('',(#12309,#12310,#12311));
#3182=EDGE_LOOP('',(#12312,#12313,#12314));
#3183=EDGE_LOOP('',(#12315,#12316,#12317));
#3184=EDGE_LOOP('',(#12318,#12319,#12320));
#3185=EDGE_LOOP('',(#12321,#12322,#12323));
#3186=EDGE_LOOP('',(#12324,#12325,#12326,#12327,#12328,#12329));
#3187=EDGE_LOOP('',(#12330));
#3188=EDGE_LOOP('',(#12331));
#3189=EDGE_LOOP('',(#12332,#12333,#12334));
#3190=EDGE_LOOP('',(#12335,#12336,#12337));
#3191=EDGE_LOOP('',(#12338,#12339,#12340));
#3192=EDGE_LOOP('',(#12341,#12342,#12343));
#3193=EDGE_LOOP('',(#12344,#12345,#12346));
#3194=EDGE_LOOP('',(#12347,#12348,#12349));
#3195=EDGE_LOOP('',(#12350,#12351,#12352,#12353,#12354,#12355));
#3196=EDGE_LOOP('',(#12356,#12357,#12358,#12359));
#3197=EDGE_LOOP('',(#12360,#12361,#12362,#12363,#12364,#12365,#12366));
#3198=EDGE_LOOP('',(#12367,#12368,#12369,#12370));
#3199=EDGE_LOOP('',(#12371,#12372,#12373,#12374));
#3200=EDGE_LOOP('',(#12375,#12376,#12377,#12378,#12379,#12380));
#3201=EDGE_LOOP('',(#12381,#12382,#12383,#12384));
#3202=EDGE_LOOP('',(#12385,#12386,#12387,#12388));
#3203=EDGE_LOOP('',(#12389,#12390,#12391,#12392));
#3204=EDGE_LOOP('',(#12393,#12394,#12395,#12396));
#3205=EDGE_LOOP('',(#12397,#12398,#12399,#12400));
#3206=EDGE_LOOP('',(#12401,#12402,#12403,#12404));
#3207=EDGE_LOOP('',(#12405,#12406,#12407,#12408,#12409,#12410,#12411,#12412,
#12413,#12414,#12415,#12416,#12417,#12418,#12419,#12420));
#3208=EDGE_LOOP('',(#12421,#12422,#12423,#12424));
#3209=EDGE_LOOP('',(#12425,#12426,#12427,#12428));
#3210=EDGE_LOOP('',(#12429,#12430,#12431,#12432));
#3211=EDGE_LOOP('',(#12433,#12434,#12435,#12436));
#3212=EDGE_LOOP('',(#12437,#12438,#12439,#12440,#12441));
#3213=EDGE_LOOP('',(#12442,#12443,#12444,#12445));
#3214=EDGE_LOOP('',(#12446));
#3215=EDGE_LOOP('',(#12447));
#3216=EDGE_LOOP('',(#12448,#12449,#12450,#12451,#12452));
#3217=EDGE_LOOP('',(#12453));
#3218=EDGE_LOOP('',(#12454));
#3219=EDGE_LOOP('',(#12455,#12456,#12457,#12458,#12459,#12460,#12461,#12462,
#12463,#12464,#12465,#12466,#12467));
#3220=EDGE_LOOP('',(#12468,#12469,#12470,#12471));
#3221=EDGE_LOOP('',(#12472));
#3222=EDGE_LOOP('',(#12473));
#3223=EDGE_LOOP('',(#12474,#12475,#12476,#12477));
#3224=EDGE_LOOP('',(#12478,#12479,#12480,#12481));
#3225=EDGE_LOOP('',(#12482,#12483,#12484,#12485,#12486));
#3226=EDGE_LOOP('',(#12487,#12488,#12489,#12490,#12491));
#3227=EDGE_LOOP('',(#12492));
#3228=EDGE_LOOP('',(#12493));
#3229=EDGE_LOOP('',(#12494,#12495,#12496,#12497,#12498));
#3230=EDGE_LOOP('',(#12499,#12500,#12501,#12502,#12503));
#3231=EDGE_LOOP('',(#12504));
#3232=EDGE_LOOP('',(#12505));
#3233=EDGE_LOOP('',(#12506,#12507,#12508,#12509));
#3234=EDGE_LOOP('',(#12510));
#3235=EDGE_LOOP('',(#12511));
#3236=EDGE_LOOP('',(#12512,#12513,#12514,#12515));
#3237=EDGE_LOOP('',(#12516,#12517,#12518,#12519));
#3238=EDGE_LOOP('',(#12520,#12521,#12522,#12523));
#3239=EDGE_LOOP('',(#12524,#12525,#12526,#12527));
#3240=EDGE_LOOP('',(#12528,#12529,#12530,#12531));
#3241=EDGE_LOOP('',(#12532,#12533,#12534,#12535));
#3242=EDGE_LOOP('',(#12536,#12537,#12538,#12539));
#3243=EDGE_LOOP('',(#12540,#12541,#12542,#12543));
#3244=EDGE_LOOP('',(#12544,#12545,#12546,#12547));
#3245=EDGE_LOOP('',(#12548,#12549,#12550,#12551));
#3246=EDGE_LOOP('',(#12552,#12553,#12554,#12555));
#3247=EDGE_LOOP('',(#12556,#12557,#12558,#12559));
#3248=EDGE_LOOP('',(#12560));
#3249=EDGE_LOOP('',(#12561,#12562,#12563,#12564,#12565,#12566,#12567,#12568));
#3250=EDGE_LOOP('',(#12569));
#3251=EDGE_LOOP('',(#12570));
#3252=EDGE_LOOP('',(#12571));
#3253=EDGE_LOOP('',(#12572,#12573,#12574,#12575));
#3254=EDGE_LOOP('',(#12576,#12577,#12578,#12579));
#3255=EDGE_LOOP('',(#12580,#12581,#12582,#12583));
#3256=EDGE_LOOP('',(#12584,#12585,#12586,#12587));
#3257=EDGE_LOOP('',(#12588,#12589,#12590,#12591));
#3258=EDGE_LOOP('',(#12592,#12593,#12594,#12595));
#3259=EDGE_LOOP('',(#12596,#12597,#12598,#12599));
#3260=EDGE_LOOP('',(#12600,#12601,#12602,#12603));
#3261=EDGE_LOOP('',(#12604,#12605,#12606,#12607));
#3262=EDGE_LOOP('',(#12608,#12609,#12610,#12611));
#3263=EDGE_LOOP('',(#12612,#12613,#12614,#12615));
#3264=EDGE_LOOP('',(#12616,#12617,#12618,#12619,#12620,#12621,#12622,#12623));
#3265=EDGE_LOOP('',(#12624));
#3266=EDGE_LOOP('',(#12625));
#3267=EDGE_LOOP('',(#12626,#12627,#12628,#12629));
#3268=EDGE_LOOP('',(#12630,#12631,#12632,#12633));
#3269=EDGE_LOOP('',(#12634,#12635,#12636,#12637));
#3270=EDGE_LOOP('',(#12638,#12639,#12640,#12641));
#3271=EDGE_LOOP('',(#12642,#12643,#12644,#12645));
#3272=EDGE_LOOP('',(#12646,#12647,#12648,#12649));
#3273=EDGE_LOOP('',(#12650,#12651,#12652,#12653));
#3274=EDGE_LOOP('',(#12654,#12655,#12656,#12657));
#3275=EDGE_LOOP('',(#12658,#12659,#12660,#12661));
#3276=EDGE_LOOP('',(#12662,#12663,#12664,#12665));
#3277=EDGE_LOOP('',(#12666,#12667,#12668,#12669));
#3278=EDGE_LOOP('',(#12670,#12671,#12672,#12673));
#3279=EDGE_LOOP('',(#12674));
#3280=EDGE_LOOP('',(#12675,#12676,#12677,#12678,#12679,#12680,#12681,#12682));
#3281=EDGE_LOOP('',(#12683));
#3282=EDGE_LOOP('',(#12684));
#3283=EDGE_LOOP('',(#12685));
#3284=EDGE_LOOP('',(#12686,#12687,#12688,#12689));
#3285=EDGE_LOOP('',(#12690,#12691,#12692,#12693));
#3286=EDGE_LOOP('',(#12694,#12695,#12696,#12697));
#3287=EDGE_LOOP('',(#12698,#12699,#12700,#12701));
#3288=EDGE_LOOP('',(#12702,#12703,#12704,#12705));
#3289=EDGE_LOOP('',(#12706,#12707,#12708,#12709));
#3290=EDGE_LOOP('',(#12710,#12711,#12712,#12713));
#3291=EDGE_LOOP('',(#12714,#12715,#12716,#12717));
#3292=EDGE_LOOP('',(#12718,#12719,#12720,#12721));
#3293=EDGE_LOOP('',(#12722,#12723,#12724,#12725));
#3294=EDGE_LOOP('',(#12726,#12727,#12728,#12729));
#3295=EDGE_LOOP('',(#12730,#12731,#12732,#12733,#12734,#12735,#12736,#12737));
#3296=EDGE_LOOP('',(#12738));
#3297=EDGE_LOOP('',(#12739));
#3298=EDGE_LOOP('',(#12740,#12741,#12742));
#3299=EDGE_LOOP('',(#12743,#12744));
#3300=EDGE_LOOP('',(#12745,#12746,#12747));
#3301=EDGE_LOOP('',(#12748,#12749));
#3302=EDGE_LOOP('',(#12750,#12751,#12752,#12753));
#3303=EDGE_LOOP('',(#12754,#12755,#12756,#12757));
#3304=EDGE_LOOP('',(#12758,#12759,#12760,#12761));
#3305=EDGE_LOOP('',(#12762,#12763,#12764,#12765));
#3306=EDGE_LOOP('',(#12766,#12767,#12768,#12769,#12770,#12771));
#3307=EDGE_LOOP('',(#12772,#12773,#12774,#12775,#12776,#12777));
#3308=EDGE_LOOP('',(#12778,#12779,#12780,#12781));
#3309=EDGE_LOOP('',(#12782));
#3310=EDGE_LOOP('',(#12783));
#3311=EDGE_LOOP('',(#12784,#12785,#12786,#12787));
#3312=EDGE_LOOP('',(#12788));
#3313=EDGE_LOOP('',(#12789,#12790,#12791,#12792));
#3314=EDGE_LOOP('',(#12793,#12794,#12795,#12796));
#3315=EDGE_LOOP('',(#12797));
#3316=EDGE_LOOP('',(#12798,#12799,#12800,#12801));
#3317=EDGE_LOOP('',(#12802,#12803,#12804,#12805));
#3318=EDGE_LOOP('',(#12806,#12807,#12808,#12809));
#3319=EDGE_LOOP('',(#12810,#12811,#12812,#12813));
#3320=EDGE_LOOP('',(#12814,#12815,#12816,#12817));
#3321=EDGE_LOOP('',(#12818,#12819,#12820,#12821));
#3322=EDGE_LOOP('',(#12822,#12823,#12824,#12825));
#3323=EDGE_LOOP('',(#12826,#12827,#12828,#12829));
#3324=EDGE_LOOP('',(#12830,#12831,#12832));
#3325=EDGE_LOOP('',(#12833,#12834,#12835,#12836,#12837));
#3326=EDGE_LOOP('',(#12838,#12839,#12840,#12841));
#3327=EDGE_LOOP('',(#12842,#12843,#12844,#12845));
#3328=EDGE_LOOP('',(#12846,#12847,#12848,#12849));
#3329=EDGE_LOOP('',(#12850,#12851,#12852,#12853));
#3330=EDGE_LOOP('',(#12854,#12855,#12856,#12857,#12858));
#3331=EDGE_LOOP('',(#12859,#12860,#12861,#12862,#12863,#12864));
#3332=EDGE_LOOP('',(#12865));
#3333=EDGE_LOOP('',(#12866,#12867,#12868,#12869));
#3334=EDGE_LOOP('',(#12870,#12871,#12872,#12873,#12874,#12875));
#3335=EDGE_LOOP('',(#12876,#12877,#12878,#12879,#12880,#12881));
#3336=EDGE_LOOP('',(#12882,#12883,#12884,#12885,#12886));
#3337=EDGE_LOOP('',(#12887));
#3338=EDGE_LOOP('',(#12888,#12889,#12890,#12891,#12892,#12893));
#3339=EDGE_LOOP('',(#12894,#12895,#12896,#12897));
#3340=EDGE_LOOP('',(#12898,#12899,#12900,#12901));
#3341=EDGE_LOOP('',(#12902,#12903,#12904,#12905));
#3342=EDGE_LOOP('',(#12906,#12907,#12908,#12909));
#3343=EDGE_LOOP('',(#12910,#12911,#12912,#12913));
#3344=EDGE_LOOP('',(#12914,#12915,#12916,#12917));
#3345=EDGE_LOOP('',(#12918,#12919,#12920,#12921));
#3346=EDGE_LOOP('',(#12922,#12923,#12924,#12925));
#3347=EDGE_LOOP('',(#12926,#12927,#12928,#12929));
#3348=EDGE_LOOP('',(#12930,#12931,#12932,#12933,#12934,#12935));
#3349=EDGE_LOOP('',(#12936,#12937,#12938,#12939,#12940,#12941,#12942,#12943,
#12944,#12945,#12946,#12947,#12948,#12949,#12950));
#3350=EDGE_LOOP('',(#12951,#12952,#12953,#12954));
#3351=EDGE_LOOP('',(#12955,#12956,#12957,#12958,#12959,#12960,#12961,#12962,
#12963,#12964,#12965,#12966,#12967,#12968,#12969,#12970));
#3352=EDGE_LOOP('',(#12971,#12972,#12973,#12974));
#3353=EDGE_LOOP('',(#12975,#12976,#12977,#12978));
#3354=EDGE_LOOP('',(#12979,#12980,#12981,#12982));
#3355=EDGE_LOOP('',(#12983,#12984,#12985,#12986));
#3356=EDGE_LOOP('',(#12987,#12988,#12989,#12990,#12991,#12992));
#3357=EDGE_LOOP('',(#12993,#12994,#12995,#12996,#12997,#12998));
#3358=EDGE_LOOP('',(#12999));
#3359=EDGE_LOOP('',(#13000,#13001,#13002,#13003,#13004,#13005,#13006,#13007));
#3360=EDGE_LOOP('',(#13008));
#3361=EDGE_LOOP('',(#13009,#13010,#13011,#13012));
#3362=EDGE_LOOP('',(#13013,#13014,#13015,#13016));
#3363=EDGE_LOOP('',(#13017,#13018,#13019,#13020));
#3364=EDGE_LOOP('',(#13021,#13022,#13023,#13024));
#3365=EDGE_LOOP('',(#13025,#13026,#13027,#13028));
#3366=EDGE_LOOP('',(#13029,#13030,#13031,#13032));
#3367=EDGE_LOOP('',(#13033,#13034,#13035,#13036));
#3368=EDGE_LOOP('',(#13037,#13038,#13039,#13040));
#3369=EDGE_LOOP('',(#13041,#13042,#13043,#13044,#13045,#13046,#13047,#13048));
#3370=EDGE_LOOP('',(#13049,#13050,#13051,#13052,#13053,#13054));
#3371=EDGE_LOOP('',(#13055,#13056,#13057,#13058,#13059,#13060,#13061,#13062));
#3372=EDGE_LOOP('',(#13063));
#3373=EDGE_LOOP('',(#13064,#13065,#13066,#13067));
#3374=EDGE_LOOP('',(#13068,#13069));
#3375=EDGE_LOOP('',(#13070,#13071));
#3376=EDGE_LOOP('',(#13072,#13073));
#3377=EDGE_LOOP('',(#13074,#13075,#13076));
#3378=EDGE_LOOP('',(#13077,#13078));
#3379=EDGE_LOOP('',(#13079,#13080));
#3380=EDGE_LOOP('',(#13081,#13082,#13083,#13084,#13085,#13086,#13087,#13088,
#13089,#13090,#13091,#13092,#13093,#13094,#13095,#13096));
#3381=EDGE_LOOP('',(#13097,#13098,#13099,#13100));
#3382=EDGE_LOOP('',(#13101));
#3383=EDGE_LOOP('',(#13102));
#3384=EDGE_LOOP('',(#13103,#13104,#13105));
#3385=EDGE_LOOP('',(#13106,#13107,#13108));
#3386=EDGE_LOOP('',(#13109,#13110,#13111));
#3387=EDGE_LOOP('',(#13112,#13113,#13114));
#3388=EDGE_LOOP('',(#13115,#13116,#13117));
#3389=EDGE_LOOP('',(#13118,#13119,#13120,#13121,#13122,#13123));
#3390=EDGE_LOOP('',(#13124));
#3391=EDGE_LOOP('',(#13125,#13126,#13127,#13128,#13129,#13130));
#3392=EDGE_LOOP('',(#13131,#13132,#13133,#13134,#13135,#13136));
#3393=EDGE_LOOP('',(#13137,#13138,#13139,#13140,#13141,#13142,#13143,#13144,
#13145));
#3394=EDGE_LOOP('',(#13146,#13147,#13148,#13149,#13150,#13151));
#3395=EDGE_LOOP('',(#13152,#13153,#13154,#13155,#13156,#13157));
#3396=EDGE_LOOP('',(#13158,#13159,#13160));
#3397=EDGE_LOOP('',(#13161));
#3398=EDGE_LOOP('',(#13162,#13163,#13164,#13165));
#3399=EDGE_LOOP('',(#13166,#13167,#13168,#13169));
#3400=EDGE_LOOP('',(#13170,#13171,#13172));
#3401=EDGE_LOOP('',(#13173,#13174,#13175));
#3402=EDGE_LOOP('',(#13176,#13177,#13178));
#3403=EDGE_LOOP('',(#13179,#13180,#13181,#13182));
#3404=EDGE_LOOP('',(#13183,#13184,#13185));
#3405=EDGE_LOOP('',(#13186,#13187,#13188));
#3406=EDGE_LOOP('',(#13189,#13190,#13191));
#3407=EDGE_LOOP('',(#13192,#13193,#13194,#13195));
#3408=EDGE_LOOP('',(#13196,#13197,#13198,#13199));
#3409=EDGE_LOOP('',(#13200,#13201,#13202,#13203));
#3410=EDGE_LOOP('',(#13204,#13205,#13206,#13207));
#3411=EDGE_LOOP('',(#13208,#13209,#13210,#13211));
#3412=EDGE_LOOP('',(#13212,#13213,#13214,#13215));
#3413=EDGE_LOOP('',(#13216,#13217,#13218,#13219));
#3414=EDGE_LOOP('',(#13220,#13221,#13222,#13223));
#3415=EDGE_LOOP('',(#13224,#13225,#13226,#13227));
#3416=EDGE_LOOP('',(#13228,#13229,#13230,#13231));
#3417=EDGE_LOOP('',(#13232,#13233,#13234,#13235));
#3418=EDGE_LOOP('',(#13236,#13237,#13238,#13239));
#3419=EDGE_LOOP('',(#13240,#13241,#13242,#13243));
#3420=EDGE_LOOP('',(#13244,#13245,#13246,#13247));
#3421=EDGE_LOOP('',(#13248,#13249,#13250,#13251,#13252,#13253));
#3422=EDGE_LOOP('',(#13254));
#3423=EDGE_LOOP('',(#13255,#13256,#13257,#13258,#13259,#13260));
#3424=EDGE_LOOP('',(#13261,#13262,#13263,#13264,#13265,#13266));
#3425=EDGE_LOOP('',(#13267,#13268,#13269,#13270,#13271));
#3426=EDGE_LOOP('',(#13272,#13273,#13274,#13275,#13276));
#3427=EDGE_LOOP('',(#13277));
#3428=EDGE_LOOP('',(#13278,#13279,#13280,#13281,#13282));
#3429=EDGE_LOOP('',(#13283,#13284,#13285,#13286,#13287));
#3430=EDGE_LOOP('',(#13288));
#3431=EDGE_LOOP('',(#13289,#13290,#13291,#13292,#13293,#13294,#13295,#13296,
#13297,#13298,#13299,#13300));
#3432=EDGE_LOOP('',(#13301));
#3433=EDGE_LOOP('',(#13302));
#3434=EDGE_LOOP('',(#13303));
#3435=EDGE_LOOP('',(#13304));
#3436=EDGE_LOOP('',(#13305,#13306,#13307,#13308));
#3437=EDGE_LOOP('',(#13309,#13310,#13311,#13312));
#3438=EDGE_LOOP('',(#13313));
#3439=EDGE_LOOP('',(#13314));
#3440=EDGE_LOOP('',(#13315));
#3441=EDGE_LOOP('',(#13316));
#3442=EDGE_LOOP('',(#13317,#13318,#13319,#13320));
#3443=EDGE_LOOP('',(#13321,#13322,#13323,#13324));
#3444=EDGE_LOOP('',(#13325,#13326,#13327,#13328));
#3445=EDGE_LOOP('',(#13329,#13330,#13331,#13332));
#3446=EDGE_LOOP('',(#13333,#13334,#13335,#13336));
#3447=EDGE_LOOP('',(#13337,#13338,#13339,#13340));
#3448=EDGE_LOOP('',(#13341));
#3449=EDGE_LOOP('',(#13342,#13343));
#3450=EDGE_LOOP('',(#13344,#13345,#13346,#13347));
#3451=EDGE_LOOP('',(#13348));
#3452=EDGE_LOOP('',(#13349));
#3453=EDGE_LOOP('',(#13350,#13351,#13352,#13353));
#3454=EDGE_LOOP('',(#13354,#13355,#13356,#13357));
#3455=EDGE_LOOP('',(#13358,#13359,#13360,#13361));
#3456=EDGE_LOOP('',(#13362));
#3457=EDGE_LOOP('',(#13363));
#3458=EDGE_LOOP('',(#13364,#13365,#13366,#13367));
#3459=EDGE_LOOP('',(#13368,#13369,#13370,#13371));
#3460=EDGE_LOOP('',(#13372));
#3461=EDGE_LOOP('',(#13373));
#3462=EDGE_LOOP('',(#13374));
#3463=EDGE_LOOP('',(#13375));
#3464=EDGE_LOOP('',(#13376));
#3465=EDGE_LOOP('',(#13377));
#3466=EDGE_LOOP('',(#13378,#13379,#13380,#13381));
#3467=EDGE_LOOP('',(#13382,#13383,#13384,#13385));
#3468=EDGE_LOOP('',(#13386,#13387,#13388,#13389));
#3469=EDGE_LOOP('',(#13390,#13391,#13392,#13393));
#3470=EDGE_LOOP('',(#13394,#13395,#13396,#13397));
#3471=EDGE_LOOP('',(#13398,#13399,#13400,#13401));
#3472=EDGE_LOOP('',(#13402,#13403,#13404,#13405));
#3473=EDGE_LOOP('',(#13406,#13407,#13408,#13409));
#3474=EDGE_LOOP('',(#13410,#13411,#13412,#13413));
#3475=EDGE_LOOP('',(#13414,#13415,#13416,#13417));
#3476=EDGE_LOOP('',(#13418,#13419,#13420,#13421));
#3477=EDGE_LOOP('',(#13422,#13423,#13424,#13425));
#3478=EDGE_LOOP('',(#13426,#13427,#13428,#13429));
#3479=EDGE_LOOP('',(#13430,#13431,#13432,#13433));
#3480=EDGE_LOOP('',(#13434,#13435,#13436,#13437));
#3481=EDGE_LOOP('',(#13438,#13439,#13440,#13441));
#3482=EDGE_LOOP('',(#13442,#13443,#13444,#13445));
#3483=EDGE_LOOP('',(#13446,#13447,#13448,#13449));
#3484=EDGE_LOOP('',(#13450,#13451,#13452,#13453));
#3485=EDGE_LOOP('',(#13454,#13455,#13456,#13457));
#3486=EDGE_LOOP('',(#13458,#13459,#13460,#13461));
#3487=EDGE_LOOP('',(#13462,#13463,#13464,#13465));
#3488=EDGE_LOOP('',(#13466,#13467,#13468,#13469));
#3489=EDGE_LOOP('',(#13470,#13471,#13472,#13473));
#3490=EDGE_LOOP('',(#13474,#13475,#13476,#13477));
#3491=EDGE_LOOP('',(#13478,#13479,#13480,#13481));
#3492=EDGE_LOOP('',(#13482,#13483,#13484,#13485));
#3493=EDGE_LOOP('',(#13486));
#3494=EDGE_LOOP('',(#13487));
#3495=EDGE_LOOP('',(#13488));
#3496=EDGE_LOOP('',(#13489));
#3497=EDGE_LOOP('',(#13490));
#3498=EDGE_LOOP('',(#13491));
#3499=EDGE_LOOP('',(#13492,#13493,#13494,#13495,#13496,#13497,#13498,#13499,
#13500,#13501,#13502,#13503,#13504,#13505,#13506,#13507));
#3500=EDGE_LOOP('',(#13508,#13509,#13510,#13511));
#3501=EDGE_LOOP('',(#13512,#13513,#13514,#13515));
#3502=EDGE_LOOP('',(#13516,#13517,#13518,#13519));
#3503=EDGE_LOOP('',(#13520,#13521,#13522,#13523));
#3504=EDGE_LOOP('',(#13524,#13525,#13526,#13527));
#3505=EDGE_LOOP('',(#13528,#13529,#13530,#13531));
#3506=EDGE_LOOP('',(#13532,#13533,#13534,#13535));
#3507=EDGE_LOOP('',(#13536,#13537,#13538,#13539));
#3508=EDGE_LOOP('',(#13540,#13541,#13542,#13543));
#3509=EDGE_LOOP('',(#13544,#13545,#13546,#13547));
#3510=EDGE_LOOP('',(#13548,#13549,#13550,#13551));
#3511=EDGE_LOOP('',(#13552,#13553,#13554,#13555));
#3512=EDGE_LOOP('',(#13556,#13557,#13558,#13559));
#3513=EDGE_LOOP('',(#13560,#13561,#13562,#13563));
#3514=EDGE_LOOP('',(#13564,#13565,#13566,#13567));
#3515=EDGE_LOOP('',(#13568,#13569,#13570,#13571));
#3516=EDGE_LOOP('',(#13572,#13573,#13574,#13575));
#3517=EDGE_LOOP('',(#13576,#13577,#13578,#13579));
#3518=EDGE_LOOP('',(#13580,#13581,#13582,#13583));
#3519=EDGE_LOOP('',(#13584,#13585,#13586,#13587));
#3520=EDGE_LOOP('',(#13588,#13589,#13590,#13591));
#3521=EDGE_LOOP('',(#13592,#13593,#13594,#13595));
#3522=EDGE_LOOP('',(#13596,#13597,#13598,#13599));
#3523=EDGE_LOOP('',(#13600,#13601,#13602,#13603,#13604,#13605,#13606,#13607,
#13608,#13609,#13610,#13611,#13612,#13613,#13614,#13615));
#3524=EDGE_LOOP('',(#13616,#13617,#13618,#13619));
#3525=EDGE_LOOP('',(#13620,#13621,#13622,#13623));
#3526=EDGE_LOOP('',(#13624,#13625,#13626,#13627));
#3527=EDGE_LOOP('',(#13628,#13629,#13630,#13631));
#3528=EDGE_LOOP('',(#13632,#13633,#13634,#13635));
#3529=EDGE_LOOP('',(#13636,#13637,#13638,#13639));
#3530=EDGE_LOOP('',(#13640,#13641,#13642,#13643));
#3531=EDGE_LOOP('',(#13644,#13645,#13646,#13647));
#3532=EDGE_LOOP('',(#13648,#13649,#13650,#13651));
#3533=EDGE_LOOP('',(#13652,#13653,#13654,#13655));
#3534=EDGE_LOOP('',(#13656,#13657,#13658,#13659));
#3535=EDGE_LOOP('',(#13660,#13661,#13662,#13663));
#3536=EDGE_LOOP('',(#13664,#13665,#13666,#13667));
#3537=EDGE_LOOP('',(#13668,#13669,#13670,#13671));
#3538=EDGE_LOOP('',(#13672,#13673,#13674,#13675));
#3539=EDGE_LOOP('',(#13676,#13677,#13678,#13679,#13680));
#3540=EDGE_LOOP('',(#13681,#13682,#13683,#13684));
#3541=EDGE_LOOP('',(#13685,#13686,#13687,#13688));
#3542=EDGE_LOOP('',(#13689,#13690,#13691,#13692));
#3543=EDGE_LOOP('',(#13693,#13694,#13695,#13696));
#3544=EDGE_LOOP('',(#13697,#13698,#13699,#13700));
#3545=EDGE_LOOP('',(#13701,#13702,#13703,#13704));
#3546=EDGE_LOOP('',(#13705,#13706,#13707,#13708));
#3547=EDGE_LOOP('',(#13709,#13710,#13711,#13712));
#3548=EDGE_LOOP('',(#13713,#13714,#13715,#13716));
#3549=EDGE_LOOP('',(#13717,#13718,#13719,#13720,#13721,#13722));
#3550=EDGE_LOOP('',(#13723,#13724,#13725,#13726,#13727,#13728));
#3551=EDGE_LOOP('',(#13729,#13730,#13731,#13732,#13733));
#3552=EDGE_LOOP('',(#13734,#13735,#13736,#13737,#13738));
#3553=EDGE_LOOP('',(#13739));
#3554=EDGE_LOOP('',(#13740,#13741,#13742,#13743));
#3555=EDGE_LOOP('',(#13744,#13745,#13746,#13747,#13748,#13749,#13750,#13751,
#13752,#13753,#13754,#13755,#13756,#13757,#13758,#13759,#13760,#13761,#13762,
#13763,#13764,#13765,#13766));
#3556=EDGE_LOOP('',(#13767,#13768,#13769,#13770));
#3557=EDGE_LOOP('',(#13771,#13772,#13773,#13774,#13775,#13776,#13777,#13778,
#13779,#13780,#13781,#13782,#13783,#13784,#13785,#13786,#13787,#13788,#13789,
#13790,#13791,#13792));
#3558=EDGE_LOOP('',(#13793,#13794,#13795));
#3559=EDGE_LOOP('',(#13796,#13797,#13798,#13799));
#3560=EDGE_LOOP('',(#13800));
#3561=EDGE_LOOP('',(#13801,#13802,#13803,#13804));
#3562=EDGE_LOOP('',(#13805,#13806,#13807,#13808,#13809,#13810));
#3563=EDGE_LOOP('',(#13811));
#3564=EDGE_LOOP('',(#13812,#13813,#13814,#13815));
#3565=EDGE_LOOP('',(#13816,#13817,#13818,#13819));
#3566=EDGE_LOOP('',(#13820,#13821,#13822,#13823));
#3567=EDGE_LOOP('',(#13824,#13825,#13826,#13827));
#3568=EDGE_LOOP('',(#13828,#13829,#13830,#13831));
#3569=EDGE_LOOP('',(#13832,#13833,#13834,#13835));
#3570=EDGE_LOOP('',(#13836,#13837,#13838,#13839));
#3571=EDGE_LOOP('',(#13840,#13841,#13842,#13843));
#3572=EDGE_LOOP('',(#13844,#13845,#13846,#13847));
#3573=EDGE_LOOP('',(#13848,#13849,#13850,#13851));
#3574=EDGE_LOOP('',(#13852,#13853,#13854,#13855));
#3575=EDGE_LOOP('',(#13856,#13857,#13858,#13859));
#3576=EDGE_LOOP('',(#13860,#13861,#13862,#13863));
#3577=EDGE_LOOP('',(#13864,#13865,#13866,#13867));
#3578=EDGE_LOOP('',(#13868,#13869,#13870,#13871));
#3579=EDGE_LOOP('',(#13872,#13873,#13874,#13875));
#3580=EDGE_LOOP('',(#13876,#13877,#13878,#13879));
#3581=EDGE_LOOP('',(#13880,#13881,#13882,#13883));
#3582=EDGE_LOOP('',(#13884,#13885,#13886,#13887));
#3583=EDGE_LOOP('',(#13888,#13889,#13890,#13891));
#3584=EDGE_LOOP('',(#13892,#13893,#13894,#13895));
#3585=EDGE_LOOP('',(#13896,#13897,#13898,#13899));
#3586=EDGE_LOOP('',(#13900,#13901,#13902,#13903));
#3587=EDGE_LOOP('',(#13904,#13905,#13906,#13907));
#3588=EDGE_LOOP('',(#13908,#13909,#13910,#13911));
#3589=EDGE_LOOP('',(#13912,#13913,#13914,#13915));
#3590=EDGE_LOOP('',(#13916,#13917,#13918,#13919));
#3591=EDGE_LOOP('',(#13920,#13921,#13922,#13923));
#3592=EDGE_LOOP('',(#13924,#13925,#13926,#13927));
#3593=EDGE_LOOP('',(#13928,#13929,#13930,#13931));
#3594=EDGE_LOOP('',(#13932,#13933,#13934,#13935));
#3595=EDGE_LOOP('',(#13936,#13937,#13938,#13939));
#3596=EDGE_LOOP('',(#13940,#13941,#13942,#13943));
#3597=EDGE_LOOP('',(#13944,#13945,#13946,#13947));
#3598=EDGE_LOOP('',(#13948,#13949,#13950,#13951));
#3599=EDGE_LOOP('',(#13952,#13953,#13954,#13955));
#3600=EDGE_LOOP('',(#13956,#13957,#13958,#13959));
#3601=EDGE_LOOP('',(#13960,#13961,#13962,#13963));
#3602=EDGE_LOOP('',(#13964,#13965,#13966,#13967));
#3603=EDGE_LOOP('',(#13968,#13969,#13970,#13971));
#3604=EDGE_LOOP('',(#13972,#13973,#13974,#13975));
#3605=EDGE_LOOP('',(#13976,#13977,#13978,#13979));
#3606=EDGE_LOOP('',(#13980,#13981,#13982,#13983));
#3607=EDGE_LOOP('',(#13984,#13985,#13986,#13987));
#3608=EDGE_LOOP('',(#13988,#13989,#13990));
#3609=EDGE_LOOP('',(#13991,#13992,#13993,#13994,#13995));
#3610=EDGE_LOOP('',(#13996,#13997,#13998,#13999));
#3611=EDGE_LOOP('',(#14000,#14001,#14002,#14003));
#3612=EDGE_LOOP('',(#14004,#14005,#14006,#14007));
#3613=EDGE_LOOP('',(#14008,#14009,#14010,#14011));
#3614=EDGE_LOOP('',(#14012,#14013,#14014,#14015));
#3615=EDGE_LOOP('',(#14016,#14017,#14018,#14019));
#3616=EDGE_LOOP('',(#14020,#14021,#14022,#14023));
#3617=EDGE_LOOP('',(#14024,#14025,#14026,#14027));
#3618=EDGE_LOOP('',(#14028,#14029,#14030,#14031));
#3619=EDGE_LOOP('',(#14032,#14033,#14034,#14035));
#3620=EDGE_LOOP('',(#14036,#14037,#14038,#14039));
#3621=EDGE_LOOP('',(#14040,#14041,#14042,#14043));
#3622=EDGE_LOOP('',(#14044,#14045,#14046,#14047));
#3623=EDGE_LOOP('',(#14048,#14049,#14050,#14051));
#3624=EDGE_LOOP('',(#14052,#14053,#14054,#14055));
#3625=EDGE_LOOP('',(#14056,#14057,#14058,#14059));
#3626=EDGE_LOOP('',(#14060,#14061,#14062,#14063));
#3627=EDGE_LOOP('',(#14064,#14065,#14066,#14067));
#3628=EDGE_LOOP('',(#14068,#14069,#14070,#14071));
#3629=EDGE_LOOP('',(#14072,#14073,#14074,#14075));
#3630=EDGE_LOOP('',(#14076,#14077,#14078,#14079));
#3631=EDGE_LOOP('',(#14080,#14081,#14082,#14083));
#3632=EDGE_LOOP('',(#14084,#14085,#14086,#14087));
#3633=EDGE_LOOP('',(#14088,#14089,#14090,#14091));
#3634=EDGE_LOOP('',(#14092,#14093,#14094,#14095));
#3635=EDGE_LOOP('',(#14096,#14097,#14098,#14099));
#3636=EDGE_LOOP('',(#14100,#14101,#14102,#14103));
#3637=EDGE_LOOP('',(#14104,#14105,#14106,#14107));
#3638=EDGE_LOOP('',(#14108,#14109,#14110,#14111));
#3639=EDGE_LOOP('',(#14112,#14113,#14114,#14115));
#3640=EDGE_LOOP('',(#14116,#14117,#14118,#14119));
#3641=EDGE_LOOP('',(#14120,#14121,#14122,#14123));
#3642=EDGE_LOOP('',(#14124,#14125,#14126,#14127));
#3643=EDGE_LOOP('',(#14128,#14129,#14130,#14131));
#3644=EDGE_LOOP('',(#14132,#14133,#14134,#14135));
#3645=EDGE_LOOP('',(#14136,#14137,#14138,#14139));
#3646=EDGE_LOOP('',(#14140,#14141,#14142,#14143));
#3647=EDGE_LOOP('',(#14144,#14145,#14146,#14147));
#3648=EDGE_LOOP('',(#14148,#14149,#14150,#14151));
#3649=EDGE_LOOP('',(#14152,#14153,#14154,#14155));
#3650=EDGE_LOOP('',(#14156,#14157,#14158,#14159));
#3651=EDGE_LOOP('',(#14160,#14161,#14162,#14163));
#3652=EDGE_LOOP('',(#14164,#14165,#14166,#14167,#14168,#14169,#14170,#14171,
#14172,#14173,#14174,#14175,#14176,#14177,#14178,#14179,#14180,#14181,#14182,
#14183,#14184,#14185,#14186,#14187,#14188,#14189,#14190,#14191,#14192,#14193,
#14194,#14195,#14196,#14197,#14198,#14199,#14200,#14201,#14202,#14203,#14204,
#14205,#14206,#14207,#14208,#14209,#14210,#14211,#14212,#14213,#14214,#14215,
#14216,#14217,#14218,#14219,#14220,#14221,#14222,#14223,#14224,#14225,#14226,
#14227,#14228,#14229,#14230,#14231,#14232,#14233,#14234,#14235,#14236,#14237,
#14238,#14239,#14240,#14241,#14242,#14243,#14244,#14245,#14246,#14247,#14248,
#14249,#14250,#14251,#14252,#14253,#14254));
#3653=EDGE_LOOP('',(#14255,#14256,#14257,#14258,#14259));
#3654=EDGE_LOOP('',(#14260,#14261,#14262,#14263));
#3655=EDGE_LOOP('',(#14264,#14265,#14266,#14267,#14268,#14269,#14270,#14271,
#14272,#14273,#14274,#14275,#14276,#14277,#14278,#14279,#14280,#14281,#14282,
#14283,#14284,#14285,#14286,#14287,#14288,#14289,#14290,#14291,#14292,#14293,
#14294,#14295,#14296,#14297,#14298,#14299,#14300,#14301,#14302,#14303,#14304,
#14305,#14306,#14307,#14308,#14309,#14310,#14311,#14312,#14313,#14314,#14315,
#14316,#14317,#14318,#14319,#14320,#14321,#14322,#14323,#14324,#14325,#14326,
#14327,#14328,#14329,#14330,#14331,#14332,#14333,#14334,#14335,#14336,#14337,
#14338,#14339,#14340,#14341,#14342,#14343,#14344,#14345,#14346,#14347,#14348,
#14349,#14350,#14351,#14352,#14353,#14354,#14355));
#3656=EDGE_LOOP('',(#14356,#14357,#14358,#14359,#14360,#14361,#14362,#14363,
#14364,#14365));
#3657=EDGE_LOOP('',(#14366,#14367,#14368,#14369));
#3658=EDGE_LOOP('',(#14370,#14371,#14372,#14373));
#3659=EDGE_LOOP('',(#14374,#14375,#14376,#14377));
#3660=EDGE_LOOP('',(#14378,#14379,#14380,#14381,#14382,#14383));
#3661=EDGE_LOOP('',(#14384,#14385,#14386,#14387,#14388));
#3662=EDGE_LOOP('',(#14389,#14390,#14391,#14392));
#3663=EDGE_LOOP('',(#14393,#14394,#14395,#14396));
#3664=EDGE_LOOP('',(#14397,#14398,#14399,#14400,#14401));
#3665=EDGE_LOOP('',(#14402));
#3666=EDGE_LOOP('',(#14403));
#3667=EDGE_LOOP('',(#14404,#14405,#14406,#14407,#14408,#14409));
#3668=EDGE_LOOP('',(#14410,#14411,#14412,#14413));
#3669=EDGE_LOOP('',(#14414,#14415,#14416,#14417));
#3670=EDGE_LOOP('',(#14418,#14419,#14420,#14421));
#3671=EDGE_LOOP('',(#14422,#14423,#14424,#14425));
#3672=EDGE_LOOP('',(#14426,#14427,#14428,#14429));
#3673=EDGE_LOOP('',(#14430,#14431,#14432,#14433));
#3674=EDGE_LOOP('',(#14434,#14435,#14436,#14437));
#3675=EDGE_LOOP('',(#14438,#14439,#14440,#14441));
#3676=EDGE_LOOP('',(#14442,#14443,#14444,#14445));
#3677=EDGE_LOOP('',(#14446,#14447,#14448,#14449));
#3678=EDGE_LOOP('',(#14450,#14451,#14452,#14453));
#3679=EDGE_LOOP('',(#14454,#14455,#14456,#14457));
#3680=EDGE_LOOP('',(#14458,#14459,#14460,#14461));
#3681=EDGE_LOOP('',(#14462,#14463,#14464,#14465));
#3682=EDGE_LOOP('',(#14466,#14467,#14468,#14469));
#3683=EDGE_LOOP('',(#14470,#14471,#14472,#14473));
#3684=EDGE_LOOP('',(#14474,#14475,#14476,#14477));
#3685=EDGE_LOOP('',(#14478,#14479,#14480,#14481));
#3686=EDGE_LOOP('',(#14482,#14483,#14484,#14485));
#3687=EDGE_LOOP('',(#14486,#14487,#14488,#14489));
#3688=EDGE_LOOP('',(#14490,#14491,#14492,#14493));
#3689=EDGE_LOOP('',(#14494,#14495,#14496,#14497));
#3690=EDGE_LOOP('',(#14498,#14499,#14500,#14501));
#3691=EDGE_LOOP('',(#14502,#14503,#14504,#14505));
#3692=EDGE_LOOP('',(#14506,#14507,#14508,#14509));
#3693=EDGE_LOOP('',(#14510,#14511,#14512,#14513));
#3694=EDGE_LOOP('',(#14514,#14515,#14516,#14517));
#3695=EDGE_LOOP('',(#14518,#14519,#14520,#14521));
#3696=EDGE_LOOP('',(#14522,#14523,#14524,#14525));
#3697=EDGE_LOOP('',(#14526,#14527,#14528,#14529));
#3698=EDGE_LOOP('',(#14530,#14531,#14532,#14533));
#3699=EDGE_LOOP('',(#14534,#14535,#14536,#14537));
#3700=EDGE_LOOP('',(#14538,#14539,#14540,#14541));
#3701=EDGE_LOOP('',(#14542,#14543,#14544,#14545));
#3702=EDGE_LOOP('',(#14546,#14547,#14548,#14549));
#3703=EDGE_LOOP('',(#14550,#14551,#14552,#14553));
#3704=EDGE_LOOP('',(#14554,#14555,#14556,#14557));
#3705=EDGE_LOOP('',(#14558,#14559,#14560,#14561));
#3706=EDGE_LOOP('',(#14562,#14563,#14564,#14565));
#3707=EDGE_LOOP('',(#14566,#14567,#14568,#14569));
#3708=EDGE_LOOP('',(#14570,#14571,#14572,#14573));
#3709=EDGE_LOOP('',(#14574,#14575,#14576,#14577));
#3710=EDGE_LOOP('',(#14578,#14579,#14580,#14581));
#3711=EDGE_LOOP('',(#14582,#14583,#14584,#14585));
#3712=EDGE_LOOP('',(#14586,#14587,#14588,#14589));
#3713=EDGE_LOOP('',(#14590,#14591,#14592,#14593));
#3714=EDGE_LOOP('',(#14594,#14595,#14596,#14597));
#3715=EDGE_LOOP('',(#14598,#14599,#14600,#14601));
#3716=EDGE_LOOP('',(#14602,#14603,#14604,#14605));
#3717=EDGE_LOOP('',(#14606,#14607,#14608,#14609));
#3718=EDGE_LOOP('',(#14610,#14611,#14612,#14613));
#3719=EDGE_LOOP('',(#14614,#14615,#14616,#14617));
#3720=EDGE_LOOP('',(#14618,#14619,#14620,#14621));
#3721=EDGE_LOOP('',(#14622,#14623,#14624,#14625));
#3722=EDGE_LOOP('',(#14626,#14627,#14628,#14629));
#3723=EDGE_LOOP('',(#14630,#14631,#14632,#14633));
#3724=EDGE_LOOP('',(#14634,#14635,#14636,#14637));
#3725=EDGE_LOOP('',(#14638,#14639,#14640,#14641));
#3726=EDGE_LOOP('',(#14642,#14643,#14644,#14645));
#3727=EDGE_LOOP('',(#14646,#14647,#14648,#14649));
#3728=EDGE_LOOP('',(#14650,#14651,#14652,#14653));
#3729=EDGE_LOOP('',(#14654,#14655,#14656,#14657));
#3730=EDGE_LOOP('',(#14658,#14659,#14660,#14661));
#3731=EDGE_LOOP('',(#14662,#14663,#14664,#14665));
#3732=EDGE_LOOP('',(#14666,#14667,#14668,#14669));
#3733=EDGE_LOOP('',(#14670,#14671,#14672,#14673));
#3734=EDGE_LOOP('',(#14674,#14675,#14676,#14677));
#3735=EDGE_LOOP('',(#14678,#14679,#14680,#14681));
#3736=EDGE_LOOP('',(#14682,#14683,#14684,#14685));
#3737=EDGE_LOOP('',(#14686,#14687,#14688,#14689));
#3738=EDGE_LOOP('',(#14690,#14691,#14692,#14693));
#3739=EDGE_LOOP('',(#14694,#14695,#14696,#14697));
#3740=EDGE_LOOP('',(#14698,#14699,#14700,#14701));
#3741=EDGE_LOOP('',(#14702,#14703,#14704,#14705));
#3742=EDGE_LOOP('',(#14706,#14707,#14708,#14709));
#3743=EDGE_LOOP('',(#14710,#14711,#14712,#14713));
#3744=EDGE_LOOP('',(#14714,#14715,#14716,#14717));
#3745=EDGE_LOOP('',(#14718,#14719,#14720,#14721));
#3746=EDGE_LOOP('',(#14722,#14723,#14724,#14725));
#3747=EDGE_LOOP('',(#14726,#14727,#14728,#14729));
#3748=EDGE_LOOP('',(#14730,#14731,#14732,#14733));
#3749=EDGE_LOOP('',(#14734,#14735,#14736,#14737));
#3750=EDGE_LOOP('',(#14738,#14739,#14740,#14741));
#3751=EDGE_LOOP('',(#14742,#14743,#14744,#14745));
#3752=EDGE_LOOP('',(#14746,#14747,#14748,#14749));
#3753=EDGE_LOOP('',(#14750,#14751,#14752,#14753));
#3754=EDGE_LOOP('',(#14754,#14755,#14756,#14757));
#3755=EDGE_LOOP('',(#14758,#14759,#14760,#14761));
#3756=EDGE_LOOP('',(#14762,#14763,#14764,#14765));
#3757=EDGE_LOOP('',(#14766,#14767,#14768));
#3758=EDGE_LOOP('',(#14769,#14770,#14771,#14772,#14773));
#3759=EDGE_LOOP('',(#14774,#14775,#14776,#14777));
#3760=EDGE_LOOP('',(#14778,#14779,#14780,#14781));
#3761=EDGE_LOOP('',(#14782,#14783,#14784,#14785));
#3762=EDGE_LOOP('',(#14786,#14787,#14788,#14789));
#3763=EDGE_LOOP('',(#14790,#14791,#14792,#14793));
#3764=EDGE_LOOP('',(#14794,#14795,#14796,#14797));
#3765=EDGE_LOOP('',(#14798,#14799,#14800,#14801));
#3766=EDGE_LOOP('',(#14802,#14803,#14804,#14805));
#3767=EDGE_LOOP('',(#14806,#14807,#14808,#14809));
#3768=EDGE_LOOP('',(#14810,#14811,#14812,#14813));
#3769=EDGE_LOOP('',(#14814,#14815,#14816,#14817));
#3770=EDGE_LOOP('',(#14818,#14819,#14820,#14821));
#3771=EDGE_LOOP('',(#14822,#14823,#14824,#14825));
#3772=EDGE_LOOP('',(#14826,#14827,#14828,#14829));
#3773=EDGE_LOOP('',(#14830,#14831,#14832,#14833));
#3774=EDGE_LOOP('',(#14834,#14835,#14836,#14837));
#3775=EDGE_LOOP('',(#14838,#14839,#14840,#14841));
#3776=EDGE_LOOP('',(#14842,#14843,#14844,#14845));
#3777=EDGE_LOOP('',(#14846,#14847,#14848,#14849));
#3778=EDGE_LOOP('',(#14850,#14851,#14852,#14853));
#3779=EDGE_LOOP('',(#14854,#14855,#14856,#14857));
#3780=EDGE_LOOP('',(#14858,#14859,#14860,#14861));
#3781=EDGE_LOOP('',(#14862,#14863,#14864,#14865));
#3782=EDGE_LOOP('',(#14866,#14867,#14868,#14869));
#3783=EDGE_LOOP('',(#14870,#14871,#14872,#14873));
#3784=EDGE_LOOP('',(#14874,#14875,#14876,#14877));
#3785=EDGE_LOOP('',(#14878,#14879,#14880,#14881));
#3786=EDGE_LOOP('',(#14882,#14883,#14884,#14885));
#3787=EDGE_LOOP('',(#14886,#14887,#14888,#14889));
#3788=EDGE_LOOP('',(#14890,#14891,#14892,#14893));
#3789=EDGE_LOOP('',(#14894,#14895,#14896,#14897));
#3790=EDGE_LOOP('',(#14898,#14899,#14900,#14901));
#3791=EDGE_LOOP('',(#14902,#14903,#14904,#14905));
#3792=EDGE_LOOP('',(#14906,#14907,#14908,#14909));
#3793=EDGE_LOOP('',(#14910,#14911,#14912,#14913));
#3794=EDGE_LOOP('',(#14914,#14915,#14916,#14917));
#3795=EDGE_LOOP('',(#14918,#14919,#14920,#14921));
#3796=EDGE_LOOP('',(#14922,#14923,#14924,#14925));
#3797=EDGE_LOOP('',(#14926,#14927,#14928,#14929));
#3798=EDGE_LOOP('',(#14930,#14931,#14932,#14933));
#3799=EDGE_LOOP('',(#14934,#14935,#14936,#14937));
#3800=EDGE_LOOP('',(#14938,#14939,#14940,#14941));
#3801=EDGE_LOOP('',(#14942,#14943,#14944,#14945));
#3802=EDGE_LOOP('',(#14946,#14947,#14948,#14949));
#3803=EDGE_LOOP('',(#14950,#14951,#14952,#14953));
#3804=EDGE_LOOP('',(#14954,#14955,#14956,#14957));
#3805=EDGE_LOOP('',(#14958,#14959,#14960,#14961));
#3806=EDGE_LOOP('',(#14962,#14963,#14964,#14965));
#3807=EDGE_LOOP('',(#14966,#14967,#14968,#14969));
#3808=EDGE_LOOP('',(#14970,#14971,#14972,#14973));
#3809=EDGE_LOOP('',(#14974,#14975,#14976,#14977));
#3810=EDGE_LOOP('',(#14978,#14979,#14980,#14981));
#3811=EDGE_LOOP('',(#14982,#14983,#14984,#14985));
#3812=EDGE_LOOP('',(#14986,#14987,#14988,#14989));
#3813=EDGE_LOOP('',(#14990,#14991,#14992,#14993));
#3814=EDGE_LOOP('',(#14994,#14995,#14996,#14997));
#3815=EDGE_LOOP('',(#14998,#14999,#15000,#15001));
#3816=EDGE_LOOP('',(#15002,#15003,#15004,#15005));
#3817=EDGE_LOOP('',(#15006,#15007,#15008,#15009));
#3818=EDGE_LOOP('',(#15010,#15011,#15012,#15013));
#3819=EDGE_LOOP('',(#15014,#15015,#15016,#15017));
#3820=EDGE_LOOP('',(#15018,#15019,#15020,#15021));
#3821=EDGE_LOOP('',(#15022,#15023,#15024,#15025));
#3822=EDGE_LOOP('',(#15026,#15027,#15028,#15029));
#3823=EDGE_LOOP('',(#15030,#15031,#15032,#15033));
#3824=EDGE_LOOP('',(#15034,#15035,#15036,#15037));
#3825=EDGE_LOOP('',(#15038,#15039,#15040,#15041));
#3826=EDGE_LOOP('',(#15042,#15043,#15044,#15045));
#3827=EDGE_LOOP('',(#15046,#15047,#15048,#15049));
#3828=EDGE_LOOP('',(#15050,#15051,#15052,#15053));
#3829=EDGE_LOOP('',(#15054,#15055,#15056,#15057));
#3830=EDGE_LOOP('',(#15058,#15059,#15060,#15061));
#3831=EDGE_LOOP('',(#15062,#15063,#15064,#15065));
#3832=EDGE_LOOP('',(#15066,#15067,#15068,#15069));
#3833=EDGE_LOOP('',(#15070,#15071,#15072,#15073));
#3834=EDGE_LOOP('',(#15074,#15075,#15076,#15077));
#3835=EDGE_LOOP('',(#15078,#15079,#15080,#15081));
#3836=EDGE_LOOP('',(#15082,#15083,#15084,#15085));
#3837=EDGE_LOOP('',(#15086,#15087,#15088,#15089));
#3838=EDGE_LOOP('',(#15090,#15091,#15092,#15093));
#3839=EDGE_LOOP('',(#15094,#15095,#15096,#15097));
#3840=EDGE_LOOP('',(#15098,#15099,#15100,#15101));
#3841=EDGE_LOOP('',(#15102,#15103,#15104,#15105));
#3842=EDGE_LOOP('',(#15106,#15107,#15108,#15109));
#3843=EDGE_LOOP('',(#15110,#15111,#15112,#15113));
#3844=EDGE_LOOP('',(#15114,#15115,#15116,#15117));
#3845=EDGE_LOOP('',(#15118,#15119,#15120,#15121,#15122,#15123,#15124,#15125,
#15126,#15127,#15128,#15129,#15130,#15131,#15132,#15133,#15134,#15135,#15136,
#15137,#15138,#15139,#15140,#15141,#15142,#15143,#15144,#15145,#15146,#15147,
#15148,#15149,#15150,#15151,#15152,#15153,#15154,#15155,#15156,#15157,#15158,
#15159,#15160,#15161,#15162,#15163,#15164,#15165,#15166,#15167,#15168,#15169,
#15170,#15171,#15172,#15173,#15174,#15175,#15176,#15177,#15178,#15179,#15180,
#15181,#15182,#15183,#15184,#15185,#15186,#15187,#15188,#15189,#15190,#15191,
#15192,#15193,#15194,#15195,#15196,#15197,#15198,#15199,#15200,#15201,#15202,
#15203,#15204,#15205,#15206,#15207,#15208,#15209,#15210,#15211,#15212,#15213,
#15214,#15215,#15216,#15217,#15218,#15219,#15220,#15221,#15222,#15223,#15224,
#15225,#15226,#15227,#15228,#15229,#15230,#15231,#15232,#15233,#15234,#15235,
#15236,#15237,#15238,#15239,#15240,#15241,#15242,#15243,#15244,#15245,#15246,
#15247,#15248,#15249,#15250,#15251,#15252,#15253,#15254,#15255,#15256,#15257,
#15258,#15259,#15260,#15261,#15262,#15263,#15264,#15265,#15266,#15267,#15268,
#15269,#15270,#15271,#15272,#15273,#15274,#15275,#15276,#15277,#15278,#15279,
#15280,#15281,#15282,#15283,#15284,#15285,#15286,#15287,#15288,#15289,#15290,
#15291,#15292,#15293,#15294,#15295,#15296));
#3846=EDGE_LOOP('',(#15297,#15298,#15299,#15300,#15301));
#3847=EDGE_LOOP('',(#15302,#15303,#15304,#15305));
#3848=EDGE_LOOP('',(#15306,#15307,#15308,#15309,#15310,#15311,#15312,#15313,
#15314,#15315,#15316,#15317,#15318,#15319,#15320,#15321,#15322,#15323,#15324,
#15325,#15326,#15327,#15328,#15329,#15330,#15331,#15332,#15333,#15334,#15335,
#15336,#15337,#15338,#15339,#15340,#15341,#15342,#15343,#15344,#15345,#15346,
#15347,#15348,#15349,#15350,#15351,#15352,#15353,#15354,#15355,#15356,#15357,
#15358,#15359,#15360,#15361,#15362,#15363,#15364,#15365,#15366,#15367,#15368,
#15369,#15370,#15371,#15372,#15373,#15374,#15375,#15376,#15377,#15378,#15379,
#15380,#15381,#15382,#15383,#15384,#15385,#15386,#15387,#15388,#15389,#15390,
#15391,#15392,#15393,#15394,#15395,#15396,#15397,#15398,#15399,#15400,#15401,
#15402,#15403,#15404,#15405,#15406,#15407,#15408,#15409,#15410,#15411,#15412,
#15413,#15414,#15415,#15416,#15417,#15418,#15419,#15420,#15421,#15422,#15423,
#15424,#15425,#15426,#15427,#15428,#15429,#15430,#15431,#15432,#15433,#15434,
#15435,#15436,#15437,#15438,#15439,#15440,#15441,#15442,#15443,#15444,#15445,
#15446,#15447,#15448,#15449,#15450,#15451,#15452,#15453,#15454,#15455,#15456,
#15457,#15458,#15459,#15460,#15461,#15462,#15463,#15464,#15465,#15466,#15467,
#15468,#15469,#15470,#15471,#15472,#15473,#15474,#15475,#15476,#15477,#15478,
#15479,#15480,#15481,#15482,#15483,#15484,#15485));
#3849=EDGE_LOOP('',(#15486,#15487,#15488,#15489,#15490,#15491,#15492,#15493,
#15494,#15495));
#3850=EDGE_LOOP('',(#15496,#15497,#15498,#15499));
#3851=EDGE_LOOP('',(#15500,#15501,#15502,#15503));
#3852=EDGE_LOOP('',(#15504,#15505,#15506,#15507));
#3853=EDGE_LOOP('',(#15508,#15509,#15510,#15511,#15512,#15513));
#3854=EDGE_LOOP('',(#15514,#15515,#15516,#15517,#15518));
#3855=EDGE_LOOP('',(#15519,#15520,#15521,#15522));
#3856=EDGE_LOOP('',(#15523,#15524,#15525,#15526));
#3857=EDGE_LOOP('',(#15527,#15528,#15529,#15530,#15531));
#3858=EDGE_LOOP('',(#15532));
#3859=EDGE_LOOP('',(#15533));
#3860=EDGE_LOOP('',(#15534,#15535,#15536,#15537,#15538,#15539));
#3861=EDGE_LOOP('',(#15540,#15541,#15542,#15543));
#3862=EDGE_LOOP('',(#15544,#15545,#15546,#15547,#15548,#15549,#15550,#15551,
#15552,#15553,#15554,#15555,#15556,#15557,#15558,#15559));
#3863=EDGE_LOOP('',(#15560,#15561,#15562,#15563,#15564,#15565));
#3864=EDGE_LOOP('',(#15566,#15567,#15568,#15569,#15570,#15571));
#3865=EDGE_LOOP('',(#15572,#15573,#15574));
#3866=EDGE_LOOP('',(#15575,#15576,#15577));
#3867=EDGE_LOOP('',(#15578,#15579,#15580));
#3868=EDGE_LOOP('',(#15581,#15582,#15583));
#3869=EDGE_LOOP('',(#15584,#15585,#15586));
#3870=EDGE_LOOP('',(#15587,#15588,#15589));
#3871=EDGE_LOOP('',(#15590,#15591,#15592,#15593,#15594,#15595));
#3872=EDGE_LOOP('',(#15596));
#3873=EDGE_LOOP('',(#15597));
#3874=EDGE_LOOP('',(#15598,#15599,#15600));
#3875=EDGE_LOOP('',(#15601,#15602,#15603));
#3876=EDGE_LOOP('',(#15604,#15605,#15606));
#3877=EDGE_LOOP('',(#15607,#15608,#15609));
#3878=EDGE_LOOP('',(#15610,#15611,#15612));
#3879=EDGE_LOOP('',(#15613,#15614,#15615));
#3880=EDGE_LOOP('',(#15616,#15617,#15618,#15619,#15620,#15621));
#3881=EDGE_LOOP('',(#15622,#15623,#15624,#15625));
#3882=EDGE_LOOP('',(#15626,#15627,#15628,#15629,#15630,#15631,#15632));
#3883=EDGE_LOOP('',(#15633,#15634,#15635,#15636));
#3884=EDGE_LOOP('',(#15637,#15638,#15639,#15640));
#3885=EDGE_LOOP('',(#15641,#15642,#15643,#15644,#15645,#15646));
#3886=EDGE_LOOP('',(#15647,#15648,#15649,#15650));
#3887=EDGE_LOOP('',(#15651,#15652,#15653,#15654));
#3888=EDGE_LOOP('',(#15655,#15656,#15657,#15658));
#3889=EDGE_LOOP('',(#15659,#15660,#15661,#15662));
#3890=EDGE_LOOP('',(#15663,#15664,#15665,#15666));
#3891=EDGE_LOOP('',(#15667,#15668,#15669,#15670));
#3892=EDGE_LOOP('',(#15671,#15672,#15673,#15674,#15675,#15676,#15677,#15678,
#15679,#15680,#15681,#15682,#15683,#15684,#15685,#15686));
#3893=EDGE_LOOP('',(#15687,#15688,#15689,#15690));
#3894=EDGE_LOOP('',(#15691,#15692,#15693,#15694));
#3895=EDGE_LOOP('',(#15695,#15696,#15697,#15698));
#3896=EDGE_LOOP('',(#15699,#15700,#15701,#15702));
#3897=EDGE_LOOP('',(#15703,#15704,#15705,#15706,#15707));
#3898=EDGE_LOOP('',(#15708,#15709,#15710,#15711));
#3899=EDGE_LOOP('',(#15712));
#3900=EDGE_LOOP('',(#15713));
#3901=LINE('',#22955,#4855);
#3902=LINE('',#22957,#4856);
#3903=LINE('',#22958,#4857);
#3904=LINE('',#22961,#4858);
#3905=LINE('',#22972,#4859);
#3906=LINE('',#22974,#4860);
#3907=LINE('',#22980,#4861);
#3908=LINE('',#22982,#4862);
#3909=LINE('',#22992,#4863);
#3910=LINE('',#23004,#4864);
#3911=LINE('',#23005,#4865);
#3912=LINE('',#23010,#4866);
#3913=LINE('',#23026,#4867);
#3914=LINE('',#23028,#4868);
#3915=LINE('',#23029,#4869);
#3916=LINE('',#23032,#4870);
#3917=LINE('',#23043,#4871);
#3918=LINE('',#23045,#4872);
#3919=LINE('',#23051,#4873);
#3920=LINE('',#23053,#4874);
#3921=LINE('',#23063,#4875);
#3922=LINE('',#23075,#4876);
#3923=LINE('',#23076,#4877);
#3924=LINE('',#23081,#4878);
#3925=LINE('',#23088,#4879);
#3926=LINE('',#23094,#4880);
#3927=LINE('',#23098,#4881);
#3928=LINE('',#23102,#4882);
#3929=LINE('',#23105,#4883);
#3930=LINE('',#23111,#4884);
#3931=LINE('',#23116,#4885);
#3932=LINE('',#23121,#4886);
#3933=LINE('',#23125,#4887);
#3934=LINE('',#23129,#4888);
#3935=LINE('',#23133,#4889);
#3936=LINE('',#23141,#4890);
#3937=LINE('',#23145,#4891);
#3938=LINE('',#23149,#4892);
#3939=LINE('',#23266,#4893);
#3940=LINE('',#23334,#4894);
#3941=LINE('',#23336,#4895);
#3942=LINE('',#23338,#4896);
#3943=LINE('',#23339,#4897);
#3944=LINE('',#23342,#4898);
#3945=LINE('',#23344,#4899);
#3946=LINE('',#23346,#4900);
#3947=LINE('',#23347,#4901);
#3948=LINE('',#23350,#4902);
#3949=LINE('',#23352,#4903);
#3950=LINE('',#23354,#4904);
#3951=LINE('',#23355,#4905);
#3952=LINE('',#23358,#4906);
#3953=LINE('',#23360,#4907);
#3954=LINE('',#23362,#4908);
#3955=LINE('',#23363,#4909);
#3956=LINE('',#23366,#4910);
#3957=LINE('',#23368,#4911);
#3958=LINE('',#23370,#4912);
#3959=LINE('',#23371,#4913);
#3960=LINE('',#23374,#4914);
#3961=LINE('',#23376,#4915);
#3962=LINE('',#23378,#4916);
#3963=LINE('',#23379,#4917);
#3964=LINE('',#23423,#4918);
#3965=LINE('',#23424,#4919);
#3966=LINE('',#23426,#4920);
#3967=LINE('',#23428,#4921);
#3968=LINE('',#23504,#4922);
#3969=LINE('',#23543,#4923);
#3970=LINE('',#23544,#4924);
#3971=LINE('',#23546,#4925);
#3972=LINE('',#23548,#4926);
#3973=LINE('',#23609,#4927);
#3974=LINE('',#23610,#4928);
#3975=LINE('',#23626,#4929);
#3976=LINE('',#23627,#4930);
#3977=LINE('',#23629,#4931);
#3978=LINE('',#23631,#4932);
#3979=LINE('',#23633,#4933);
#3980=LINE('',#23635,#4934);
#3981=LINE('',#23637,#4935);
#3982=LINE('',#23638,#4936);
#3983=LINE('',#23643,#4937);
#3984=LINE('',#23655,#4938);
#3985=LINE('',#23663,#4939);
#3986=LINE('',#23671,#4940);
#3987=LINE('',#23676,#4941);
#3988=LINE('',#23678,#4942);
#3989=LINE('',#23681,#4943);
#3990=LINE('',#23682,#4944);
#3991=LINE('',#23695,#4945);
#3992=LINE('',#23700,#4946);
#3993=LINE('',#23710,#4947);
#3994=LINE('',#23720,#4948);
#3995=LINE('',#24053,#4949);
#3996=LINE('',#24060,#4950);
#3997=LINE('',#24112,#4951);
#3998=LINE('',#24118,#4952);
#3999=LINE('',#24415,#4953);
#4000=LINE('',#24417,#4954);
#4001=LINE('',#24438,#4955);
#4002=LINE('',#24440,#4956);
#4003=LINE('',#24443,#4957);
#4004=LINE('',#24459,#4958);
#4005=LINE('',#24460,#4959);
#4006=LINE('',#24463,#4960);
#4007=LINE('',#24465,#4961);
#4008=LINE('',#24466,#4962);
#4009=LINE('',#24469,#4963);
#4010=LINE('',#24485,#4964);
#4011=LINE('',#24492,#4965);
#4012=LINE('',#24502,#4966);
#4013=LINE('',#24504,#4967);
#4014=LINE('',#24507,#4968);
#4015=LINE('',#24509,#4969);
#4016=LINE('',#24510,#4970);
#4017=LINE('',#24511,#4971);
#4018=LINE('',#24514,#4972);
#4019=LINE('',#24520,#4973);
#4020=LINE('',#24544,#4974);
#4021=LINE('',#24546,#4975);
#4022=LINE('',#24549,#4976);
#4023=LINE('',#24597,#4977);
#4024=LINE('',#24599,#4978);
#4025=LINE('',#24601,#4979);
#4026=LINE('',#24603,#4980);
#4027=LINE('',#24605,#4981);
#4028=LINE('',#24607,#4982);
#4029=LINE('',#24610,#4983);
#4030=LINE('',#24617,#4984);
#4031=LINE('',#24624,#4985);
#4032=LINE('',#24626,#4986);
#4033=LINE('',#24630,#4987);
#4034=LINE('',#24632,#4988);
#4035=LINE('',#24634,#4989);
#4036=LINE('',#24636,#4990);
#4037=LINE('',#24637,#4991);
#4038=LINE('',#24644,#4992);
#4039=LINE('',#24648,#4993);
#4040=LINE('',#24650,#4994);
#4041=LINE('',#24652,#4995);
#4042=LINE('',#24660,#4996);
#4043=LINE('',#24664,#4997);
#4044=LINE('',#24671,#4998);
#4045=LINE('',#24675,#4999);
#4046=LINE('',#24721,#5000);
#4047=LINE('',#24727,#5001);
#4048=LINE('',#24746,#5002);
#4049=LINE('',#24751,#5003);
#4050=LINE('',#24755,#5004);
#4051=LINE('',#24759,#5005);
#4052=LINE('',#24763,#5006);
#4053=LINE('',#24767,#5007);
#4054=LINE('',#24771,#5008);
#4055=LINE('',#24780,#5009);
#4056=LINE('',#24784,#5010);
#4057=LINE('',#24790,#5011);
#4058=LINE('',#24792,#5012);
#4059=LINE('',#24798,#5013);
#4060=LINE('',#24802,#5014);
#4061=LINE('',#24809,#5015);
#4062=LINE('',#24826,#5016);
#4063=LINE('',#24846,#5017);
#4064=LINE('',#24896,#5018);
#4065=LINE('',#24901,#5019);
#4066=LINE('',#24905,#5020);
#4067=LINE('',#24909,#5021);
#4068=LINE('',#24913,#5022);
#4069=LINE('',#24917,#5023);
#4070=LINE('',#24921,#5024);
#4071=LINE('',#24926,#5025);
#4072=LINE('',#24930,#5026);
#4073=LINE('',#24936,#5027);
#4074=LINE('',#24940,#5028);
#4075=LINE('',#24948,#5029);
#4076=LINE('',#24954,#5030);
#4077=LINE('',#24960,#5031);
#4078=LINE('',#24966,#5032);
#4079=LINE('',#24972,#5033);
#4080=LINE('',#24978,#5034);
#4081=LINE('',#24984,#5035);
#4082=LINE('',#24992,#5036);
#4083=LINE('',#24999,#5037);
#4084=LINE('',#25005,#5038);
#4085=LINE('',#25011,#5039);
#4086=LINE('',#25017,#5040);
#4087=LINE('',#25023,#5041);
#4088=LINE('',#25029,#5042);
#4089=LINE('',#25035,#5043);
#4090=LINE('',#25042,#5044);
#4091=LINE('',#25050,#5045);
#4092=LINE('',#25056,#5046);
#4093=LINE('',#25066,#5047);
#4094=LINE('',#25074,#5048);
#4095=LINE('',#25078,#5049);
#4096=LINE('',#25082,#5050);
#4097=LINE('',#25089,#5051);
#4098=LINE('',#25098,#5052);
#4099=LINE('',#25104,#5053);
#4100=LINE('',#25113,#5054);
#4101=LINE('',#25118,#5055);
#4102=LINE('',#25120,#5056);
#4103=LINE('',#25125,#5057);
#4104=LINE('',#25158,#5058);
#4105=LINE('',#25242,#5059);
#4106=LINE('',#25332,#5060);
#4107=LINE('',#25422,#5061);
#4108=LINE('',#25506,#5062);
#4109=LINE('',#25596,#5063);
#4110=LINE('',#25680,#5064);
#4111=LINE('',#25767,#5065);
#4112=LINE('',#25842,#5066);
#4113=LINE('',#25926,#5067);
#4114=LINE('',#26016,#5068);
#4115=LINE('',#26100,#5069);
#4116=LINE('',#26187,#5070);
#4117=LINE('',#26277,#5071);
#4118=LINE('',#26361,#5072);
#4119=LINE('',#26383,#5073);
#4120=LINE('',#26420,#5074);
#4121=LINE('',#26457,#5075);
#4122=LINE('',#26495,#5076);
#4123=LINE('',#26532,#5077);
#4124=LINE('',#26569,#5078);
#4125=LINE('',#26606,#5079);
#4126=LINE('',#26641,#5080);
#4127=LINE('',#26675,#5081);
#4128=LINE('',#26712,#5082);
#4129=LINE('',#26749,#5083);
#4130=LINE('',#26786,#5084);
#4131=LINE('',#26823,#5085);
#4132=LINE('',#26861,#5086);
#4133=LINE('',#26898,#5087);
#4134=LINE('',#26931,#5088);
#4135=LINE('',#27015,#5089);
#4136=LINE('',#27105,#5090);
#4137=LINE('',#27195,#5091);
#4138=LINE('',#27279,#5092);
#4139=LINE('',#27369,#5093);
#4140=LINE('',#27453,#5094);
#4141=LINE('',#27540,#5095);
#4142=LINE('',#27615,#5096);
#4143=LINE('',#27699,#5097);
#4144=LINE('',#27789,#5098);
#4145=LINE('',#27873,#5099);
#4146=LINE('',#27960,#5100);
#4147=LINE('',#28050,#5101);
#4148=LINE('',#28134,#5102);
#4149=LINE('',#28156,#5103);
#4150=LINE('',#28193,#5104);
#4151=LINE('',#28230,#5105);
#4152=LINE('',#28268,#5106);
#4153=LINE('',#28305,#5107);
#4154=LINE('',#28342,#5108);
#4155=LINE('',#28379,#5109);
#4156=LINE('',#28414,#5110);
#4157=LINE('',#28448,#5111);
#4158=LINE('',#28485,#5112);
#4159=LINE('',#28522,#5113);
#4160=LINE('',#28559,#5114);
#4161=LINE('',#28596,#5115);
#4162=LINE('',#28634,#5116);
#4163=LINE('',#32870,#5117);
#4164=LINE('',#32879,#5118);
#4165=LINE('',#32884,#5119);
#4166=LINE('',#32891,#5120);
#4167=LINE('',#33281,#5121);
#4168=LINE('',#33290,#5122);
#4169=LINE('',#33292,#5123);
#4170=LINE('',#33308,#5124);
#4171=LINE('',#33311,#5125);
#4172=LINE('',#33333,#5126);
#4173=LINE('',#33365,#5127);
#4174=LINE('',#33366,#5128);
#4175=LINE('',#33398,#5129);
#4176=LINE('',#33399,#5130);
#4177=LINE('',#33406,#5131);
#4178=LINE('',#33407,#5132);
#4179=LINE('',#33439,#5133);
#4180=LINE('',#33440,#5134);
#4181=LINE('',#33447,#5135);
#4182=LINE('',#33448,#5136);
#4183=LINE('',#33455,#5137);
#4184=LINE('',#33456,#5138);
#4185=LINE('',#33473,#5139);
#4186=LINE('',#33490,#5140);
#4187=LINE('',#33494,#5141);
#4188=LINE('',#33497,#5142);
#4189=LINE('',#33507,#5143);
#4190=LINE('',#33516,#5144);
#4191=LINE('',#33518,#5145);
#4192=LINE('',#33520,#5146);
#4193=LINE('',#33532,#5147);
#4194=LINE('',#33540,#5148);
#4195=LINE('',#33547,#5149);
#4196=LINE('',#33568,#5150);
#4197=LINE('',#33585,#5151);
#4198=LINE('',#33588,#5152);
#4199=LINE('',#33599,#5153);
#4200=LINE('',#33600,#5154);
#4201=LINE('',#33611,#5155);
#4202=LINE('',#33612,#5156);
#4203=LINE('',#33623,#5157);
#4204=LINE('',#33624,#5158);
#4205=LINE('',#33630,#5159);
#4206=LINE('',#33633,#5160);
#4207=LINE('',#33636,#5161);
#4208=LINE('',#33637,#5162);
#4209=LINE('',#33640,#5163);
#4210=LINE('',#33644,#5164);
#4211=LINE('',#33645,#5165);
#4212=LINE('',#33659,#5166);
#4213=LINE('',#33668,#5167);
#4214=LINE('',#33677,#5168);
#4215=LINE('',#33678,#5169);
#4216=LINE('',#33689,#5170);
#4217=LINE('',#33690,#5171);
#4218=LINE('',#33695,#5172);
#4219=LINE('',#33696,#5173);
#4220=LINE('',#33698,#5174);
#4221=LINE('',#33710,#5175);
#4222=LINE('',#33713,#5176);
#4223=LINE('',#33724,#5177);
#4224=LINE('',#33725,#5178);
#4225=LINE('',#33736,#5179);
#4226=LINE('',#33737,#5180);
#4227=LINE('',#33748,#5181);
#4228=LINE('',#33749,#5182);
#4229=LINE('',#33755,#5183);
#4230=LINE('',#33758,#5184);
#4231=LINE('',#33761,#5185);
#4232=LINE('',#33762,#5186);
#4233=LINE('',#33765,#5187);
#4234=LINE('',#33769,#5188);
#4235=LINE('',#33770,#5189);
#4236=LINE('',#33784,#5190);
#4237=LINE('',#33793,#5191);
#4238=LINE('',#33802,#5192);
#4239=LINE('',#33803,#5193);
#4240=LINE('',#33814,#5194);
#4241=LINE('',#33815,#5195);
#4242=LINE('',#33820,#5196);
#4243=LINE('',#33821,#5197);
#4244=LINE('',#33823,#5198);
#4245=LINE('',#34039,#5199);
#4246=LINE('',#34041,#5200);
#4247=LINE('',#34043,#5201);
#4248=LINE('',#34045,#5202);
#4249=LINE('',#34047,#5203);
#4250=LINE('',#34049,#5204);
#4251=LINE('',#34051,#5205);
#4252=LINE('',#34057,#5206);
#4253=LINE('',#34062,#5207);
#4254=LINE('',#34064,#5208);
#4255=LINE('',#34069,#5209);
#4256=LINE('',#34102,#5210);
#4257=LINE('',#34186,#5211);
#4258=LINE('',#34276,#5212);
#4259=LINE('',#34360,#5213);
#4260=LINE('',#34450,#5214);
#4261=LINE('',#34540,#5215);
#4262=LINE('',#34550,#5216);
#4263=LINE('',#34587,#5217);
#4264=LINE('',#34625,#5218);
#4265=LINE('',#34662,#5219);
#4266=LINE('',#34699,#5220);
#4267=LINE('',#34737,#5221);
#4268=LINE('',#34743,#5222);
#4269=LINE('',#35019,#5223);
#4270=LINE('',#35025,#5224);
#4271=LINE('',#35031,#5225);
#4272=LINE('',#35036,#5226);
#4273=LINE('',#35038,#5227);
#4274=LINE('',#35040,#5228);
#4275=LINE('',#35042,#5229);
#4276=LINE('',#35044,#5230);
#4277=LINE('',#35045,#5231);
#4278=LINE('',#35048,#5232);
#4279=LINE('',#35050,#5233);
#4280=LINE('',#35051,#5234);
#4281=LINE('',#35054,#5235);
#4282=LINE('',#35055,#5236);
#4283=LINE('',#35058,#5237);
#4284=LINE('',#35060,#5238);
#4285=LINE('',#35061,#5239);
#4286=LINE('',#35064,#5240);
#4287=LINE('',#35065,#5241);
#4288=LINE('',#35067,#5242);
#4289=LINE('',#35069,#5243);
#4290=LINE('',#35072,#5244);
#4291=LINE('',#35074,#5245);
#4292=LINE('',#35075,#5246);
#4293=LINE('',#35078,#5247);
#4294=LINE('',#35079,#5248);
#4295=LINE('',#35082,#5249);
#4296=LINE('',#35083,#5250);
#4297=LINE('',#36057,#5251);
#4298=LINE('',#36058,#5252);
#4299=LINE('',#36061,#5253);
#4300=LINE('',#36062,#5254);
#4301=LINE('',#36064,#5255);
#4302=LINE('',#36069,#5256);
#4303=LINE('',#36077,#5257);
#4304=LINE('',#36081,#5258);
#4305=LINE('',#36085,#5259);
#4306=LINE('',#36088,#5260);
#4307=LINE('',#36093,#5261);
#4308=LINE('',#36095,#5262);
#4309=LINE('',#36096,#5263);
#4310=LINE('',#36100,#5264);
#4311=LINE('',#36103,#5265);
#4312=LINE('',#36104,#5266);
#4313=LINE('',#36108,#5267);
#4314=LINE('',#36111,#5268);
#4315=LINE('',#36112,#5269);
#4316=LINE('',#36116,#5270);
#4317=LINE('',#36119,#5271);
#4318=LINE('',#36120,#5272);
#4319=LINE('',#36126,#5273);
#4320=LINE('',#36134,#5274);
#4321=LINE('',#36136,#5275);
#4322=LINE('',#36138,#5276);
#4323=LINE('',#36140,#5277);
#4324=LINE('',#36142,#5278);
#4325=LINE('',#36144,#5279);
#4326=LINE('',#36145,#5280);
#4327=LINE('',#36151,#5281);
#4328=LINE('',#36156,#5282);
#4329=LINE('',#36161,#5283);
#4330=LINE('',#36166,#5284);
#4331=LINE('',#36171,#5285);
#4332=LINE('',#36180,#5286);
#4333=LINE('',#36185,#5287);
#4334=LINE('',#36195,#5288);
#4335=LINE('',#36199,#5289);
#4336=LINE('',#36200,#5290);
#4337=LINE('',#36202,#5291);
#4338=LINE('',#36205,#5292);
#4339=LINE('',#36206,#5293);
#4340=LINE('',#36208,#5294);
#4341=LINE('',#36211,#5295);
#4342=LINE('',#36212,#5296);
#4343=LINE('',#36216,#5297);
#4344=LINE('',#36218,#5298);
#4345=LINE('',#36220,#5299);
#4346=LINE('',#36221,#5300);
#4347=LINE('',#36222,#5301);
#4348=LINE('',#36226,#5302);
#4349=LINE('',#36227,#5303);
#4350=LINE('',#36230,#5304);
#4351=LINE('',#36231,#5305);
#4352=LINE('',#36233,#5306);
#4353=LINE('',#36235,#5307);
#4354=LINE('',#36244,#5308);
#4355=LINE('',#36246,#5309);
#4356=LINE('',#36251,#5310);
#4357=LINE('',#36253,#5311);
#4358=LINE('',#36254,#5312);
#4359=LINE('',#36258,#5313);
#4360=LINE('',#36260,#5314);
#4361=LINE('',#36261,#5315);
#4362=LINE('',#36265,#5316);
#4363=LINE('',#36267,#5317);
#4364=LINE('',#36268,#5318);
#4365=LINE('',#36270,#5319);
#4366=LINE('',#36271,#5320);
#4367=LINE('',#36275,#5321);
#4368=LINE('',#36277,#5322);
#4369=LINE('',#36278,#5323);
#4370=LINE('',#36282,#5324);
#4371=LINE('',#36284,#5325);
#4372=LINE('',#36285,#5326);
#4373=LINE('',#36289,#5327);
#4374=LINE('',#36291,#5328);
#4375=LINE('',#36292,#5329);
#4376=LINE('',#36294,#5330);
#4377=LINE('',#36295,#5331);
#4378=LINE('',#36297,#5332);
#4379=LINE('',#36298,#5333);
#4380=LINE('',#36302,#5334);
#4381=LINE('',#36303,#5335);
#4382=LINE('',#36304,#5336);
#4383=LINE('',#36308,#5337);
#4384=LINE('',#36309,#5338);
#4385=LINE('',#36310,#5339);
#4386=LINE('',#36312,#5340);
#4387=LINE('',#36313,#5341);
#4388=LINE('',#36315,#5342);
#4389=LINE('',#36316,#5343);
#4390=LINE('',#36320,#5344);
#4391=LINE('',#36321,#5345);
#4392=LINE('',#36322,#5346);
#4393=LINE('',#36326,#5347);
#4394=LINE('',#36327,#5348);
#4395=LINE('',#36328,#5349);
#4396=LINE('',#36330,#5350);
#4397=LINE('',#36331,#5351);
#4398=LINE('',#36335,#5352);
#4399=LINE('',#36336,#5353);
#4400=LINE('',#36337,#5354);
#4401=LINE('',#36341,#5355);
#4402=LINE('',#36342,#5356);
#4403=LINE('',#36343,#5357);
#4404=LINE('',#36345,#5358);
#4405=LINE('',#36347,#5359);
#4406=LINE('',#36349,#5360);
#4407=LINE('',#36359,#5361);
#4408=LINE('',#36365,#5362);
#4409=LINE('',#36372,#5363);
#4410=LINE('',#36375,#5364);
#4411=LINE('',#36382,#5365);
#4412=LINE('',#36388,#5366);
#4413=LINE('',#36391,#5367);
#4414=LINE('',#36392,#5368);
#4415=LINE('',#36393,#5369);
#4416=LINE('',#36403,#5370);
#4417=LINE('',#36407,#5371);
#4418=LINE('',#36415,#5372);
#4419=LINE('',#36422,#5373);
#4420=LINE('',#36426,#5374);
#4421=LINE('',#36438,#5375);
#4422=LINE('',#36446,#5376);
#4423=LINE('',#36450,#5377);
#4424=LINE('',#36454,#5378);
#4425=LINE('',#36461,#5379);
#4426=LINE('',#36466,#5380);
#4427=LINE('',#36468,#5381);
#4428=LINE('',#36470,#5382);
#4429=LINE('',#36471,#5383);
#4430=LINE('',#36485,#5384);
#4431=LINE('',#36488,#5385);
#4432=LINE('',#36493,#5386);
#4433=LINE('',#36497,#5387);
#4434=LINE('',#36499,#5388);
#4435=LINE('',#36501,#5389);
#4436=LINE('',#36502,#5390);
#4437=LINE('',#36507,#5391);
#4438=LINE('',#36512,#5392);
#4439=LINE('',#36513,#5393);
#4440=LINE('',#36514,#5394);
#4441=LINE('',#36519,#5395);
#4442=LINE('',#36524,#5396);
#4443=LINE('',#36525,#5397);
#4444=LINE('',#36526,#5398);
#4445=LINE('',#36531,#5399);
#4446=LINE('',#36536,#5400);
#4447=LINE('',#36537,#5401);
#4448=LINE('',#36538,#5402);
#4449=LINE('',#36542,#5403);
#4450=LINE('',#36546,#5404);
#4451=LINE('',#36547,#5405);
#4452=LINE('',#36552,#5406);
#4453=LINE('',#36557,#5407);
#4454=LINE('',#36558,#5408);
#4455=LINE('',#36559,#5409);
#4456=LINE('',#36564,#5410);
#4457=LINE('',#36569,#5411);
#4458=LINE('',#36570,#5412);
#4459=LINE('',#36571,#5413);
#4460=LINE('',#36576,#5414);
#4461=LINE('',#36581,#5415);
#4462=LINE('',#36582,#5416);
#4463=LINE('',#36583,#5417);
#4464=LINE('',#36589,#5418);
#4465=LINE('',#36593,#5419);
#4466=LINE('',#36594,#5420);
#4467=LINE('',#36597,#5421);
#4468=LINE('',#36601,#5422);
#4469=LINE('',#36602,#5423);
#4470=LINE('',#36605,#5424);
#4471=LINE('',#36609,#5425);
#4472=LINE('',#36610,#5426);
#4473=LINE('',#36613,#5427);
#4474=LINE('',#36617,#5428);
#4475=LINE('',#36618,#5429);
#4476=LINE('',#36634,#5430);
#4477=LINE('',#36636,#5431);
#4478=LINE('',#36637,#5432);
#4479=LINE('',#36642,#5433);
#4480=LINE('',#36647,#5434);
#4481=LINE('',#36648,#5435);
#4482=LINE('',#36649,#5436);
#4483=LINE('',#36654,#5437);
#4484=LINE('',#36659,#5438);
#4485=LINE('',#36660,#5439);
#4486=LINE('',#36661,#5440);
#4487=LINE('',#36666,#5441);
#4488=LINE('',#36671,#5442);
#4489=LINE('',#36672,#5443);
#4490=LINE('',#36673,#5444);
#4491=LINE('',#36677,#5445);
#4492=LINE('',#36681,#5446);
#4493=LINE('',#36682,#5447);
#4494=LINE('',#36685,#5448);
#4495=LINE('',#36689,#5449);
#4496=LINE('',#36690,#5450);
#4497=LINE('',#36693,#5451);
#4498=LINE('',#36697,#5452);
#4499=LINE('',#36698,#5453);
#4500=LINE('',#36701,#5454);
#4501=LINE('',#36705,#5455);
#4502=LINE('',#36706,#5456);
#4503=LINE('',#36710,#5457);
#4504=LINE('',#36712,#5458);
#4505=LINE('',#36714,#5459);
#4506=LINE('',#36716,#5460);
#4507=LINE('',#36718,#5461);
#4508=LINE('',#36720,#5462);
#4509=LINE('',#36724,#5463);
#4510=LINE('',#36726,#5464);
#4511=LINE('',#36728,#5465);
#4512=LINE('',#36730,#5466);
#4513=LINE('',#36732,#5467);
#4514=LINE('',#36734,#5468);
#4515=LINE('',#36739,#5469);
#4516=LINE('',#36763,#5470);
#4517=LINE('',#36811,#5471);
#4518=LINE('',#36859,#5472);
#4519=LINE('',#36913,#5473);
#4520=LINE('',#36961,#5474);
#4521=LINE('',#37009,#5475);
#4522=LINE('',#37063,#5476);
#4523=LINE('',#37111,#5477);
#4524=LINE('',#37165,#5478);
#4525=LINE('',#37212,#5479);
#4526=LINE('',#37232,#5480);
#4527=LINE('',#37257,#5481);
#4528=LINE('',#37282,#5482);
#4529=LINE('',#37307,#5483);
#4530=LINE('',#37332,#5484);
#4531=LINE('',#37356,#5485);
#4532=LINE('',#37381,#5486);
#4533=LINE('',#37406,#5487);
#4534=LINE('',#37433,#5488);
#4535=LINE('',#37439,#5489);
#4536=LINE('',#37446,#5490);
#4537=LINE('',#37449,#5491);
#4538=LINE('',#38385,#5492);
#4539=LINE('',#38390,#5493);
#4540=LINE('',#38396,#5494);
#4541=LINE('',#38420,#5495);
#4542=LINE('',#38468,#5496);
#4543=LINE('',#38516,#5497);
#4544=LINE('',#38567,#5498);
#4545=LINE('',#38618,#5499);
#4546=LINE('',#38666,#5500);
#4547=LINE('',#38714,#5501);
#4548=LINE('',#38768,#5502);
#4549=LINE('',#38816,#5503);
#4550=LINE('',#38864,#5504);
#4551=LINE('',#38918,#5505);
#4552=LINE('',#38966,#5506);
#4553=LINE('',#39014,#5507);
#4554=LINE('',#39062,#5508);
#4555=LINE('',#39116,#5509);
#4556=LINE('',#39164,#5510);
#4557=LINE('',#39212,#5511);
#4558=LINE('',#39266,#5512);
#4559=LINE('',#39314,#5513);
#4560=LINE('',#39362,#5514);
#4561=LINE('',#39416,#5515);
#4562=LINE('',#39464,#5516);
#4563=LINE('',#39512,#5517);
#4564=LINE('',#39560,#5518);
#4565=LINE('',#39614,#5519);
#4566=LINE('',#39662,#5520);
#4567=LINE('',#39710,#5521);
#4568=LINE('',#39764,#5522);
#4569=LINE('',#39812,#5523);
#4570=LINE('',#39860,#5524);
#4571=LINE('',#39914,#5525);
#4572=LINE('',#39962,#5526);
#4573=LINE('',#40010,#5527);
#4574=LINE('',#40058,#5528);
#4575=LINE('',#40112,#5529);
#4576=LINE('',#40160,#5530);
#4577=LINE('',#40208,#5531);
#4578=LINE('',#40262,#5532);
#4579=LINE('',#40310,#5533);
#4580=LINE('',#40358,#5534);
#4581=LINE('',#40412,#5535);
#4582=LINE('',#40460,#5536);
#4583=LINE('',#40508,#5537);
#4584=LINE('',#40556,#5538);
#4585=LINE('',#40566,#5539);
#4586=LINE('',#40591,#5540);
#4587=LINE('',#40615,#5541);
#4588=LINE('',#40639,#5542);
#4589=LINE('',#40664,#5543);
#4590=LINE('',#40689,#5544);
#4591=LINE('',#40713,#5545);
#4592=LINE('',#40738,#5546);
#4593=LINE('',#40763,#5547);
#4594=LINE('',#40787,#5548);
#4595=LINE('',#40812,#5549);
#4596=LINE('',#40837,#5550);
#4597=LINE('',#40861,#5551);
#4598=LINE('',#40885,#5552);
#4599=LINE('',#40910,#5553);
#4600=LINE('',#40935,#5554);
#4601=LINE('',#40959,#5555);
#4602=LINE('',#40984,#5556);
#4603=LINE('',#41009,#5557);
#4604=LINE('',#41033,#5558);
#4605=LINE('',#41058,#5559);
#4606=LINE('',#41083,#5560);
#4607=LINE('',#41107,#5561);
#4608=LINE('',#41131,#5562);
#4609=LINE('',#41156,#5563);
#4610=LINE('',#41181,#5564);
#4611=LINE('',#41205,#5565);
#4612=LINE('',#41230,#5566);
#4613=LINE('',#41255,#5567);
#4614=LINE('',#41279,#5568);
#4615=LINE('',#41304,#5569);
#4616=LINE('',#41329,#5570);
#4617=LINE('',#41353,#5571);
#4618=LINE('',#41377,#5572);
#4619=LINE('',#41402,#5573);
#4620=LINE('',#41427,#5574);
#4621=LINE('',#41451,#5575);
#4622=LINE('',#41476,#5576);
#4623=LINE('',#41501,#5577);
#4624=LINE('',#41525,#5578);
#4625=LINE('',#41550,#5579);
#4626=LINE('',#41574,#5580);
#4627=LINE('',#41599,#5581);
#4628=LINE('',#44327,#5582);
#4629=LINE('',#44338,#5583);
#4630=LINE('',#44340,#5584);
#4631=LINE('',#44341,#5585);
#4632=LINE('',#44344,#5586);
#4633=LINE('',#44345,#5587);
#4634=LINE('',#44348,#5588);
#4635=LINE('',#44349,#5589);
#4636=LINE('',#44352,#5590);
#4637=LINE('',#44354,#5591);
#4638=LINE('',#44355,#5592);
#4639=LINE('',#44358,#5593);
#4640=LINE('',#44360,#5594);
#4641=LINE('',#44367,#5595);
#4642=LINE('',#44373,#5596);
#4643=LINE('',#44397,#5597);
#4644=LINE('',#44445,#5598);
#4645=LINE('',#44493,#5599);
#4646=LINE('',#44541,#5600);
#4647=LINE('',#44595,#5601);
#4648=LINE('',#44643,#5602);
#4649=LINE('',#44691,#5603);
#4650=LINE('',#44745,#5604);
#4651=LINE('',#44793,#5605);
#4652=LINE('',#44841,#5606);
#4653=LINE('',#44889,#5607);
#4654=LINE('',#44943,#5608);
#4655=LINE('',#44991,#5609);
#4656=LINE('',#45039,#5610);
#4657=LINE('',#45093,#5611);
#4658=LINE('',#45141,#5612);
#4659=LINE('',#45189,#5613);
#4660=LINE('',#45237,#5614);
#4661=LINE('',#45291,#5615);
#4662=LINE('',#45339,#5616);
#4663=LINE('',#45387,#5617);
#4664=LINE('',#45441,#5618);
#4665=LINE('',#45489,#5619);
#4666=LINE('',#45537,#5620);
#4667=LINE('',#45585,#5621);
#4668=LINE('',#45639,#5622);
#4669=LINE('',#45687,#5623);
#4670=LINE('',#45735,#5624);
#4671=LINE('',#45789,#5625);
#4672=LINE('',#45837,#5626);
#4673=LINE('',#45885,#5627);
#4674=LINE('',#45933,#5628);
#4675=LINE('',#45987,#5629);
#4676=LINE('',#46035,#5630);
#4677=LINE('',#46083,#5631);
#4678=LINE('',#46137,#5632);
#4679=LINE('',#46185,#5633);
#4680=LINE('',#46233,#5634);
#4681=LINE('',#46281,#5635);
#4682=LINE('',#46335,#5636);
#4683=LINE('',#46383,#5637);
#4684=LINE('',#46431,#5638);
#4685=LINE('',#46485,#5639);
#4686=LINE('',#46533,#5640);
#4687=LINE('',#46581,#5641);
#4688=LINE('',#46629,#5642);
#4689=LINE('',#46683,#5643);
#4690=LINE('',#46731,#5644);
#4691=LINE('',#46779,#5645);
#4692=LINE('',#46833,#5646);
#4693=LINE('',#46881,#5647);
#4694=LINE('',#46929,#5648);
#4695=LINE('',#46977,#5649);
#4696=LINE('',#47031,#5650);
#4697=LINE('',#47079,#5651);
#4698=LINE('',#47127,#5652);
#4699=LINE('',#47181,#5653);
#4700=LINE('',#47229,#5654);
#4701=LINE('',#47277,#5655);
#4702=LINE('',#47325,#5656);
#4703=LINE('',#47379,#5657);
#4704=LINE('',#47427,#5658);
#4705=LINE('',#47475,#5659);
#4706=LINE('',#47529,#5660);
#4707=LINE('',#47577,#5661);
#4708=LINE('',#47625,#5662);
#4709=LINE('',#47673,#5663);
#4710=LINE('',#47727,#5664);
#4711=LINE('',#47775,#5665);
#4712=LINE('',#47823,#5666);
#4713=LINE('',#47877,#5667);
#4714=LINE('',#47925,#5668);
#4715=LINE('',#47973,#5669);
#4716=LINE('',#48021,#5670);
#4717=LINE('',#48075,#5671);
#4718=LINE('',#48123,#5672);
#4719=LINE('',#48171,#5673);
#4720=LINE('',#48225,#5674);
#4721=LINE('',#48273,#5675);
#4722=LINE('',#48321,#5676);
#4723=LINE('',#48369,#5677);
#4724=LINE('',#48423,#5678);
#4725=LINE('',#48471,#5679);
#4726=LINE('',#48519,#5680);
#4727=LINE('',#48573,#5681);
#4728=LINE('',#48621,#5682);
#4729=LINE('',#48669,#5683);
#4730=LINE('',#48717,#5684);
#4731=LINE('',#48727,#5685);
#4732=LINE('',#48764,#5686);
#4733=LINE('',#48812,#5687);
#4734=LINE('',#48860,#5688);
#4735=LINE('',#48885,#5689);
#4736=LINE('',#48910,#5690);
#4737=LINE('',#48934,#5691);
#4738=LINE('',#48959,#5692);
#4739=LINE('',#48998,#5693);
#4740=LINE('',#49034,#5694);
#4741=LINE('',#49058,#5695);
#4742=LINE('',#49083,#5696);
#4743=LINE('',#49108,#5697);
#4744=LINE('',#49132,#5698);
#4745=LINE('',#49157,#5699);
#4746=LINE('',#49182,#5700);
#4747=LINE('',#49218,#5701);
#4748=LINE('',#49254,#5702);
#4749=LINE('',#49279,#5703);
#4750=LINE('',#49304,#5704);
#4751=LINE('',#49328,#5705);
#4752=LINE('',#49353,#5706);
#4753=LINE('',#49378,#5707);
#4754=LINE('',#49402,#5708);
#4755=LINE('',#49426,#5709);
#4756=LINE('',#49451,#5710);
#4757=LINE('',#49476,#5711);
#4758=LINE('',#49500,#5712);
#4759=LINE('',#49525,#5713);
#4760=LINE('',#49550,#5714);
#4761=LINE('',#49574,#5715);
#4762=LINE('',#49598,#5716);
#4763=LINE('',#49623,#5717);
#4764=LINE('',#49648,#5718);
#4765=LINE('',#49672,#5719);
#4766=LINE('',#49697,#5720);
#4767=LINE('',#49722,#5721);
#4768=LINE('',#49746,#5722);
#4769=LINE('',#49770,#5723);
#4770=LINE('',#49795,#5724);
#4771=LINE('',#49820,#5725);
#4772=LINE('',#49844,#5726);
#4773=LINE('',#49869,#5727);
#4774=LINE('',#49894,#5728);
#4775=LINE('',#49918,#5729);
#4776=LINE('',#49942,#5730);
#4777=LINE('',#49967,#5731);
#4778=LINE('',#49992,#5732);
#4779=LINE('',#50016,#5733);
#4780=LINE('',#50041,#5734);
#4781=LINE('',#50066,#5735);
#4782=LINE('',#50090,#5736);
#4783=LINE('',#50114,#5737);
#4784=LINE('',#50139,#5738);
#4785=LINE('',#50164,#5739);
#4786=LINE('',#50188,#5740);
#4787=LINE('',#50213,#5741);
#4788=LINE('',#50238,#5742);
#4789=LINE('',#50262,#5743);
#4790=LINE('',#50286,#5744);
#4791=LINE('',#50311,#5745);
#4792=LINE('',#50336,#5746);
#4793=LINE('',#50360,#5747);
#4794=LINE('',#50385,#5748);
#4795=LINE('',#50410,#5749);
#4796=LINE('',#50434,#5750);
#4797=LINE('',#50458,#5751);
#4798=LINE('',#50483,#5752);
#4799=LINE('',#50508,#5753);
#4800=LINE('',#50532,#5754);
#4801=LINE('',#50557,#5755);
#4802=LINE('',#50582,#5756);
#4803=LINE('',#50606,#5757);
#4804=LINE('',#50630,#5758);
#4805=LINE('',#50655,#5759);
#4806=LINE('',#50680,#5760);
#4807=LINE('',#50704,#5761);
#4808=LINE('',#50729,#5762);
#4809=LINE('',#50754,#5763);
#4810=LINE('',#50778,#5764);
#4811=LINE('',#50802,#5765);
#4812=LINE('',#50827,#5766);
#4813=LINE('',#50852,#5767);
#4814=LINE('',#50876,#5768);
#4815=LINE('',#50901,#5769);
#4816=LINE('',#50926,#5770);
#4817=LINE('',#50950,#5771);
#4818=LINE('',#55880,#5772);
#4819=LINE('',#55891,#5773);
#4820=LINE('',#55893,#5774);
#4821=LINE('',#55894,#5775);
#4822=LINE('',#55897,#5776);
#4823=LINE('',#55898,#5777);
#4824=LINE('',#55901,#5778);
#4825=LINE('',#55902,#5779);
#4826=LINE('',#55905,#5780);
#4827=LINE('',#55907,#5781);
#4828=LINE('',#55908,#5782);
#4829=LINE('',#55911,#5783);
#4830=LINE('',#55913,#5784);
#4831=LINE('',#55920,#5785);
#4832=LINE('',#55927,#5786);
#4833=LINE('',#56317,#5787);
#4834=LINE('',#56326,#5788);
#4835=LINE('',#56328,#5789);
#4836=LINE('',#56344,#5790);
#4837=LINE('',#56347,#5791);
#4838=LINE('',#56369,#5792);
#4839=LINE('',#56401,#5793);
#4840=LINE('',#56402,#5794);
#4841=LINE('',#56434,#5795);
#4842=LINE('',#56435,#5796);
#4843=LINE('',#56442,#5797);
#4844=LINE('',#56443,#5798);
#4845=LINE('',#56475,#5799);
#4846=LINE('',#56476,#5800);
#4847=LINE('',#56483,#5801);
#4848=LINE('',#56484,#5802);
#4849=LINE('',#56491,#5803);
#4850=LINE('',#56492,#5804);
#4851=LINE('',#56509,#5805);
#4852=LINE('',#56526,#5806);
#4853=LINE('',#56530,#5807);
#4854=LINE('',#56533,#5808);
#4855=VECTOR('',#18795,10.);
#4856=VECTOR('',#18796,10.);
#4857=VECTOR('',#18797,10.);
#4858=VECTOR('',#18800,10.);
#4859=VECTOR('',#18801,10.);
#4860=VECTOR('',#18802,10.);
#4861=VECTOR('',#18803,10.);
#4862=VECTOR('',#18804,10.);
#4863=VECTOR('',#18805,10.);
#4864=VECTOR('',#18808,10.);
#4865=VECTOR('',#18809,10.);
#4866=VECTOR('',#18814,4.05);
#4867=VECTOR('',#18823,10.);
#4868=VECTOR('',#18824,10.);
#4869=VECTOR('',#18825,10.);
#4870=VECTOR('',#18828,10.);
#4871=VECTOR('',#18829,10.);
#4872=VECTOR('',#18830,10.);
#4873=VECTOR('',#18831,10.);
#4874=VECTOR('',#18832,10.);
#4875=VECTOR('',#18833,10.);
#4876=VECTOR('',#18836,10.);
#4877=VECTOR('',#18837,10.);
#4878=VECTOR('',#18842,4.05);
#4879=VECTOR('',#18853,4.3);
#4880=VECTOR('',#18858,10.);
#4881=VECTOR('',#18861,10.);
#4882=VECTOR('',#18864,10.);
#4883=VECTOR('',#18867,10.);
#4884=VECTOR('',#18874,4.3);
#4885=VECTOR('',#18879,4.3);
#4886=VECTOR('',#18884,10.);
#4887=VECTOR('',#18887,10.);
#4888=VECTOR('',#18890,10.);
#4889=VECTOR('',#18893,10.);
#4890=VECTOR('',#18902,4.05);
#4891=VECTOR('',#18907,4.3);
#4892=VECTOR('',#18912,4.05);
#4893=VECTOR('',#18949,41.);
#4894=VECTOR('',#18956,10.);
#4895=VECTOR('',#18957,10.);
#4896=VECTOR('',#18958,10.);
#4897=VECTOR('',#18959,10.);
#4898=VECTOR('',#18960,10.);
#4899=VECTOR('',#18961,10.);
#4900=VECTOR('',#18962,10.);
#4901=VECTOR('',#18963,10.);
#4902=VECTOR('',#18964,10.);
#4903=VECTOR('',#18965,10.);
#4904=VECTOR('',#18966,10.);
#4905=VECTOR('',#18967,10.);
#4906=VECTOR('',#18968,10.);
#4907=VECTOR('',#18969,10.);
#4908=VECTOR('',#18970,10.);
#4909=VECTOR('',#18971,10.);
#4910=VECTOR('',#18972,10.);
#4911=VECTOR('',#18973,10.);
#4912=VECTOR('',#18974,10.);
#4913=VECTOR('',#18975,10.);
#4914=VECTOR('',#18976,10.);
#4915=VECTOR('',#18977,10.);
#4916=VECTOR('',#18978,10.);
#4917=VECTOR('',#18979,10.);
#4918=VECTOR('',#18988,10.);
#4919=VECTOR('',#18989,10.);
#4920=VECTOR('',#18990,10.);
#4921=VECTOR('',#18991,10.);
#4922=VECTOR('',#19012,73.);
#4923=VECTOR('',#19023,10.);
#4924=VECTOR('',#19024,10.);
#4925=VECTOR('',#19025,10.);
#4926=VECTOR('',#19026,10.);
#4927=VECTOR('',#19069,10.);
#4928=VECTOR('',#19070,10.);
#4929=VECTOR('',#19081,10.);
#4930=VECTOR('',#19082,10.);
#4931=VECTOR('',#19085,10.);
#4932=VECTOR('',#19086,10.);
#4933=VECTOR('',#19087,10.);
#4934=VECTOR('',#19088,10.);
#4935=VECTOR('',#19089,10.);
#4936=VECTOR('',#19090,10.);
#4937=VECTOR('',#19095,10.);
#4938=VECTOR('',#19114,10.);
#4939=VECTOR('',#19125,10.);
#4940=VECTOR('',#19136,10.);
#4941=VECTOR('',#19143,10.);
#4942=VECTOR('',#19146,10.);
#4943=VECTOR('',#19149,10.);
#4944=VECTOR('',#19150,10.);
#4945=VECTOR('',#19159,10.);
#4946=VECTOR('',#19164,10.);
#4947=VECTOR('',#19179,10.);
#4948=VECTOR('',#19192,47.);
#4949=VECTOR('',#19197,10.);
#4950=VECTOR('',#19198,10.);
#4951=VECTOR('',#19201,10.);
#4952=VECTOR('',#19202,10.);
#4953=VECTOR('',#19213,7.);
#4954=VECTOR('',#19214,7.);
#4955=VECTOR('',#19227,10.);
#4956=VECTOR('',#19228,10.);
#4957=VECTOR('',#19231,10.);
#4958=VECTOR('',#19242,10.);
#4959=VECTOR('',#19243,10.);
#4960=VECTOR('',#19246,10.);
#4961=VECTOR('',#19247,10.);
#4962=VECTOR('',#19248,10.);
#4963=VECTOR('',#19251,10.);
#4964=VECTOR('',#19276,10.);
#4965=VECTOR('',#19287,10.);
#4966=VECTOR('',#19304,10.);
#4967=VECTOR('',#19307,10.);
#4968=VECTOR('',#19310,10.);
#4969=VECTOR('',#19311,10.);
#4970=VECTOR('',#19312,10.);
#4971=VECTOR('',#19313,10.);
#4972=VECTOR('',#19316,10.);
#4973=VECTOR('',#19323,10.);
#4974=VECTOR('',#19332,10.);
#4975=VECTOR('',#19333,10.);
#4976=VECTOR('',#19336,10.);
#4977=VECTOR('',#19431,4.5);
#4978=VECTOR('',#19434,4.5);
#4979=VECTOR('',#19437,4.5);
#4980=VECTOR('',#19440,4.5);
#4981=VECTOR('',#19443,4.5);
#4982=VECTOR('',#19446,4.5);
#4983=VECTOR('',#19449,13.05);
#4984=VECTOR('',#19458,11.);
#4985=VECTOR('',#19469,13.05);
#4986=VECTOR('',#19472,38.);
#4987=VECTOR('',#19479,10.);
#4988=VECTOR('',#19482,10.);
#4989=VECTOR('',#19485,10.);
#4990=VECTOR('',#19488,10.);
#4991=VECTOR('',#19489,10.);
#4992=VECTOR('',#19502,10.);
#4993=VECTOR('',#19509,10.);
#4994=VECTOR('',#19512,10.);
#4995=VECTOR('',#19515,10.);
#4996=VECTOR('',#19526,10.9267766952966);
#4997=VECTOR('',#19531,11.5);
#4998=VECTOR('',#19540,11.8232233047034);
#4999=VECTOR('',#19545,12.);
#5000=VECTOR('',#19550,69.7);
#5001=VECTOR('',#19557,70.);
#5002=VECTOR('',#19578,6.9);
#5003=VECTOR('',#19585,4.5);
#5004=VECTOR('',#19590,4.5);
#5005=VECTOR('',#19595,4.5);
#5006=VECTOR('',#19600,4.5);
#5007=VECTOR('',#19605,4.5);
#5008=VECTOR('',#19610,4.5);
#5009=VECTOR('',#19621,40.);
#5010=VECTOR('',#19626,47.5);
#5011=VECTOR('',#19635,69.5);
#5012=VECTOR('',#19638,8.05);
#5013=VECTOR('',#19645,12.9267766952966);
#5014=VECTOR('',#19650,13.5);
#5015=VECTOR('',#19659,13.8232233047034);
#5016=VECTOR('',#19670,69.7);
#5017=VECTOR('',#19693,70.);
#5018=VECTOR('',#19698,8.6);
#5019=VECTOR('',#19705,4.5);
#5020=VECTOR('',#19710,4.5);
#5021=VECTOR('',#19715,4.5);
#5022=VECTOR('',#19720,4.5);
#5023=VECTOR('',#19725,4.5);
#5024=VECTOR('',#19730,4.5);
#5025=VECTOR('',#19737,8.05);
#5026=VECTOR('',#19742,69.5);
#5027=VECTOR('',#19749,47.5);
#5028=VECTOR('',#19754,40.);
#5029=VECTOR('',#19765,4.5);
#5030=VECTOR('',#19772,4.5);
#5031=VECTOR('',#19779,4.5);
#5032=VECTOR('',#19786,4.5);
#5033=VECTOR('',#19793,4.5);
#5034=VECTOR('',#19800,4.5);
#5035=VECTOR('',#19807,8.5);
#5036=VECTOR('',#19818,70.);
#5037=VECTOR('',#19827,4.5);
#5038=VECTOR('',#19834,4.5);
#5039=VECTOR('',#19841,4.5);
#5040=VECTOR('',#19848,4.5);
#5041=VECTOR('',#19855,4.5);
#5042=VECTOR('',#19862,4.5);
#5043=VECTOR('',#19869,5.2);
#5044=VECTOR('',#19878,45.);
#5045=VECTOR('',#19889,70.);
#5046=VECTOR('',#19896,45.);
#5047=VECTOR('',#19909,28.9663172798364);
#5048=VECTOR('',#19920,29.5);
#5049=VECTOR('',#19925,5.1);
#5050=VECTOR('',#19930,30.);
#5051=VECTOR('',#19939,17.9940985792758);
#5052=VECTOR('',#19950,24.);
#5053=VECTOR('',#19957,5.215);
#5054=VECTOR('',#19968,5.1);
#5055=VECTOR('',#19975,5.215);
#5056=VECTOR('',#19978,30.);
#5057=VECTOR('',#19983,5.);
#5058=VECTOR('',#19988,5.);
#5059=VECTOR('',#19991,5.);
#5060=VECTOR('',#19994,5.);
#5061=VECTOR('',#19997,5.);
#5062=VECTOR('',#20000,5.);
#5063=VECTOR('',#20003,5.);
#5064=VECTOR('',#20006,5.);
#5065=VECTOR('',#20009,5.);
#5066=VECTOR('',#20012,5.);
#5067=VECTOR('',#20015,5.);
#5068=VECTOR('',#20018,5.);
#5069=VECTOR('',#20021,5.);
#5070=VECTOR('',#20024,5.);
#5071=VECTOR('',#20027,5.);
#5072=VECTOR('',#20030,4.0705);
#5073=VECTOR('',#20035,4.0705);
#5074=VECTOR('',#20038,4.0705);
#5075=VECTOR('',#20041,4.0705);
#5076=VECTOR('',#20044,4.0705);
#5077=VECTOR('',#20047,4.0705);
#5078=VECTOR('',#20050,4.0705);
#5079=VECTOR('',#20053,4.0705);
#5080=VECTOR('',#20056,4.0705);
#5081=VECTOR('',#20059,4.0705);
#5082=VECTOR('',#20062,4.0705);
#5083=VECTOR('',#20065,4.0705);
#5084=VECTOR('',#20068,4.0705);
#5085=VECTOR('',#20071,4.0705);
#5086=VECTOR('',#20074,4.0705);
#5087=VECTOR('',#20077,5.);
#5088=VECTOR('',#20082,5.);
#5089=VECTOR('',#20085,5.);
#5090=VECTOR('',#20088,5.);
#5091=VECTOR('',#20091,5.);
#5092=VECTOR('',#20094,5.);
#5093=VECTOR('',#20097,5.);
#5094=VECTOR('',#20100,5.);
#5095=VECTOR('',#20103,5.);
#5096=VECTOR('',#20106,5.);
#5097=VECTOR('',#20109,5.);
#5098=VECTOR('',#20112,5.);
#5099=VECTOR('',#20115,5.);
#5100=VECTOR('',#20118,5.);
#5101=VECTOR('',#20121,5.);
#5102=VECTOR('',#20124,4.0705);
#5103=VECTOR('',#20129,4.0705);
#5104=VECTOR('',#20132,4.0705);
#5105=VECTOR('',#20135,4.0705);
#5106=VECTOR('',#20138,4.0705);
#5107=VECTOR('',#20141,4.0705);
#5108=VECTOR('',#20144,4.0705);
#5109=VECTOR('',#20147,4.0705);
#5110=VECTOR('',#20150,4.0705);
#5111=VECTOR('',#20153,4.0705);
#5112=VECTOR('',#20156,4.0705);
#5113=VECTOR('',#20159,4.0705);
#5114=VECTOR('',#20162,4.0705);
#5115=VECTOR('',#20165,4.0705);
#5116=VECTOR('',#20168,4.0705);
#5117=VECTOR('',#20199,4.75);
#5118=VECTOR('',#20212,8.);
#5119=VECTOR('',#20219,4.75);
#5120=VECTOR('',#20228,7.580184099288);
#5121=VECTOR('',#20259,10.);
#5122=VECTOR('',#20262,10.);
#5123=VECTOR('',#20265,10.);
#5124=VECTOR('',#20268,10.);
#5125=VECTOR('',#20271,10.);
#5126=VECTOR('',#20274,10.);
#5127=VECTOR('',#20277,10.);
#5128=VECTOR('',#20278,10.);
#5129=VECTOR('',#20281,10.);
#5130=VECTOR('',#20282,10.);
#5131=VECTOR('',#20285,10.);
#5132=VECTOR('',#20286,10.);
#5133=VECTOR('',#20289,10.);
#5134=VECTOR('',#20290,10.);
#5135=VECTOR('',#20293,10.);
#5136=VECTOR('',#20294,10.);
#5137=VECTOR('',#20297,10.);
#5138=VECTOR('',#20298,10.);
#5139=VECTOR('',#20309,8.83380215351701);
#5140=VECTOR('',#20314,5.25);
#5141=VECTOR('',#20319,5.05);
#5142=VECTOR('',#20324,5.25);
#5143=VECTOR('',#20339,10.25);
#5144=VECTOR('',#20350,10.);
#5145=VECTOR('',#20351,10.);
#5146=VECTOR('',#20352,10.);
#5147=VECTOR('',#20367,10.8);
#5148=VECTOR('',#20378,10.55);
#5149=VECTOR('',#20387,17.);
#5150=VECTOR('',#20414,17.);
#5151=VECTOR('',#20435,10.);
#5152=VECTOR('',#20438,10.);
#5153=VECTOR('',#20451,10.);
#5154=VECTOR('',#20452,10.);
#5155=VECTOR('',#20465,10.);
#5156=VECTOR('',#20466,10.);
#5157=VECTOR('',#20479,10.);
#5158=VECTOR('',#20480,10.);
#5159=VECTOR('',#20489,10.);
#5160=VECTOR('',#20492,10.);
#5161=VECTOR('',#20495,10.);
#5162=VECTOR('',#20496,10.);
#5163=VECTOR('',#20499,10.);
#5164=VECTOR('',#20504,10.);
#5165=VECTOR('',#20505,10.);
#5166=VECTOR('',#20520,10.);
#5167=VECTOR('',#20533,10.);
#5168=VECTOR('',#20544,10.);
#5169=VECTOR('',#20545,10.);
#5170=VECTOR('',#20558,10.);
#5171=VECTOR('',#20559,10.);
#5172=VECTOR('',#20568,10.);
#5173=VECTOR('',#20569,10.);
#5174=VECTOR('',#20572,10.);
#5175=VECTOR('',#20585,10.);
#5176=VECTOR('',#20588,10.);
#5177=VECTOR('',#20601,10.);
#5178=VECTOR('',#20602,10.);
#5179=VECTOR('',#20615,10.);
#5180=VECTOR('',#20616,10.);
#5181=VECTOR('',#20629,10.);
#5182=VECTOR('',#20630,10.);
#5183=VECTOR('',#20639,10.);
#5184=VECTOR('',#20642,10.);
#5185=VECTOR('',#20645,10.);
#5186=VECTOR('',#20646,10.);
#5187=VECTOR('',#20649,10.);
#5188=VECTOR('',#20654,10.);
#5189=VECTOR('',#20655,10.);
#5190=VECTOR('',#20670,10.);
#5191=VECTOR('',#20683,10.);
#5192=VECTOR('',#20694,10.);
#5193=VECTOR('',#20695,10.);
#5194=VECTOR('',#20708,10.);
#5195=VECTOR('',#20709,10.);
#5196=VECTOR('',#20718,10.);
#5197=VECTOR('',#20719,10.);
#5198=VECTOR('',#20722,10.);
#5199=VECTOR('',#20745,4.5);
#5200=VECTOR('',#20748,4.5);
#5201=VECTOR('',#20751,4.5);
#5202=VECTOR('',#20754,4.5);
#5203=VECTOR('',#20757,10.);
#5204=VECTOR('',#20760,10.);
#5205=VECTOR('',#20763,12.05);
#5206=VECTOR('',#20772,14.);
#5207=VECTOR('',#20779,14.);
#5208=VECTOR('',#20782,14.);
#5209=VECTOR('',#20787,12.);
#5210=VECTOR('',#20792,12.);
#5211=VECTOR('',#20795,12.);
#5212=VECTOR('',#20798,12.);
#5213=VECTOR('',#20801,12.);
#5214=VECTOR('',#20804,12.);
#5215=VECTOR('',#20807,11.06595);
#5216=VECTOR('',#20812,11.06595);
#5217=VECTOR('',#20817,11.06595);
#5218=VECTOR('',#20820,11.06595);
#5219=VECTOR('',#20823,11.06595);
#5220=VECTOR('',#20826,11.06595);
#5221=VECTOR('',#20831,15.75);
#5222=VECTOR('',#20838,16.);
#5223=VECTOR('',#20849,15.8232233047034);
#5224=VECTOR('',#20856,15.5);
#5225=VECTOR('',#20863,14.9267766952966);
#5226=VECTOR('',#20868,10.);
#5227=VECTOR('',#20869,10.);
#5228=VECTOR('',#20870,10.);
#5229=VECTOR('',#20871,10.);
#5230=VECTOR('',#20872,10.);
#5231=VECTOR('',#20873,10.);
#5232=VECTOR('',#20876,10.);
#5233=VECTOR('',#20877,10.);
#5234=VECTOR('',#20878,10.);
#5235=VECTOR('',#20881,10.);
#5236=VECTOR('',#20882,10.);
#5237=VECTOR('',#20885,10.);
#5238=VECTOR('',#20886,10.);
#5239=VECTOR('',#20887,10.);
#5240=VECTOR('',#20890,10.);
#5241=VECTOR('',#20891,10.);
#5242=VECTOR('',#20894,10.);
#5243=VECTOR('',#20897,10.);
#5244=VECTOR('',#20900,10.);
#5245=VECTOR('',#20901,10.);
#5246=VECTOR('',#20902,10.);
#5247=VECTOR('',#20905,10.);
#5248=VECTOR('',#20906,10.);
#5249=VECTOR('',#20909,10.);
#5250=VECTOR('',#20910,10.);
#5251=VECTOR('',#20925,10.);
#5252=VECTOR('',#20926,10.);
#5253=VECTOR('',#20929,10.);
#5254=VECTOR('',#20930,10.);
#5255=VECTOR('',#20933,10.);
#5256=VECTOR('',#20940,11.75);
#5257=VECTOR('',#20949,10.);
#5258=VECTOR('',#20952,10.);
#5259=VECTOR('',#20955,10.);
#5260=VECTOR('',#20958,10.);
#5261=VECTOR('',#20963,10.);
#5262=VECTOR('',#20964,10.);
#5263=VECTOR('',#20965,10.);
#5264=VECTOR('',#20970,10.);
#5265=VECTOR('',#20973,10.);
#5266=VECTOR('',#20974,10.);
#5267=VECTOR('',#20979,10.);
#5268=VECTOR('',#20982,10.);
#5269=VECTOR('',#20983,10.);
#5270=VECTOR('',#20988,10.);
#5271=VECTOR('',#20991,10.);
#5272=VECTOR('',#20992,10.);
#5273=VECTOR('',#21001,3.);
#5274=VECTOR('',#21010,10.);
#5275=VECTOR('',#21011,10.);
#5276=VECTOR('',#21012,10.);
#5277=VECTOR('',#21013,10.);
#5278=VECTOR('',#21014,10.);
#5279=VECTOR('',#21015,10.);
#5280=VECTOR('',#21016,10.);
#5281=VECTOR('',#21023,5.6);
#5282=VECTOR('',#21028,10.);
#5283=VECTOR('',#21033,10.);
#5284=VECTOR('',#21038,10.);
#5285=VECTOR('',#21043,10.);
#5286=VECTOR('',#21054,10.);
#5287=VECTOR('',#21061,9.);
#5288=VECTOR('',#21078,8.5);
#5289=VECTOR('',#21083,10.);
#5290=VECTOR('',#21084,10.);
#5291=VECTOR('',#21087,10.);
#5292=VECTOR('',#21090,10.);
#5293=VECTOR('',#21091,10.);
#5294=VECTOR('',#21094,10.);
#5295=VECTOR('',#21097,10.);
#5296=VECTOR('',#21098,10.);
#5297=VECTOR('',#21101,10.);
#5298=VECTOR('',#21102,10.);
#5299=VECTOR('',#21103,10.);
#5300=VECTOR('',#21104,10.);
#5301=VECTOR('',#21105,10.);
#5302=VECTOR('',#21110,10.);
#5303=VECTOR('',#21111,10.);
#5304=VECTOR('',#21114,10.);
#5305=VECTOR('',#21115,10.);
#5306=VECTOR('',#21118,10.);
#5307=VECTOR('',#21121,10.);
#5308=VECTOR('',#21134,6.65);
#5309=VECTOR('',#21137,6.8);
#5310=VECTOR('',#21142,10.);
#5311=VECTOR('',#21143,10.);
#5312=VECTOR('',#21144,10.);
#5313=VECTOR('',#21147,10.);
#5314=VECTOR('',#21148,10.);
#5315=VECTOR('',#21149,10.);
#5316=VECTOR('',#21152,10.);
#5317=VECTOR('',#21153,10.);
#5318=VECTOR('',#21154,10.);
#5319=VECTOR('',#21157,10.);
#5320=VECTOR('',#21158,10.);
#5321=VECTOR('',#21161,10.);
#5322=VECTOR('',#21162,10.);
#5323=VECTOR('',#21163,10.);
#5324=VECTOR('',#21166,10.);
#5325=VECTOR('',#21167,10.);
#5326=VECTOR('',#21168,10.);
#5327=VECTOR('',#21171,10.);
#5328=VECTOR('',#21172,10.);
#5329=VECTOR('',#21173,10.);
#5330=VECTOR('',#21176,10.);
#5331=VECTOR('',#21177,10.);
#5332=VECTOR('',#21180,10.);
#5333=VECTOR('',#21181,10.);
#5334=VECTOR('',#21184,10.);
#5335=VECTOR('',#21185,10.);
#5336=VECTOR('',#21186,10.);
#5337=VECTOR('',#21189,10.);
#5338=VECTOR('',#21190,10.);
#5339=VECTOR('',#21191,10.);
#5340=VECTOR('',#21194,10.);
#5341=VECTOR('',#21195,10.);
#5342=VECTOR('',#21198,10.);
#5343=VECTOR('',#21199,10.);
#5344=VECTOR('',#21202,10.);
#5345=VECTOR('',#21203,10.);
#5346=VECTOR('',#21204,10.);
#5347=VECTOR('',#21207,10.);
#5348=VECTOR('',#21208,10.);
#5349=VECTOR('',#21209,10.);
#5350=VECTOR('',#21212,10.);
#5351=VECTOR('',#21213,10.);
#5352=VECTOR('',#21216,10.);
#5353=VECTOR('',#21217,10.);
#5354=VECTOR('',#21218,10.);
#5355=VECTOR('',#21221,10.);
#5356=VECTOR('',#21222,10.);
#5357=VECTOR('',#21223,10.);
#5358=VECTOR('',#21226,10.);
#5359=VECTOR('',#21229,10.);
#5360=VECTOR('',#21232,10.);
#5361=VECTOR('',#21243,11.8232233047034);
#5362=VECTOR('',#21250,11.25);
#5363=VECTOR('',#21259,12.);
#5364=VECTOR('',#21262,10.4267766952966);
#5365=VECTOR('',#21271,11.75);
#5366=VECTOR('',#21278,12.);
#5367=VECTOR('',#21283,10.);
#5368=VECTOR('',#21284,10.);
#5369=VECTOR('',#21285,10.);
#5370=VECTOR('',#21298,11.);
#5371=VECTOR('',#21303,12.);
#5372=VECTOR('',#21314,11.);
#5373=VECTOR('',#21325,8.5);
#5374=VECTOR('',#21330,8.35);
#5375=VECTOR('',#21345,6.);
#5376=VECTOR('',#21356,12.75);
#5377=VECTOR('',#21361,13.);
#5378=VECTOR('',#21366,12.75);
#5379=VECTOR('',#21375,3.75);
#5380=VECTOR('',#21380,10.);
#5381=VECTOR('',#21381,10.);
#5382=VECTOR('',#21382,10.);
#5383=VECTOR('',#21383,10.);
#5384=VECTOR('',#21398,3.5);
#5385=VECTOR('',#21401,3.75);
#5386=VECTOR('',#21408,3.5);
#5387=VECTOR('',#21411,10.);
#5388=VECTOR('',#21412,10.);
#5389=VECTOR('',#21413,10.);
#5390=VECTOR('',#21414,10.);
#5391=VECTOR('',#21419,10.);
#5392=VECTOR('',#21424,10.);
#5393=VECTOR('',#21425,10.);
#5394=VECTOR('',#21426,10.);
#5395=VECTOR('',#21431,10.);
#5396=VECTOR('',#21436,10.);
#5397=VECTOR('',#21437,10.);
#5398=VECTOR('',#21438,10.);
#5399=VECTOR('',#21443,10.);
#5400=VECTOR('',#21448,10.);
#5401=VECTOR('',#21449,10.);
#5402=VECTOR('',#21450,10.);
#5403=VECTOR('',#21455,10.);
#5404=VECTOR('',#21460,10.);
#5405=VECTOR('',#21461,10.);
#5406=VECTOR('',#21466,10.);
#5407=VECTOR('',#21471,10.);
#5408=VECTOR('',#21472,10.);
#5409=VECTOR('',#21473,10.);
#5410=VECTOR('',#21478,10.);
#5411=VECTOR('',#21483,10.);
#5412=VECTOR('',#21484,10.);
#5413=VECTOR('',#21485,10.);
#5414=VECTOR('',#21490,10.);
#5415=VECTOR('',#21495,10.);
#5416=VECTOR('',#21496,10.);
#5417=VECTOR('',#21497,10.);
#5418=VECTOR('',#21506,10.);
#5419=VECTOR('',#21511,10.);
#5420=VECTOR('',#21512,10.);
#5421=VECTOR('',#21515,10.);
#5422=VECTOR('',#21520,10.);
#5423=VECTOR('',#21521,10.);
#5424=VECTOR('',#21524,10.);
#5425=VECTOR('',#21529,10.);
#5426=VECTOR('',#21530,10.);
#5427=VECTOR('',#21533,10.);
#5428=VECTOR('',#21538,10.);
#5429=VECTOR('',#21539,10.);
#5430=VECTOR('',#21556,10.);
#5431=VECTOR('',#21557,10.);
#5432=VECTOR('',#21558,10.);
#5433=VECTOR('',#21563,10.);
#5434=VECTOR('',#21568,10.);
#5435=VECTOR('',#21569,10.);
#5436=VECTOR('',#21570,10.);
#5437=VECTOR('',#21575,10.);
#5438=VECTOR('',#21580,10.);
#5439=VECTOR('',#21581,10.);
#5440=VECTOR('',#21582,10.);
#5441=VECTOR('',#21587,10.);
#5442=VECTOR('',#21592,10.);
#5443=VECTOR('',#21593,10.);
#5444=VECTOR('',#21594,10.);
#5445=VECTOR('',#21599,10.);
#5446=VECTOR('',#21604,10.);
#5447=VECTOR('',#21605,10.);
#5448=VECTOR('',#21608,10.);
#5449=VECTOR('',#21613,10.);
#5450=VECTOR('',#21614,10.);
#5451=VECTOR('',#21617,10.);
#5452=VECTOR('',#21622,10.);
#5453=VECTOR('',#21623,10.);
#5454=VECTOR('',#21626,10.);
#5455=VECTOR('',#21631,10.);
#5456=VECTOR('',#21632,10.);
#5457=VECTOR('',#21639,10.);
#5458=VECTOR('',#21642,10.);
#5459=VECTOR('',#21645,10.);
#5460=VECTOR('',#21648,10.);
#5461=VECTOR('',#21651,10.);
#5462=VECTOR('',#21654,10.);
#5463=VECTOR('',#21661,3.75);
#5464=VECTOR('',#21664,3.75);
#5465=VECTOR('',#21667,4.5);
#5466=VECTOR('',#21670,4.5);
#5467=VECTOR('',#21673,4.5);
#5468=VECTOR('',#21676,4.5);
#5469=VECTOR('',#21681,4.);
#5470=VECTOR('',#21686,4.);
#5471=VECTOR('',#21689,4.);
#5472=VECTOR('',#21692,4.);
#5473=VECTOR('',#21695,4.);
#5474=VECTOR('',#21698,4.);
#5475=VECTOR('',#21701,4.);
#5476=VECTOR('',#21704,4.);
#5477=VECTOR('',#21707,4.);
#5478=VECTOR('',#21710,4.);
#5479=VECTOR('',#21715,3.22275);
#5480=VECTOR('',#21720,3.22275);
#5481=VECTOR('',#21723,3.22275);
#5482=VECTOR('',#21726,3.22275);
#5483=VECTOR('',#21729,3.22275);
#5484=VECTOR('',#21732,3.22275);
#5485=VECTOR('',#21735,3.22275);
#5486=VECTOR('',#21738,3.22275);
#5487=VECTOR('',#21741,3.22275);
#5488=VECTOR('',#21748,9.82322330470336);
#5489=VECTOR('',#21755,9.5);
#5490=VECTOR('',#21764,10.);
#5491=VECTOR('',#21767,8.92677669529664);
#5492=VECTOR('',#21788,9.);
#5493=VECTOR('',#21795,3.75);
#5494=VECTOR('',#21802,4.);
#5495=VECTOR('',#21807,4.);
#5496=VECTOR('',#21810,4.);
#5497=VECTOR('',#21813,4.);
#5498=VECTOR('',#21816,4.);
#5499=VECTOR('',#21819,4.);
#5500=VECTOR('',#21822,4.);
#5501=VECTOR('',#21825,4.);
#5502=VECTOR('',#21828,4.);
#5503=VECTOR('',#21831,4.);
#5504=VECTOR('',#21834,4.);
#5505=VECTOR('',#21837,4.);
#5506=VECTOR('',#21840,4.);
#5507=VECTOR('',#21843,4.);
#5508=VECTOR('',#21846,4.);
#5509=VECTOR('',#21849,4.);
#5510=VECTOR('',#21852,4.);
#5511=VECTOR('',#21855,4.);
#5512=VECTOR('',#21858,4.);
#5513=VECTOR('',#21861,4.);
#5514=VECTOR('',#21864,4.);
#5515=VECTOR('',#21867,4.);
#5516=VECTOR('',#21870,4.);
#5517=VECTOR('',#21873,4.);
#5518=VECTOR('',#21876,4.);
#5519=VECTOR('',#21879,4.);
#5520=VECTOR('',#21882,4.);
#5521=VECTOR('',#21885,4.);
#5522=VECTOR('',#21888,4.);
#5523=VECTOR('',#21891,4.);
#5524=VECTOR('',#21894,4.);
#5525=VECTOR('',#21897,4.);
#5526=VECTOR('',#21900,4.);
#5527=VECTOR('',#21903,4.);
#5528=VECTOR('',#21906,4.);
#5529=VECTOR('',#21909,4.);
#5530=VECTOR('',#21912,4.);
#5531=VECTOR('',#21915,4.);
#5532=VECTOR('',#21918,4.);
#5533=VECTOR('',#21921,4.);
#5534=VECTOR('',#21924,4.);
#5535=VECTOR('',#21927,4.);
#5536=VECTOR('',#21930,4.);
#5537=VECTOR('',#21933,4.);
#5538=VECTOR('',#21936,3.22275);
#5539=VECTOR('',#21941,3.22275);
#5540=VECTOR('',#21946,3.22275);
#5541=VECTOR('',#21949,3.22275);
#5542=VECTOR('',#21952,3.22275);
#5543=VECTOR('',#21955,3.22275);
#5544=VECTOR('',#21958,3.22275);
#5545=VECTOR('',#21961,3.22275);
#5546=VECTOR('',#21964,3.22275);
#5547=VECTOR('',#21967,3.22275);
#5548=VECTOR('',#21970,3.22275);
#5549=VECTOR('',#21973,3.22275);
#5550=VECTOR('',#21976,3.22275);
#5551=VECTOR('',#21979,3.22275);
#5552=VECTOR('',#21982,3.22275);
#5553=VECTOR('',#21985,3.22275);
#5554=VECTOR('',#21988,3.22275);
#5555=VECTOR('',#21991,3.22275);
#5556=VECTOR('',#21994,3.22275);
#5557=VECTOR('',#21997,3.22275);
#5558=VECTOR('',#22000,3.22275);
#5559=VECTOR('',#22003,3.22275);
#5560=VECTOR('',#22006,3.22275);
#5561=VECTOR('',#22009,3.22275);
#5562=VECTOR('',#22012,3.22275);
#5563=VECTOR('',#22015,3.22275);
#5564=VECTOR('',#22018,3.22275);
#5565=VECTOR('',#22021,3.22275);
#5566=VECTOR('',#22024,3.22275);
#5567=VECTOR('',#22027,3.22275);
#5568=VECTOR('',#22030,3.22275);
#5569=VECTOR('',#22033,3.22275);
#5570=VECTOR('',#22036,3.22275);
#5571=VECTOR('',#22039,3.22275);
#5572=VECTOR('',#22042,3.22275);
#5573=VECTOR('',#22045,3.22275);
#5574=VECTOR('',#22048,3.22275);
#5575=VECTOR('',#22051,3.22275);
#5576=VECTOR('',#22054,3.22275);
#5577=VECTOR('',#22057,3.22275);
#5578=VECTOR('',#22060,3.22275);
#5579=VECTOR('',#22063,3.22275);
#5580=VECTOR('',#22066,3.22275);
#5581=VECTOR('',#22069,3.22275);
#5582=VECTOR('',#22082,7.25527674973257);
#5583=VECTOR('',#22087,10.);
#5584=VECTOR('',#22088,10.);
#5585=VECTOR('',#22089,10.);
#5586=VECTOR('',#22092,10.);
#5587=VECTOR('',#22093,10.);
#5588=VECTOR('',#22096,10.);
#5589=VECTOR('',#22097,10.);
#5590=VECTOR('',#22100,10.);
#5591=VECTOR('',#22101,10.);
#5592=VECTOR('',#22102,10.);
#5593=VECTOR('',#22107,10.);
#5594=VECTOR('',#22110,10.);
#5595=VECTOR('',#22121,3.75);
#5596=VECTOR('',#22128,4.);
#5597=VECTOR('',#22133,4.);
#5598=VECTOR('',#22136,4.);
#5599=VECTOR('',#22139,4.);
#5600=VECTOR('',#22142,4.);
#5601=VECTOR('',#22145,4.);
#5602=VECTOR('',#22148,4.);
#5603=VECTOR('',#22151,4.);
#5604=VECTOR('',#22154,4.);
#5605=VECTOR('',#22157,4.);
#5606=VECTOR('',#22160,4.);
#5607=VECTOR('',#22163,4.);
#5608=VECTOR('',#22166,4.);
#5609=VECTOR('',#22169,4.);
#5610=VECTOR('',#22172,4.);
#5611=VECTOR('',#22175,4.);
#5612=VECTOR('',#22178,4.);
#5613=VECTOR('',#22181,4.);
#5614=VECTOR('',#22184,4.);
#5615=VECTOR('',#22187,4.);
#5616=VECTOR('',#22190,4.);
#5617=VECTOR('',#22193,4.);
#5618=VECTOR('',#22196,4.);
#5619=VECTOR('',#22199,4.);
#5620=VECTOR('',#22202,4.);
#5621=VECTOR('',#22205,4.);
#5622=VECTOR('',#22208,4.);
#5623=VECTOR('',#22211,4.);
#5624=VECTOR('',#22214,4.);
#5625=VECTOR('',#22217,4.);
#5626=VECTOR('',#22220,4.);
#5627=VECTOR('',#22223,4.);
#5628=VECTOR('',#22226,4.);
#5629=VECTOR('',#22229,4.);
#5630=VECTOR('',#22232,4.);
#5631=VECTOR('',#22235,4.);
#5632=VECTOR('',#22238,4.);
#5633=VECTOR('',#22241,4.);
#5634=VECTOR('',#22244,4.);
#5635=VECTOR('',#22247,4.);
#5636=VECTOR('',#22250,4.);
#5637=VECTOR('',#22253,4.);
#5638=VECTOR('',#22256,4.);
#5639=VECTOR('',#22259,4.);
#5640=VECTOR('',#22262,4.);
#5641=VECTOR('',#22265,4.);
#5642=VECTOR('',#22268,4.);
#5643=VECTOR('',#22271,4.);
#5644=VECTOR('',#22274,4.);
#5645=VECTOR('',#22277,4.);
#5646=VECTOR('',#22280,4.);
#5647=VECTOR('',#22283,4.);
#5648=VECTOR('',#22286,4.);
#5649=VECTOR('',#22289,4.);
#5650=VECTOR('',#22292,4.);
#5651=VECTOR('',#22295,4.);
#5652=VECTOR('',#22298,4.);
#5653=VECTOR('',#22301,4.);
#5654=VECTOR('',#22304,4.);
#5655=VECTOR('',#22307,4.);
#5656=VECTOR('',#22310,4.);
#5657=VECTOR('',#22313,4.);
#5658=VECTOR('',#22316,4.);
#5659=VECTOR('',#22319,4.);
#5660=VECTOR('',#22322,4.);
#5661=VECTOR('',#22325,4.);
#5662=VECTOR('',#22328,4.);
#5663=VECTOR('',#22331,4.);
#5664=VECTOR('',#22334,4.);
#5665=VECTOR('',#22337,4.);
#5666=VECTOR('',#22340,4.);
#5667=VECTOR('',#22343,4.);
#5668=VECTOR('',#22346,4.);
#5669=VECTOR('',#22349,4.);
#5670=VECTOR('',#22352,4.);
#5671=VECTOR('',#22355,4.);
#5672=VECTOR('',#22358,4.);
#5673=VECTOR('',#22361,4.);
#5674=VECTOR('',#22364,4.);
#5675=VECTOR('',#22367,4.);
#5676=VECTOR('',#22370,4.);
#5677=VECTOR('',#22373,4.);
#5678=VECTOR('',#22376,4.);
#5679=VECTOR('',#22379,4.);
#5680=VECTOR('',#22382,4.);
#5681=VECTOR('',#22385,4.);
#5682=VECTOR('',#22388,4.);
#5683=VECTOR('',#22391,4.);
#5684=VECTOR('',#22394,3.22275);
#5685=VECTOR('',#22399,3.22275);
#5686=VECTOR('',#22404,3.22275);
#5687=VECTOR('',#22407,3.22275);
#5688=VECTOR('',#22410,3.22275);
#5689=VECTOR('',#22413,3.22275);
#5690=VECTOR('',#22416,3.22275);
#5691=VECTOR('',#22419,3.22275);
#5692=VECTOR('',#22422,3.22275);
#5693=VECTOR('',#22425,3.22275);
#5694=VECTOR('',#22428,3.22275);
#5695=VECTOR('',#22431,3.22275);
#5696=VECTOR('',#22434,3.22275);
#5697=VECTOR('',#22437,3.22275);
#5698=VECTOR('',#22440,3.22275);
#5699=VECTOR('',#22443,3.22275);
#5700=VECTOR('',#22446,3.22275);
#5701=VECTOR('',#22449,3.22275);
#5702=VECTOR('',#22452,3.22275);
#5703=VECTOR('',#22455,3.22275);
#5704=VECTOR('',#22458,3.22275);
#5705=VECTOR('',#22461,3.22275);
#5706=VECTOR('',#22464,3.22275);
#5707=VECTOR('',#22467,3.22275);
#5708=VECTOR('',#22470,3.22275);
#5709=VECTOR('',#22473,3.22275);
#5710=VECTOR('',#22476,3.22275);
#5711=VECTOR('',#22479,3.22275);
#5712=VECTOR('',#22482,3.22275);
#5713=VECTOR('',#22485,3.22275);
#5714=VECTOR('',#22488,3.22275);
#5715=VECTOR('',#22491,3.22275);
#5716=VECTOR('',#22494,3.22275);
#5717=VECTOR('',#22497,3.22275);
#5718=VECTOR('',#22500,3.22275);
#5719=VECTOR('',#22503,3.22275);
#5720=VECTOR('',#22506,3.22275);
#5721=VECTOR('',#22509,3.22275);
#5722=VECTOR('',#22512,3.22275);
#5723=VECTOR('',#22515,3.22275);
#5724=VECTOR('',#22518,3.22275);
#5725=VECTOR('',#22521,3.22275);
#5726=VECTOR('',#22524,3.22275);
#5727=VECTOR('',#22527,3.22275);
#5728=VECTOR('',#22530,3.22275);
#5729=VECTOR('',#22533,3.22275);
#5730=VECTOR('',#22536,3.22275);
#5731=VECTOR('',#22539,3.22275);
#5732=VECTOR('',#22542,3.22275);
#5733=VECTOR('',#22545,3.22275);
#5734=VECTOR('',#22548,3.22275);
#5735=VECTOR('',#22551,3.22275);
#5736=VECTOR('',#22554,3.22275);
#5737=VECTOR('',#22557,3.22275);
#5738=VECTOR('',#22560,3.22275);
#5739=VECTOR('',#22563,3.22275);
#5740=VECTOR('',#22566,3.22275);
#5741=VECTOR('',#22569,3.22275);
#5742=VECTOR('',#22572,3.22275);
#5743=VECTOR('',#22575,3.22275);
#5744=VECTOR('',#22578,3.22275);
#5745=VECTOR('',#22581,3.22275);
#5746=VECTOR('',#22584,3.22275);
#5747=VECTOR('',#22587,3.22275);
#5748=VECTOR('',#22590,3.22275);
#5749=VECTOR('',#22593,3.22275);
#5750=VECTOR('',#22596,3.22275);
#5751=VECTOR('',#22599,3.22275);
#5752=VECTOR('',#22602,3.22275);
#5753=VECTOR('',#22605,3.22275);
#5754=VECTOR('',#22608,3.22275);
#5755=VECTOR('',#22611,3.22275);
#5756=VECTOR('',#22614,3.22275);
#5757=VECTOR('',#22617,3.22275);
#5758=VECTOR('',#22620,3.22275);
#5759=VECTOR('',#22623,3.22275);
#5760=VECTOR('',#22626,3.22275);
#5761=VECTOR('',#22629,3.22275);
#5762=VECTOR('',#22632,3.22275);
#5763=VECTOR('',#22635,3.22275);
#5764=VECTOR('',#22638,3.22275);
#5765=VECTOR('',#22641,3.22275);
#5766=VECTOR('',#22644,3.22275);
#5767=VECTOR('',#22647,3.22275);
#5768=VECTOR('',#22650,3.22275);
#5769=VECTOR('',#22653,3.22275);
#5770=VECTOR('',#22656,3.22275);
#5771=VECTOR('',#22659,3.22275);
#5772=VECTOR('',#22672,7.25527674973257);
#5773=VECTOR('',#22677,10.);
#5774=VECTOR('',#22678,10.);
#5775=VECTOR('',#22679,10.);
#5776=VECTOR('',#22682,10.);
#5777=VECTOR('',#22683,10.);
#5778=VECTOR('',#22686,10.);
#5779=VECTOR('',#22687,10.);
#5780=VECTOR('',#22690,10.);
#5781=VECTOR('',#22691,10.);
#5782=VECTOR('',#22692,10.);
#5783=VECTOR('',#22697,10.);
#5784=VECTOR('',#22700,10.);
#5785=VECTOR('',#22711,3.75);
#5786=VECTOR('',#22720,6.15985379710312);
#5787=VECTOR('',#22751,10.);
#5788=VECTOR('',#22754,10.);
#5789=VECTOR('',#22757,10.);
#5790=VECTOR('',#22760,10.);
#5791=VECTOR('',#22763,10.);
#5792=VECTOR('',#22766,10.);
#5793=VECTOR('',#22769,10.);
#5794=VECTOR('',#22770,10.);
#5795=VECTOR('',#22773,10.);
#5796=VECTOR('',#22774,10.);
#5797=VECTOR('',#22777,10.);
#5798=VECTOR('',#22778,10.);
#5799=VECTOR('',#22781,10.);
#5800=VECTOR('',#22782,10.);
#5801=VECTOR('',#22785,10.);
#5802=VECTOR('',#22786,10.);
#5803=VECTOR('',#22789,10.);
#5804=VECTOR('',#22790,10.);
#5805=VECTOR('',#22801,7.25527674973257);
#5806=VECTOR('',#22806,4.25);
#5807=VECTOR('',#22811,4.05);
#5808=VECTOR('',#22816,4.25);
#5809=B_SPLINE_CURVE_WITH_KNOTS('',3,(#22946,#22947,#22948,#22949,#22950,
#22951,#22952,#22953),.UNSPECIFIED.,.F.,.F.,(4,2,2,4),(0.589540352546839,
0.67637836992065,0.709007118931895,0.73245734358678),.UNSPECIFIED.);
#5810=B_SPLINE_CURVE_WITH_KNOTS('',3,(#22963,#22964,#22965,#22966,#22967,
#22968,#22969,#22970),.UNSPECIFIED.,.F.,.F.,(4,2,2,4),(0.766228943549322,
0.796165087029866,0.888720170530452,0.980335690408468),.UNSPECIFIED.);
#5811=B_SPLINE_CURVE_WITH_KNOTS('',3,(#22984,#22985,#22986,#22987,#22988,
#22989,#22990,#22991),.UNSPECIFIED.,.F.,.F.,(4,2,2,4),(0.313128211350458,
0.404743731228475,0.49729881472906,0.527234958209604),.UNSPECIFIED.);
#5812=B_SPLINE_CURVE_WITH_KNOTS('',3,(#22995,#22996,#22997,#22998,#22999,
#23000,#23001,#23002),.UNSPECIFIED.,.F.,.F.,(4,2,2,4),(0.732457343586781,
0.755907568241666,0.788536317252911,0.875374334626722),.UNSPECIFIED.);
#5813=B_SPLINE_CURVE_WITH_KNOTS('',3,(#23017,#23018,#23019,#23020,#23021,
#23022,#23023,#23024),.UNSPECIFIED.,.F.,.F.,(4,2,2,4),(0.589540352546839,
0.67637836992065,0.709007118931895,0.73245734358678),.UNSPECIFIED.);
#5814=B_SPLINE_CURVE_WITH_KNOTS('',3,(#23034,#23035,#23036,#23037,#23038,
#23039,#23040,#23041),.UNSPECIFIED.,.F.,.F.,(4,2,2,4),(0.766228943549322,
0.796165087029866,0.888720170530452,0.980335690408468),.UNSPECIFIED.);
#5815=B_SPLINE_CURVE_WITH_KNOTS('',3,(#23055,#23056,#23057,#23058,#23059,
#23060,#23061,#23062),.UNSPECIFIED.,.F.,.F.,(4,2,2,4),(0.313128211350458,
0.404743731228475,0.49729881472906,0.527234958209605),.UNSPECIFIED.);
#5816=B_SPLINE_CURVE_WITH_KNOTS('',3,(#23066,#23067,#23068,#23069,#23070,
#23071,#23072,#23073),.UNSPECIFIED.,.F.,.F.,(4,2,2,4),(0.732457343586781,
0.755907568241666,0.788536317252911,0.875374334626722),.UNSPECIFIED.);
#5817=B_SPLINE_CURVE_WITH_KNOTS('',3,(#23154,#23155,#23156,#23157,#23158,
#23159,#23160,#23161),.UNSPECIFIED.,.F.,.F.,(4,2,2,4),(0.0547106625868535,
0.0760286813703655,0.152661638492553,0.177931278217517),.UNSPECIFIED.);
#5818=B_SPLINE_CURVE_WITH_KNOTS('',3,(#23165,#23166,#23167,#23168,#23169,
#23170,#23171,#23172),.UNSPECIFIED.,.F.,.F.,(4,2,2,4),(1.17732071475277,
1.23123357712069,1.29332668906214,1.30059629306183),.UNSPECIFIED.);
#5819=B_SPLINE_CURVE_WITH_KNOTS('',3,(#23175,#23176,#23177,#23178),
 .UNSPECIFIED.,.F.,.F.,(4,4),(2.48707902657156,2.52790949335551),
 .UNSPECIFIED.);
#5820=B_SPLINE_CURVE_WITH_KNOTS('',3,(#23180,#23181,#23182,#23183,#23184,
#23185),.UNSPECIFIED.,.F.,.F.,(4,2,4),(2.51549718449135,2.75342616579224,
3.00837168949227),.UNSPECIFIED.);
#5821=B_SPLINE_CURVE_WITH_KNOTS('',3,(#23189,#23190,#23191,#23192,#23193,
#23194),.UNSPECIFIED.,.F.,.F.,(4,2,4),(2.01718694432165,2.27213246802168,
2.51006144932256),.UNSPECIFIED.);
#5822=B_SPLINE_CURVE_WITH_KNOTS('',3,(#23199,#23200,#23201,#23202),
 .UNSPECIFIED.,.F.,.F.,(4,4),(2.52245632487896,2.56328703668614),
 .UNSPECIFIED.);
#5823=B_SPLINE_CURVE_WITH_KNOTS('',3,(#23206,#23207,#23208,#23209,#23210,
#23211,#23212,#23213),.UNSPECIFIED.,.F.,.F.,(4,2,2,4),(0.0547106625868542,
0.0760286813703704,0.152661638492567,0.177931278217529),.UNSPECIFIED.);
#5824=B_SPLINE_CURVE_WITH_KNOTS('',3,(#23217,#23218,#23219,#23220,#23221,
#23222,#23223,#23224),.UNSPECIFIED.,.F.,.F.,(4,2,2,4),(1.17732071475281,
1.23123357712072,1.29332668906218,1.30059629306187),.UNSPECIFIED.);
#5825=B_SPLINE_CURVE_WITH_KNOTS('',3,(#23230,#23231,#23232,#23233),
 .UNSPECIFIED.,.F.,.F.,(4,4),(0.0652178919951661,0.106048358779118),
 .UNSPECIFIED.);
#5826=B_SPLINE_CURVE_WITH_KNOTS('',3,(#23239,#23240,#23241,#23242,#23243,
#23244),.UNSPECIFIED.,.F.,.F.,(4,2,4),(0.0969458522659179,0.334874833566804,
0.589820357266834),.UNSPECIFIED.);
#5827=B_SPLINE_CURVE_WITH_KNOTS('',3,(#23247,#23248,#23249,#23250,#23251,
#23252),.UNSPECIFIED.,.F.,.F.,(4,2,4),(4.43573827654708,4.69068380024711,
4.92861278154799),.UNSPECIFIED.);
#5828=B_SPLINE_CURVE_WITH_KNOTS('',3,(#23253,#23254,#23255,#23256),
 .UNSPECIFIED.,.F.,.F.,(4,4),(4.94431745945535,4.98514817126253),
 .UNSPECIFIED.);
#5829=B_SPLINE_CURVE_WITH_KNOTS('',3,(#23268,#23269,#23270,#23271,#23272,
#23273,#23274,#23275,#23276,#23277,#23278,#23279,#23280,#23281,#23282),
 .UNSPECIFIED.,.F.,.F.,(4,3,2,2,2,2,4),(-0.398983050648409,0.,0.303890790649899,
0.455836185974848,0.607781581299797,0.752378251432681,0.891363616487534),
 .UNSPECIFIED.);
#5830=B_SPLINE_CURVE_WITH_KNOTS('',3,(#23285,#23286,#23287,#23288,#23289,
#23290,#23291,#23292,#23293,#23294,#23295,#23296,#23297,#23298),
 .UNSPECIFIED.,.F.,.F.,(4,2,2,2,2,2,4),(1.88180040661422,2.02078577166908,
2.16538244180196,2.31732783712691,2.46927323245186,2.77316402310176,3.17214707374984),
 .UNSPECIFIED.);
#5831=B_SPLINE_CURVE_WITH_KNOTS('',3,(#23300,#23301,#23302,#23303,#23304,
#23305,#23306,#23307,#23308,#23309,#23310,#23311,#23312,#23313),
 .UNSPECIFIED.,.F.,.F.,(4,2,2,2,2,2,4),(3.33378803122811,3.7327710818762,
4.0366618725261,4.18860726785105,4.34055266317599,4.48514933330888,4.62413469836373),
 .UNSPECIFIED.);
#5832=B_SPLINE_CURVE_WITH_KNOTS('',3,(#23316,#23317,#23318,#23319,#23320,
#23321,#23322,#23323,#23324,#23325,#23326,#23327,#23328,#23329,#23330),
 .UNSPECIFIED.,.F.,.F.,(4,2,2,2,2,3,4),(-0.891363616497897,-0.752378251432681,
-0.607781581299798,-0.455836185974849,-0.303890790649899,0.,0.398983050648084),
 .UNSPECIFIED.);
#5833=B_SPLINE_CURVE_WITH_KNOTS('',3,(#23383,#23384,#23385,#23386,#23387,
#23388,#23389,#23390,#23391,#23392),.UNSPECIFIED.,.F.,.F.,(4,2,2,2,4),(-0.262282482196273,
-0.227243259123267,-0.192394209601782,-0.119607601361313,-4.76311912134264E-9),
 .UNSPECIFIED.);
#5834=B_SPLINE_CURVE_WITH_KNOTS('',3,(#23396,#23397,#23398,#23399),
 .UNSPECIFIED.,.F.,.F.,(4,4),(0.126241397614949,0.16067610951008),
 .UNSPECIFIED.);
#5835=B_SPLINE_CURVE_WITH_KNOTS('',3,(#23401,#23402,#23403,#23404,#23405,
#23406,#23407,#23408,#23409,#23410),.UNSPECIFIED.,.F.,.F.,(4,2,2,2,4),(-0.170608922894474,
-0.144436965084543,-0.118924812328332,-0.0673862936043148,-0.0387732480152514),
 .UNSPECIFIED.);
#5836=B_SPLINE_CURVE_WITH_KNOTS('',3,(#23414,#23415,#23416,#23417,#23418,
#23419,#23420,#23421),.UNSPECIFIED.,.F.,.F.,(4,2,2,4),(0.833662394778907,
0.872087702776309,0.960661189189834,1.07674525757504),.UNSPECIFIED.);
#5837=B_SPLINE_CURVE_WITH_KNOTS('',3,(#23429,#23430,#23431,#23432),
 .UNSPECIFIED.,.F.,.F.,(4,4),(0.380499979702294,0.388208254648859),
 .UNSPECIFIED.);
#5838=B_SPLINE_CURVE_WITH_KNOTS('',3,(#23441,#23442,#23443,#23444,#23445,
#23446,#23447,#23448),.UNSPECIFIED.,.F.,.F.,(4,2,2,4),(2.91893463596102,
3.23522229935707,3.48529709981458,3.66035951911029),.UNSPECIFIED.);
#5839=B_SPLINE_CURVE_WITH_KNOTS('',3,(#23453,#23454,#23455,#23456,#23457,
#23458),.UNSPECIFIED.,.F.,.F.,(4,2,4),(2.69869497051652,2.83559328791136,
2.94278637796835),.UNSPECIFIED.);
#5840=B_SPLINE_CURVE_WITH_KNOTS('',3,(#23461,#23462,#23463,#23464),
 .UNSPECIFIED.,.F.,.F.,(4,4),(1.017709791401,1.13054679723933),
 .UNSPECIFIED.);
#5841=B_SPLINE_CURVE_WITH_KNOTS('',3,(#23466,#23467,#23468,#23469,#23470,
#23471),.UNSPECIFIED.,.F.,.F.,(4,2,4),(0.833062331394999,0.930697160636575,
1.25845097237232),.UNSPECIFIED.);
#5842=B_SPLINE_CURVE_WITH_KNOTS('',3,(#23475,#23476,#23477,#23478,#23479,
#23480),.UNSPECIFIED.,.F.,.F.,(4,2,4),(1.23426399221579,1.56201780395154,
1.65965263319311),.UNSPECIFIED.);
#5843=B_SPLINE_CURVE_WITH_KNOTS('',3,(#23482,#23483,#23484,#23485),
 .UNSPECIFIED.,.F.,.F.,(4,4),(3.27413741533483,3.47407808778078),
 .UNSPECIFIED.);
#5844=B_SPLINE_CURVE_WITH_KNOTS('',3,(#23489,#23490,#23491,#23492,#23493,
#23494),.UNSPECIFIED.,.F.,.F.,(4,2,4),(3.21456009570699,3.42341212522469,
3.75116593696043),.UNSPECIFIED.);
#5845=B_SPLINE_CURVE_WITH_KNOTS('',3,(#23497,#23498,#23499,#23500,#23501,
#23502),.UNSPECIFIED.,.F.,.F.,(4,2,4),(3.72697895680391,4.05473276853965,
4.26358479805735),.UNSPECIFIED.);
#5846=B_SPLINE_CURVE_WITH_KNOTS('',3,(#23509,#23510,#23511,#23512),
 .UNSPECIFIED.,.F.,.F.,(4,4),(0.,0.034672276467981),.UNSPECIFIED.);
#5847=B_SPLINE_CURVE_WITH_KNOTS('',3,(#23516,#23517,#23518,#23519,#23520,
#23521,#23522,#23523,#23524,#23525),.UNSPECIFIED.,.F.,.F.,(4,2,2,2,4),(-0.183241852105191,
-0.122572168940508,-0.0730310763026209,-0.0347695149370618,0.),
 .UNSPECIFIED.);
#5848=B_SPLINE_CURVE_WITH_KNOTS('',3,(#23528,#23529,#23530,#23531,#23532,
#23533,#23534,#23535),.UNSPECIFIED.,.F.,.F.,(4,2,2,4),(-0.113889377457268,
-0.0824728782510042,-0.0390501696847016,0.),.UNSPECIFIED.);
#5849=B_SPLINE_CURVE_WITH_KNOTS('',3,(#23538,#23539,#23540,#23541),
 .UNSPECIFIED.,.F.,.F.,(4,4),(2.52634703651881,2.53405531146538),
 .UNSPECIFIED.);
#5850=B_SPLINE_CURVE_WITH_KNOTS('',3,(#23549,#23550,#23551,#23552,#23553,
#23554,#23555,#23556),.UNSPECIFIED.,.F.,.F.,(4,2,2,4),(-1.07674525757504,
-0.960661189189834,-0.872087702776309,-0.833662394778906),.UNSPECIFIED.);
#5851=B_SPLINE_CURVE_WITH_KNOTS('',3,(#23564,#23565,#23566,#23567,#23568,
#23569,#23570,#23571,#23572,#23573),.UNSPECIFIED.,.F.,.F.,(4,2,2,2,4),(1.11476433242992,
1.1444058833459,1.18561459615229,1.2451591319351,1.2623152396797),
 .UNSPECIFIED.);
#5852=B_SPLINE_CURVE_WITH_KNOTS('',3,(#23574,#23575,#23576,#23577,#23578,
#23579),.UNSPECIFIED.,.F.,.F.,(4,2,4),(0.903765698424978,1.01257762815112,
1.10763430905713),.UNSPECIFIED.);
#5853=B_SPLINE_CURVE_WITH_KNOTS('',3,(#23620,#23621,#23622,#23623,#23624,
#23625),.UNSPECIFIED.,.F.,.F.,(4,2,4),(0.,0.299277276892222,0.598554553784445),
 .UNSPECIFIED.);
#5854=B_SPLINE_CURVE_WITH_KNOTS('',3,(#23689,#23690,#23691,#23692,#23693,
#23694),.UNSPECIFIED.,.F.,.F.,(4,2,4),(1.30156425141724,1.60084152830946,
1.90011880520168),.UNSPECIFIED.);
#5855=B_SPLINE_CURVE_WITH_KNOTS('',3,(#23822,#23823,#23824,#23825,#23826,
#23827,#23828,#23829,#23830,#23831,#23832,#23833,#23834,#23835,#23836,#23837,
#23838,#23839,#23840,#23841,#23842,#23843,#23844,#23845,#23846,#23847,#23848,
#23849,#23850,#23851,#23852,#23853,#23854,#23855,#23856,#23857,#23858,#23859,
#23860,#23861,#23862,#23863,#23864,#23865,#23866,#23867,#23868,#23869,#23870,
#23871,#23872,#23873,#23874,#23875,#23876,#23877,#23878,#23879,#23880,#23881,
#23882,#23883,#23884,#23885,#23886,#23887,#23888,#23889,#23890,#23891,#23892,
#23893,#23894,#23895,#23896,#23897,#23898,#23899,#23900,#23901,#23902,#23903,
#23904,#23905,#23906,#23907,#23908,#23909,#23910,#23911,#23912,#23913,#23914,
#23915,#23916,#23917,#23918,#23919,#23920,#23921,#23922,#23923,#23924,#23925,
#23926,#23927,#23928,#23929,#23930,#23931,#23932,#23933,#23934,#23935,#23936,
#23937,#23938,#23939,#23940,#23941,#23942,#23943,#23944,#23945,#23946,#23947,
#23948,#23949,#23950,#23951,#23952,#23953,#23954,#23955,#23956,#23957,#23958,
#23959,#23960,#23961,#23962,#23963,#23964,#23965,#23966),.UNSPECIFIED.,
 .F.,.F.,(4,3,3,3,3,3,3,3,3,3,3,3,3,3,3,3,3,3,3,3,3,3,3,3,3,3,3,3,3,3,3,
3,3,3,3,3,3,3,3,3,3,3,3,3,3,3,3,3,4),(-9.03360503529916,-8.86127604911423,
-8.68030493926038,-8.58511998488549,-8.48447670513606,-8.33562131806494,
-8.19092008514545,-8.0572821722663,-7.97401584150341,-7.8693192178446,-7.85250838613552,
-7.7529816299934,-7.65895403017618,-7.57088295203555,-7.56492643035897,
-7.43104909192891,-7.27359031327789,-7.22029805007692,-7.19153158116352,
-7.1005636564517,-7.05507969409579,-7.03145147969554,-7.01779966872338,
-7.00959573173988,-6.9345284310504,-6.9042290999944,-6.82350845623894,-6.798847127526,
-6.79827768985696,-6.73152769721655,-6.66072565278933,-6.6295195877408,
-6.58805343095027,-6.51251273433006,-6.43306219328815,-6.34686858849436,
-6.30164584299914,-6.27213715467711,-6.08350153753309,-5.95594925749777,
-5.86905659224252,-5.70894094483269,-5.53318477689864,-5.33956788736791,
-5.32383027162032,-5.15411754086443,-5.01473160504778,-4.88034698710192,
-4.77483276840798),.UNSPECIFIED.);
#5856=B_SPLINE_CURVE_WITH_KNOTS('',3,(#23968,#23969,#23970,#23971),
 .UNSPECIFIED.,.F.,.F.,(4,4),(-4.77483276840798,-4.77362713684779),
 .UNSPECIFIED.);
#5857=B_SPLINE_CURVE_WITH_KNOTS('',3,(#23973,#23974,#23975,#23976,#23977,
#23978,#23979,#23980,#23981,#23982),.UNSPECIFIED.,.F.,.F.,(4,2,2,2,4),(-0.242938279070336,
-0.168006152846838,-0.0865010676432649,0.,0.000616246384910699),
 .UNSPECIFIED.);
#5858=B_SPLINE_CURVE_WITH_KNOTS('',3,(#23984,#23985,#23986,#23987,#23988,
#23989,#23990,#23991,#23992),.UNSPECIFIED.,.F.,.F.,(4,1,1,1,1,1,4),(4.69190485072485,
5.32399487973813,5.95608490875141,6.27212992325805,6.58817493776469,6.79887161410245,
6.9042290999944),.UNSPECIFIED.);
#5859=B_SPLINE_CURVE_WITH_KNOTS('',3,(#23994,#23995,#23996,#23997,#23998,
#23999,#24000,#24001,#24002),.UNSPECIFIED.,.F.,.F.,(4,1,1,1,1,1,4),(6.90422173516042,
7.00956829044021,7.22026496677797,7.43096164311573,7.85235499579125,8.48444502480452,
9.1165350538178),.UNSPECIFIED.);
#5860=B_SPLINE_CURVE_WITH_KNOTS('',3,(#24004,#24005,#24006,#24007,#24008,
#24009,#24010,#24011,#24012,#24013,#24014,#24015,#24016,#24017,#24018,#24019,
#24020,#24021,#24022,#24023,#24024,#24025,#24026,#24027,#24028,#24029,#24030,
#24031,#24032,#24033,#24034,#24035,#24036,#24037,#24038,#24039,#24040,#24041,
#24042,#24043,#24044,#24045,#24046),.UNSPECIFIED.,.F.,.F.,(4,3,3,3,3,3,
3,3,3,3,3,3,3,3,4),(-0.242801352910212,-0.242186632434824,-0.219544055688108,
-0.196801089607309,-0.174161287740677,-0.167361569498752,-0.144942724018392,
-0.122816117509345,-0.104446209841387,-0.0913857413699424,-0.0692335334813781,
-0.0520648532547955,-0.0303649913441254,-0.0155217575353379,0.),
 .UNSPECIFIED.);
#5861=B_SPLINE_CURVE_WITH_KNOTS('',3,(#24047,#24048,#24049,#24050),
 .UNSPECIFIED.,.F.,.F.,(4,4),(-9.03481070423354,-9.03360503529916),
 .UNSPECIFIED.);
#5862=B_SPLINE_CURVE_WITH_KNOTS('',3,(#24055,#24056,#24057,#24058),
 .UNSPECIFIED.,.F.,.F.,(4,4),(-1.22314360071756,-1.20515902132338),
 .UNSPECIFIED.);
#5863=B_SPLINE_CURVE_WITH_KNOTS('',3,(#24062,#24063,#24064,#24065),
 .UNSPECIFIED.,.F.,.F.,(4,4),(-0.29725330048063,-0.279268721057567),
 .UNSPECIFIED.);
#5864=B_SPLINE_CURVE_WITH_KNOTS('',3,(#24066,#24067,#24068,#24069,#24070,
#24071,#24072,#24073,#24074,#24075,#24076,#24077,#24078,#24079,#24080,#24081,
#24082,#24083,#24084,#24085,#24086,#24087,#24088,#24089,#24090,#24091,#24092,
#24093,#24094,#24095,#24096,#24097,#24098,#24099,#24100,#24101,#24102,#24103,
#24104,#24105,#24106,#24107,#24108),.UNSPECIFIED.,.F.,.F.,(4,3,3,3,3,3,
3,3,3,3,3,3,3,3,4),(-0.242801352899586,-0.242186632423413,-0.219537690406595,
-0.196781321893934,-0.174161287742756,-0.167361569500369,-0.144934602663136,
-0.12280231801636,-0.104446209842394,-0.0913857413708117,-0.0692313418368474,
-0.0520648532552464,-0.0303594951871729,-0.0155217575353938,0.),
 .UNSPECIFIED.);
#5865=B_SPLINE_CURVE_WITH_KNOTS('',3,(#24113,#24114,#24115,#24116),
 .UNSPECIFIED.,.F.,.F.,(4,4),(-0.29725330048063,-0.279268721057567),
 .UNSPECIFIED.);
#5866=B_SPLINE_CURVE_WITH_KNOTS('',3,(#24120,#24121,#24122,#24123,#24124,
#24125,#24126,#24127,#24128,#24129),.UNSPECIFIED.,.F.,.F.,(4,2,2,2,4),(-0.000616246385038109,
0.,0.0865010676321112,0.168006152835906,0.242938281746869),
 .UNSPECIFIED.);
#5867=B_SPLINE_CURVE_WITH_KNOTS('',3,(#24130,#24131,#24132,#24133),
 .UNSPECIFIED.,.F.,.F.,(4,4),(-1.22314360071756,-1.20515902132338),
 .UNSPECIFIED.);
#5868=B_SPLINE_CURVE_WITH_KNOTS('',3,(#24241,#24242,#24243,#24244,#24245,
#24246,#24247,#24248,#24249,#24250,#24251,#24252,#24253,#24254,#24255,#24256,
#24257,#24258,#24259,#24260,#24261,#24262,#24263,#24264,#24265,#24266,#24267,
#24268,#24269,#24270,#24271,#24272,#24273,#24274,#24275,#24276,#24277,#24278,
#24279,#24280,#24281,#24282,#24283,#24284,#24285,#24286,#24287,#24288,#24289,
#24290,#24291,#24292,#24293,#24294,#24295,#24296,#24297,#24298,#24299,#24300,
#24301,#24302,#24303,#24304,#24305,#24306,#24307,#24308,#24309,#24310,#24311,
#24312,#24313,#24314,#24315,#24316,#24317,#24318,#24319,#24320,#24321,#24322,
#24323,#24324,#24325,#24326,#24327,#24328,#24329,#24330,#24331,#24332,#24333,
#24334,#24335,#24336,#24337,#24338,#24339,#24340,#24341,#24342,#24343,#24344,
#24345,#24346,#24347,#24348,#24349,#24350,#24351,#24352,#24353,#24354,#24355,
#24356,#24357,#24358,#24359,#24360,#24361,#24362,#24363,#24364,#24365,#24366,
#24367,#24368,#24369,#24370,#24371,#24372,#24373,#24374,#24375,#24376,#24377,
#24378,#24379),.UNSPECIFIED.,.F.,.F.,(4,3,3,3,3,3,3,3,3,3,3,3,3,3,3,3,3,
3,3,3,3,3,3,3,3,3,3,3,3,3,3,3,3,3,3,3,3,3,3,3,3,3,3,3,3,3,4),(-9.03360503529916,
-8.88762712989133,-8.73438537212543,-8.58511998488547,-8.48471177745109,
-8.31820898189202,-8.16176952472331,-8.02347743465504,-7.97401584150339,
-7.85242356738565,-7.7130263178265,-7.64168550640925,-7.56492643035895,
-7.44264973091217,-7.43099479970612,-7.32266350526435,-7.22031662758344,
-7.20899476726769,-7.12730880556465,-7.05066524148345,-7.02706994696297,
-7.00959174062256,-6.92909838503205,-6.9042290999944,-6.8364308822668,-6.79885763435364,
-6.79827768985695,-6.73134713296141,-6.66020538781699,-6.62951958774078,
-6.58806194215221,-6.51258041717339,-6.43313965917345,-6.34691295539751,
-6.30164584299912,-6.27214200893841,-6.08189682874827,-5.95595235925663,
-5.8690565922425,-5.70909971098082,-5.53356025052748,-5.34017121243578,
-5.3238295138681,-5.1541175408644,-5.01464175348577,-4.88022674714609,-4.77483276840798),
 .UNSPECIFIED.);
#5869=B_SPLINE_CURVE_WITH_KNOTS('',3,(#24380,#24381,#24382,#24383),
 .UNSPECIFIED.,.F.,.F.,(4,4),(4.77362713684778,4.77483276840798),
 .UNSPECIFIED.);
#5870=B_SPLINE_CURVE_WITH_KNOTS('',3,(#24385,#24386,#24387,#24388,#24389,
#24390,#24391,#24392,#24393),.UNSPECIFIED.,.F.,.F.,(4,1,1,1,1,1,4),(4.69190485072485,
5.32399487973813,5.95608490875141,6.27212992325805,6.58817493776469,6.79887161410245,
6.9042290999944),.UNSPECIFIED.);
#5871=B_SPLINE_CURVE_WITH_KNOTS('',3,(#24394,#24395,#24396,#24397,#24398,
#24399,#24400,#24401,#24402,#24403),.UNSPECIFIED.,.F.,.F.,(4,1,1,1,1,1,
1,4),(6.90422178665282,7.00956829044021,7.22026496677796,7.43096164311572,
7.64165831945348,7.85235499579124,8.48444502480452,9.1165350538178),
 .UNSPECIFIED.);
#5872=B_SPLINE_CURVE_WITH_KNOTS('',3,(#24404,#24405,#24406,#24407),
 .UNSPECIFIED.,.F.,.F.,(4,4),(-9.03481070423354,-9.03360503529916),
 .UNSPECIFIED.);
#5873=B_SPLINE_CURVE_WITH_KNOTS('',3,(#24428,#24429,#24430,#24431,#24432,
#24433,#24434,#24435,#24436,#24437),.UNSPECIFIED.,.F.,.F.,(4,2,2,2,4),(-0.150488872007352,
-0.145598643293466,-0.0727993216467576,0.,0.00489022871386419),
 .UNSPECIFIED.);
#5874=B_SPLINE_CURVE_WITH_KNOTS('',3,(#24453,#24454,#24455,#24456,#24457,
#24458),.UNSPECIFIED.,.F.,.F.,(4,2,4),(1.30156425141723,1.60084152830946,
1.90011880520168),.UNSPECIFIED.);
#5875=B_SPLINE_CURVE_WITH_KNOTS('',3,(#24521,#24522,#24523,#24524,#24525,
#24526),.UNSPECIFIED.,.F.,.F.,(4,2,4),(0.,0.299277276892223,0.598554553784447),
 .UNSPECIFIED.);
#5876=B_SPLINE_CURVE_WITH_KNOTS('',3,(#24534,#24535,#24536,#24537,#24538,
#24539,#24540,#24541,#24542,#24543),.UNSPECIFIED.,.F.,.F.,(4,2,2,2,4),(-0.150488872007919,
-0.145598643294013,-0.0727993216470067,0.,0.00489022871390594),
 .UNSPECIFIED.);
#5877=B_SPLINE_CURVE_WITH_KNOTS('',3,(#24677,#24678,#24679,#24680,#24681,
#24682,#24683,#24684,#24685,#24686),.UNSPECIFIED.,.F.,.F.,(4,2,2,2,4),(0.,
0.449224301228608,0.898448602457216,1.38616749821439,1.87388639397155),
 .UNSPECIFIED.);
#5878=B_SPLINE_CURVE_WITH_KNOTS('',3,(#24687,#24688,#24689,#24690,#24691,
#24692,#24693,#24694,#24695,#24696,#24697,#24698,#24699,#24700,#24701,#24702,
#24703,#24704,#24705,#24706,#24707,#24708,#24709,#24710,#24711,#24712,#24713,
#24714,#24715,#24716),.UNSPECIFIED.,.F.,.F.,(4,2,2,2,2,2,2,2,2,2,2,2,2,
2,4),(1.87388639397155,2.39804133800567,2.92219628203978,3.37669912288026,
3.6039505433005,3.83120196372073,4.05845338414097,4.28570480456121,4.74020764540168,
5.2643625894358,5.78851753346991,6.27623642922708,6.76395532498425,7.21317962621286,
7.66240392744147),.UNSPECIFIED.);
#5879=B_SPLINE_CURVE_WITH_KNOTS('',3,(#24813,#24814,#24815,#24816,#24817,
#24818),.UNSPECIFIED.,.F.,.F.,(4,2,4),(3.40145412174457,3.72577473971897,
4.05009535769338),.UNSPECIFIED.);
#5880=B_SPLINE_CURVE_WITH_KNOTS('',3,(#24847,#24848,#24849,#24850,#24851,
#24852,#24853,#24854,#24855,#24856,#24857,#24858,#24859,#24860,#24861,#24862,
#24863,#24864,#24865,#24866,#24867,#24868,#24869,#24870,#24871,#24872,#24873,
#24874,#24875,#24876,#24877,#24878,#24879,#24880,#24881,#24882,#24883,#24884,
#24885,#24886,#24887,#24888,#24889,#24890,#24891,#24892),.UNSPECIFIED.,
 .F.,.F.,(4,2,2,2,2,2,2,2,2,2,2,2,2,2,2,2,2,2,2,2,2,2,4),(0.330726835810475,
0.524808847269917,1.04961769453983,1.32954893198247,1.6094801694251,1.88941140686773,
2.16934264431036,2.77369676559426,3.37805088687816,3.90945930374807,4.17516351218302,
4.44086772061798,4.70657192905293,4.97227613748788,5.50368455435779,6.10803867564169,
6.71239279692559,6.99232403436822,7.27225527181085,7.55218650925349,7.83211774669612,
8.35692659396604,8.55100860542548),.UNSPECIFIED.);
#5881=B_SPLINE_CURVE_WITH_KNOTS('',3,(#25127,#25128,#25129,#25130,#25131,
#25132,#25133,#25134,#25135,#25136,#25137,#25138,#25139,#25140,#25141,#25142),
 .UNSPECIFIED.,.F.,.F.,(4,3,3,3,3,4),(-4.09323272002468,-3.98467880200839,
-3.48659395175734,-2.9885091015063,-2.49042425125525,-2.06652207565085),
 .UNSPECIFIED.);
#5882=B_SPLINE_CURVE_WITH_KNOTS('',3,(#25145,#25146,#25147,#25148,#25149,
#25150,#25151,#25152,#25153,#25154),.UNSPECIFIED.,.F.,.F.,(4,3,3,4),(0.,
0.498084850251037,0.996169700502089,1.11488200921589),.UNSPECIFIED.);
#5883=B_SPLINE_CURVE_WITH_KNOTS('',3,(#25159,#25160,#25161,#25162,#25163,
#25164,#25165,#25166,#25167,#25168,#25169,#25170,#25171,#25172,#25173,#25174,
#25175,#25176,#25177,#25178,#25179,#25180,#25181,#25182,#25183,#25184,#25185,
#25186,#25187,#25188,#25189,#25190,#25191,#25192,#25193,#25194,#25195,#25196,
#25197,#25198),.UNSPECIFIED.,.F.,.F.,(4,3,3,3,3,3,3,3,3,3,3,3,3,4),(-10.3764180272042,
-9.96169700502099,-9.46361215476994,-8.96552730451889,-8.46744245426784,
-7.96935760401679,-7.47127275376574,-6.97318790351469,-6.47510305326364,
-5.9770182030126,-5.47893335276154,-4.9808485025105,-4.48276365225944,-4.09323272002468),
 .UNSPECIFIED.);
#5884=B_SPLINE_CURVE_WITH_KNOTS('',3,(#25199,#25200,#25201,#25202,#25203,
#25204,#25205,#25206,#25207,#25208,#25209,#25210,#25211,#25212,#25213,#25214,
#25215,#25216,#25217,#25218,#25219,#25220,#25221,#25222,#25223,#25224,#25225,
#25226,#25227,#25228,#25229,#25230,#25231,#25232,#25233,#25234,#25235,#25236,
#25237,#25238),.UNSPECIFIED.,.F.,.F.,(4,3,3,3,3,3,3,3,3,3,3,3,3,4),(1.11488200921589,
1.49425455075314,1.99233940100419,2.49042425125524,2.98850910150629,3.48659395175734,
3.98467880200839,4.48276365225944,4.98084850251049,5.47893335276154,5.97701820301259,
6.47510305326364,6.97318790351469,7.39806731639545),.UNSPECIFIED.);
#5885=B_SPLINE_CURVE_WITH_KNOTS('',3,(#25243,#25244,#25245,#25246,#25247,
#25248,#25249,#25250,#25251,#25252,#25253,#25254,#25255,#25256,#25257,#25258,
#25259,#25260,#25261,#25262,#25263,#25264,#25265,#25266,#25267,#25268,#25269,
#25270,#25271,#25272,#25273,#25274,#25275,#25276,#25277,#25278,#25279,#25280,
#25281,#25282,#25283,#25284,#25285),.UNSPECIFIED.,.F.,.F.,(4,3,3,3,3,3,
3,3,3,3,3,3,3,3,4),(-16.6596033343838,-16.4368000582846,-15.9387152080336,
-15.4406303577825,-14.9425455075315,-14.4444606572804,-13.9463758070294,
-13.4482909567783,-12.9502061065273,-12.4521212562762,-11.9540364060252,
-11.4559515557741,-10.9578667055231,-10.459781855272,-10.3764180272042),
 .UNSPECIFIED.);
#5886=B_SPLINE_CURVE_WITH_KNOTS('',3,(#25286,#25287,#25288,#25289,#25290,
#25291,#25292,#25293,#25294,#25295,#25296,#25297,#25298,#25299,#25300,#25301,
#25302,#25303,#25304,#25305,#25306,#25307,#25308,#25309,#25310,#25311,#25312,
#25313,#25314,#25315,#25316,#25317,#25318,#25319,#25320,#25321,#25322,#25323,
#25324,#25325,#25326,#25327,#25328),.UNSPECIFIED.,.F.,.F.,(4,3,3,3,3,3,
3,3,3,3,3,3,3,3,4),(7.39806731639545,7.47127275376574,7.96935760401679,
8.46744245426784,8.96552730451889,9.46361215476994,9.96169700502099,10.459781855272,
10.9578667055231,11.4559515557741,11.9540364060252,12.4521212562762,12.9502061065273,
13.4482909567783,13.681252623575),.UNSPECIFIED.);
#5887=B_SPLINE_CURVE_WITH_KNOTS('',3,(#25333,#25334,#25335,#25336,#25337,
#25338,#25339,#25340,#25341,#25342,#25343,#25344,#25345,#25346,#25347,#25348,
#25349,#25350,#25351,#25352,#25353,#25354,#25355,#25356,#25357,#25358,#25359,
#25360,#25361,#25362,#25363,#25364,#25365,#25366,#25367,#25368,#25369,#25370,
#25371,#25372,#25373,#25374,#25375),.UNSPECIFIED.,.F.,.F.,(4,3,3,3,3,3,
3,3,3,3,3,3,3,3,4),(-22.9427886415634,-22.9119031115483,-22.4138182612972,
-21.9157334110462,-21.4176485607951,-20.9195637105441,-20.421478860293,
-19.923394010042,-19.4253091597909,-18.9272243095399,-18.4291394592888,
-17.9310546090378,-17.4329697587867,-16.9348849085357,-16.6596033343838),
 .UNSPECIFIED.);
#5888=B_SPLINE_CURVE_WITH_KNOTS('',3,(#25376,#25377,#25378,#25379,#25380,
#25381,#25382,#25383,#25384,#25385,#25386,#25387,#25388,#25389,#25390,#25391,
#25392,#25393,#25394,#25395,#25396,#25397,#25398,#25399,#25400,#25401,#25402,
#25403,#25404,#25405,#25406,#25407,#25408,#25409,#25410,#25411,#25412,#25413,
#25414,#25415,#25416,#25417,#25418),.UNSPECIFIED.,.F.,.F.,(4,3,3,3,3,3,
3,3,3,3,3,3,3,3,4),(13.681252623575,13.9463758070294,14.4444606572804,14.9425455075315,
15.4406303577825,15.9387152080336,16.4368000582846,16.9348849085357,17.4329697587867,
17.9310546090378,18.4291394592888,18.9272243095399,19.4253091597909,19.923394010042,
19.9644379307546),.UNSPECIFIED.);
#5889=B_SPLINE_CURVE_WITH_KNOTS('',3,(#25423,#25424,#25425,#25426,#25427,
#25428,#25429,#25430,#25431,#25432,#25433,#25434,#25435,#25436,#25437,#25438,
#25439,#25440,#25441,#25442,#25443,#25444,#25445,#25446,#25447,#25448,#25449,
#25450,#25451,#25452,#25453,#25454,#25455,#25456,#25457,#25458,#25459,#25460,
#25461,#25462),.UNSPECIFIED.,.F.,.F.,(4,3,3,3,3,3,3,3,3,3,3,3,3,4),(-29.225973948743,
-28.8889213145609,-28.3908364643098,-27.8927516140588,-27.3946667638077,
-26.8965819135567,-26.3984970633056,-25.9004122130546,-25.4023273628035,
-24.9042425125525,-24.4061576623014,-23.9080728120504,-23.4099879617993,
-22.9427886415634),.UNSPECIFIED.);
#5890=B_SPLINE_CURVE_WITH_KNOTS('',3,(#25463,#25464,#25465,#25466,#25467,
#25468,#25469,#25470,#25471,#25472,#25473,#25474,#25475,#25476,#25477,#25478,
#25479,#25480,#25481,#25482,#25483,#25484,#25485,#25486,#25487,#25488,#25489,
#25490,#25491,#25492,#25493,#25494,#25495,#25496,#25497,#25498,#25499,#25500,
#25501,#25502),.UNSPECIFIED.,.F.,.F.,(4,3,3,3,3,3,3,3,3,3,3,3,3,4),(19.9644379307546,
20.421478860293,20.9195637105441,21.4176485607951,21.9157334110462,22.4138182612972,
22.9119031115483,23.4099879617993,23.9080728120504,24.4061576623014,24.9042425125525,
25.4023273628035,25.9004122130546,26.2476232379342),.UNSPECIFIED.);
#5891=B_SPLINE_CURVE_WITH_KNOTS('',3,(#25507,#25508,#25509,#25510,#25511,
#25512,#25513,#25514,#25515,#25516,#25517,#25518,#25519,#25520,#25521,#25522,
#25523,#25524,#25525,#25526,#25527,#25528,#25529,#25530,#25531,#25532,#25533,
#25534,#25535,#25536,#25537,#25538,#25539,#25540,#25541,#25542,#25543,#25544,
#25545,#25546,#25547,#25548,#25549),.UNSPECIFIED.,.F.,.F.,(4,3,3,3,3,3,
3,3,3,3,3,3,3,3,4),(-35.5091592559226,-35.3640243678245,-34.8659395175735,
-34.3678546673224,-33.8697698170714,-33.3716849668203,-32.8736001165693,
-32.3755152663182,-31.8774304160672,-31.3793455658161,-30.8812607155651,
-30.383175865314,-29.885091015063,-29.3870061648119,-29.225973948743),
 .UNSPECIFIED.);
#5892=B_SPLINE_CURVE_WITH_KNOTS('',3,(#25550,#25551,#25552,#25553,#25554,
#25555,#25556,#25557,#25558,#25559,#25560,#25561,#25562,#25563,#25564,#25565,
#25566,#25567,#25568,#25569,#25570,#25571,#25572,#25573,#25574,#25575,#25576,
#25577,#25578,#25579,#25580,#25581,#25582,#25583,#25584,#25585,#25586,#25587,
#25588,#25589,#25590,#25591,#25592),.UNSPECIFIED.,.F.,.F.,(4,3,3,3,3,3,
3,3,3,3,3,3,3,3,4),(26.2476232379342,26.3984970633056,26.8965819135567,
27.3946667638077,27.8927516140588,28.3908364643098,28.8889213145609,29.3870061648119,
29.885091015063,30.383175865314,30.8812607155651,31.3793455658161,31.8774304160672,
32.3755152663182,32.5308085451138),.UNSPECIFIED.);
#5893=B_SPLINE_CURVE_WITH_KNOTS('',3,(#25597,#25598,#25599,#25600,#25601,
#25602,#25603,#25604,#25605,#25606,#25607,#25608,#25609,#25610,#25611,#25612,
#25613,#25614,#25615,#25616,#25617,#25618,#25619,#25620,#25621,#25622,#25623,
#25624,#25625,#25626,#25627,#25628,#25629,#25630,#25631,#25632,#25633,#25634,
#25635,#25636),.UNSPECIFIED.,.F.,.F.,(4,3,3,3,3,3,3,3,3,3,3,3,3,4),(-41.7923445631022,
-41.3410425708371,-40.842957720586,-40.344872870335,-39.846788020084,-39.3487031698329,
-38.8506183195819,-38.3525334693308,-37.8544486190798,-37.3563637688287,
-36.8582789185777,-36.3601940683266,-35.8621092180756,-35.5091592559226),
 .UNSPECIFIED.);
#5894=B_SPLINE_CURVE_WITH_KNOTS('',3,(#25637,#25638,#25639,#25640,#25641,
#25642,#25643,#25644,#25645,#25646,#25647,#25648,#25649,#25650,#25651,#25652,
#25653,#25654,#25655,#25656,#25657,#25658,#25659,#25660,#25661,#25662,#25663,
#25664,#25665,#25666,#25667,#25668,#25669,#25670,#25671,#25672,#25673,#25674,
#25675,#25676),.UNSPECIFIED.,.F.,.F.,(4,3,3,3,3,3,3,3,3,3,3,3,3,4),(32.5308085451138,
32.8736001165693,33.3716849668203,33.8697698170714,34.3678546673224,34.8659395175735,
35.3640243678245,35.8621092180756,36.3601940683266,36.8582789185776,37.3563637688287,
37.8544486190798,38.3525334693308,38.8139938522934),.UNSPECIFIED.);
#5895=B_SPLINE_CURVE_WITH_KNOTS('',3,(#25681,#25682,#25683,#25684,#25685,
#25686,#25687,#25688,#25689,#25690,#25691,#25692,#25693,#25694,#25695,#25696,
#25697,#25698,#25699,#25700,#25701,#25702,#25703,#25704,#25705,#25706,#25707,
#25708,#25709,#25710,#25711,#25712,#25713,#25714,#25715,#25716,#25717,#25718,
#25719,#25720),.UNSPECIFIED.,.F.,.F.,(4,3,3,3,3,3,3,3,3,3,3,3,3,4),(-48.0755298702818,
-47.8161456241007,-46.8199759235986,-46.3218910733476,-45.8238062230966,
-45.3257213728455,-44.8276365225944,-44.3295516723434,-43.8314668220923,
-43.3333819718413,-42.8352971215903,-42.3372122713392,-41.8391274210882,
-41.7923445631022),.UNSPECIFIED.);
#5896=B_SPLINE_CURVE_WITH_KNOTS('',3,(#25721,#25722,#25723,#25724,#25725,
#25726,#25727,#25728,#25729,#25730,#25731,#25732,#25733,#25734,#25735,#25736,
#25737,#25738,#25739,#25740,#25741,#25742,#25743,#25744,#25745,#25746,#25747,
#25748,#25749,#25750,#25751,#25752,#25753,#25754,#25755,#25756,#25757,#25758,
#25759,#25760,#25761,#25762,#25763),.UNSPECIFIED.,.F.,.F.,(4,3,3,3,3,3,
3,3,3,3,3,3,3,3,4),(38.8139938522934,38.8506183195818,39.3487031698329,
39.846788020084,40.344872870335,40.842957720586,41.3410425708371,41.8391274210882,
42.3372122713392,42.8352971215903,43.3333819718413,43.8314668220924,44.3295516723434,
44.8276365225945,45.097179159473),.UNSPECIFIED.);
#5897=B_SPLINE_CURVE_WITH_KNOTS('',3,(#25768,#25769,#25770,#25771,#25772,
#25773,#25774,#25775,#25776,#25777,#25778,#25779,#25780,#25781,#25782,#25783,
#25784,#25785,#25786,#25787,#25788,#25789,#25790,#25791,#25792,#25793,#25794,
#25795,#25796,#25797,#25798,#25799,#25800,#25801,#25802,#25803,#25804),
 .UNSPECIFIED.,.F.,.F.,(4,3,3,3,3,3,3,3,3,3,3,3,4),(-54.3587151774614,-54.2912486773644,
-53.7931638271134,-53.2950789768623,-52.7969941266112,-52.2989092763602,
-51.8008244261091,-51.3027395758581,-50.8046547256071,-50.306569875356,
-49.8084850251049,-48.8123153246028,-48.0755298702818),.UNSPECIFIED.);
#5898=B_SPLINE_CURVE_WITH_KNOTS('',3,(#25805,#25806,#25807,#25808,#25809,
#25810,#25811,#25812,#25813,#25814,#25815,#25816,#25817,#25818,#25819,#25820,
#25821,#25822,#25823,#25824,#25825,#25826,#25827,#25828,#25829,#25830,#25831,
#25832,#25833,#25834,#25835,#25836,#25837,#25838),.UNSPECIFIED.,.F.,.F.,
(4,3,3,3,3,3,3,3,3,3,3,4),(45.097179159473,45.3257213728455,45.8238062230965,
46.3218910733476,46.8199759235986,47.8161456241007,48.8123153246028,49.8084850251049,
50.306569875356,50.8046547256071,51.3027395758581,51.3803644666526),
 .UNSPECIFIED.);
#5899=B_SPLINE_CURVE_WITH_KNOTS('',3,(#25843,#25844,#25845,#25846,#25847,
#25848,#25849,#25850,#25851,#25852,#25853,#25854,#25855,#25856,#25857,#25858,
#25859,#25860,#25861,#25862,#25863,#25864,#25865,#25866,#25867,#25868,#25869,
#25870,#25871,#25872,#25873,#25874,#25875,#25876,#25877,#25878,#25879,#25880,
#25881,#25882),.UNSPECIFIED.,.F.,.F.,(4,3,3,3,3,3,3,3,3,3,3,3,3,4),(-60.641900484641,
-60.268266880377,-59.7701820301259,-59.2720971798749,-58.7740123296238,
-58.2759274793728,-57.7778426291217,-57.2797577788707,-56.7816729286196,
-56.2835880783686,-55.7855032281175,-55.2874183778665,-54.7893335276154,
-54.3587151774614),.UNSPECIFIED.);
#5900=B_SPLINE_CURVE_WITH_KNOTS('',3,(#25883,#25884,#25885,#25886,#25887,
#25888,#25889,#25890,#25891,#25892,#25893,#25894,#25895,#25896,#25897,#25898,
#25899,#25900,#25901,#25902,#25903,#25904,#25905,#25906,#25907,#25908,#25909,
#25910,#25911,#25912,#25913,#25914,#25915,#25916,#25917,#25918,#25919,#25920,
#25921,#25922),.UNSPECIFIED.,.F.,.F.,(4,3,3,3,3,3,3,3,3,3,3,3,3,4),(51.3803644666526,
51.8008244261091,52.2989092763602,52.7969941266112,53.2950789768623,53.7931638271133,
54.2912486773644,54.7893335276154,55.2874183778665,55.7855032281175,56.2835880783686,
56.7816729286196,57.2797577788707,57.6635497738322),.UNSPECIFIED.);
#5901=B_SPLINE_CURVE_WITH_KNOTS('',3,(#25927,#25928,#25929,#25930,#25931,
#25932,#25933,#25934,#25935,#25936,#25937,#25938,#25939,#25940,#25941,#25942,
#25943,#25944,#25945,#25946,#25947,#25948,#25949,#25950,#25951,#25952,#25953,
#25954,#25955,#25956,#25957,#25958,#25959,#25960,#25961,#25962,#25963,#25964,
#25965,#25966,#25967,#25968,#25969),.UNSPECIFIED.,.F.,.F.,(4,3,3,3,3,3,
3,3,3,3,3,3,3,3,4),(-66.9250857918206,-66.7433699336406,-66.2452850833896,
-65.7472002331385,-65.2491153828875,-64.7510305326364,-64.2529456823854,
-63.7548608321343,-63.2567759818833,-62.7586911316322,-62.2606062813812,
-61.7625214311301,-61.2644365808791,-60.766351730628,-60.641900484641),
 .UNSPECIFIED.);
#5902=B_SPLINE_CURVE_WITH_KNOTS('',3,(#25970,#25971,#25972,#25973,#25974,
#25975,#25976,#25977,#25978,#25979,#25980,#25981,#25982,#25983,#25984,#25985,
#25986,#25987,#25988,#25989,#25990,#25991,#25992,#25993,#25994,#25995,#25996,
#25997,#25998,#25999,#26000,#26001,#26002,#26003,#26004,#26005,#26006,#26007,
#26008,#26009,#26010,#26011,#26012),.UNSPECIFIED.,.F.,.F.,(4,3,3,3,3,3,
3,3,3,3,3,3,3,3,4),(57.6635497738322,57.7778426291217,58.2759274793728,
58.7740123296238,59.2720971798749,59.7701820301259,60.268266880377,60.766351730628,
61.2644365808791,61.7625214311301,62.2606062813812,62.7586911316322,63.2567759818833,
63.7548608321343,63.9467350810118),.UNSPECIFIED.);
#5903=B_SPLINE_CURVE_WITH_KNOTS('',3,(#26017,#26018,#26019,#26020,#26021,
#26022,#26023,#26024,#26025,#26026,#26027,#26028,#26029,#26030,#26031,#26032,
#26033,#26034,#26035,#26036,#26037,#26038,#26039,#26040,#26041,#26042,#26043,
#26044,#26045,#26046,#26047,#26048,#26049,#26050,#26051,#26052,#26053,#26054,
#26055,#26056),.UNSPECIFIED.,.F.,.F.,(4,3,3,3,3,3,3,3,3,3,3,3,3,4),(-73.2082710990001,
-72.7203881366532,-72.2223032864022,-71.7242184361511,-71.2261335859001,
-70.728048735649,-70.229963885398,-69.7318790351469,-69.2337941848959,-68.7357093346448,
-68.2376244843938,-67.7395396341427,-67.2414547838917,-66.9250857918206),
 .UNSPECIFIED.);
#5904=B_SPLINE_CURVE_WITH_KNOTS('',3,(#26057,#26058,#26059,#26060,#26061,
#26062,#26063,#26064,#26065,#26066,#26067,#26068,#26069,#26070,#26071,#26072,
#26073,#26074,#26075,#26076,#26077,#26078,#26079,#26080,#26081,#26082,#26083,
#26084,#26085,#26086,#26087,#26088,#26089,#26090,#26091,#26092,#26093,#26094,
#26095,#26096),.UNSPECIFIED.,.F.,.F.,(4,3,3,3,3,3,3,3,3,3,3,3,3,4),(63.9467350810118,
64.2529456823854,64.7510305326364,65.2491153828875,65.7472002331385,66.2452850833896,
66.7433699336406,67.2414547838917,67.7395396341427,68.2376244843938,68.7357093346448,
69.2337941848959,69.7318790351469,70.2299203881914),.UNSPECIFIED.);
#5905=B_SPLINE_CURVE_WITH_KNOTS('',3,(#26101,#26102,#26103,#26104,#26105,
#26106,#26107,#26108,#26109,#26110,#26111,#26112,#26113,#26114,#26115,#26116,
#26117,#26118,#26119,#26120,#26121,#26122,#26123,#26124,#26125,#26126,#26127,
#26128,#26129,#26130,#26131,#26132,#26133,#26134,#26135,#26136,#26137,#26138,
#26139,#26140,#26141,#26142,#26143),.UNSPECIFIED.,.F.,.F.,(4,3,3,3,3,3,
3,3,3,3,3,3,3,3,4),(-79.4914564061798,-79.1954911899169,-78.6974063396658,
-78.1993214894147,-77.7012366391637,-77.2031517889127,-76.7050669386616,
-76.2069820884106,-75.7088972381595,-75.2108123879085,-74.7127275376574,
-74.2146426874064,-73.7165578371553,-73.2184729869043,-73.2082710990001),
 .UNSPECIFIED.);
#5906=B_SPLINE_CURVE_WITH_KNOTS('',3,(#26144,#26145,#26146,#26147,#26148,
#26149,#26150,#26151,#26152,#26153,#26154,#26155,#26156,#26157,#26158,#26159,
#26160,#26161,#26162,#26163,#26164,#26165,#26166,#26167,#26168,#26169,#26170,
#26171,#26172,#26173,#26174,#26175,#26176,#26177,#26178,#26179,#26180,#26181,
#26182,#26183),.UNSPECIFIED.,.F.,.F.,(4,3,3,3,3,3,3,3,3,3,3,3,3,4),(70.2299203881914,
70.728048735649,71.2261335859,71.7242184361511,72.2223032864022,72.7203881366532,
73.2184729869043,73.7165578371553,74.2146426874063,74.7127275376574,75.2108123879084,
75.7088972381595,76.2069820884106,76.513105695371),.UNSPECIFIED.);
#5907=B_SPLINE_CURVE_WITH_KNOTS('',3,(#26188,#26189,#26190,#26191,#26192,
#26193,#26194,#26195,#26196,#26197,#26198,#26199,#26200,#26201,#26202,#26203,
#26204,#26205,#26206,#26207,#26208,#26209,#26210,#26211,#26212,#26213,#26214,
#26215,#26216,#26217,#26218,#26219,#26220,#26221,#26222,#26223,#26224,#26225,
#26226,#26227,#26228,#26229,#26230),.UNSPECIFIED.,.F.,.F.,(4,3,3,3,3,3,
3,3,3,3,3,3,3,3,4),(-85.7746417133593,-85.6705942431805,-85.1725093929295,
-84.6744245426784,-84.1763396924274,-83.6782548421763,-83.1801699919253,
-82.6820851416742,-82.1840002914231,-81.6859154411721,-81.1878305909211,
-80.68974574067,-80.191660890419,-79.6935760401679,-79.4914564061798),
 .UNSPECIFIED.);
#5908=B_SPLINE_CURVE_WITH_KNOTS('',3,(#26231,#26232,#26233,#26234,#26235,
#26236,#26237,#26238,#26239,#26240,#26241,#26242,#26243,#26244,#26245,#26246,
#26247,#26248,#26249,#26250,#26251,#26252,#26253,#26254,#26255,#26256,#26257,
#26258,#26259,#26260,#26261,#26262,#26263,#26264,#26265,#26266,#26267,#26268,
#26269,#26270,#26271,#26272,#26273),.UNSPECIFIED.,.F.,.F.,(4,3,3,3,3,3,
3,3,3,3,3,3,3,3,4),(76.513105695371,76.7050669386616,77.2031517889126,77.7012366391637,
78.1993214894148,78.6974063396658,79.1954911899169,79.6935760401679,80.1916608904189,
80.68974574067,81.187830590921,81.6859154411721,82.1840002914232,82.6820851416742,
82.7962910025505),.UNSPECIFIED.);
#5909=B_SPLINE_CURVE_WITH_KNOTS('',3,(#26278,#26279,#26280,#26281,#26282,
#26283,#26284,#26285,#26286,#26287,#26288,#26289,#26290,#26291,#26292,#26293,
#26294,#26295,#26296,#26297,#26298,#26299,#26300,#26301,#26302,#26303,#26304,
#26305,#26306,#26307,#26308,#26309,#26310,#26311,#26312,#26313,#26314,#26315,
#26316,#26317),.UNSPECIFIED.,.F.,.F.,(4,3,3,3,3,3,3,3,3,3,3,3,3,4),(-92.0578270205389,
-91.6476124461931,-91.1495275959421,-90.651442745691,-90.15335789544,-89.6552730451889,
-89.1571881949379,-88.6591033446868,-88.1610184944358,-87.6629336441847,
-87.1648487939337,-86.6667639436826,-86.1686790934316,-85.7746417133593),
 .UNSPECIFIED.);
#5910=B_SPLINE_CURVE_WITH_KNOTS('',3,(#26318,#26319,#26320,#26321,#26322,
#26323,#26324,#26325,#26326,#26327,#26328,#26329,#26330,#26331,#26332,#26333,
#26334,#26335,#26336,#26337,#26338,#26339,#26340,#26341,#26342,#26343,#26344,
#26345,#26346,#26347,#26348,#26349,#26350,#26351,#26352,#26353,#26354,#26355,
#26356,#26357),.UNSPECIFIED.,.F.,.F.,(4,3,3,3,3,3,3,3,3,3,3,3,3,4),(82.7962910025505,
83.1801699919253,83.6782548421763,84.1763396924274,84.6744245426784,85.1725093929295,
85.6705942431805,86.1686790934315,86.6667639436826,87.1648487939336,87.6629336441847,
88.1610184944358,88.6591033446868,89.0794763097301),.UNSPECIFIED.);
#5911=B_SPLINE_CURVE_WITH_KNOTS('',3,(#26363,#26364,#26365,#26366,#26367,
#26368,#26369,#26370,#26371),.UNSPECIFIED.,.F.,.F.,(4,1,1,1,1,1,4),(103.672557568463,
103.760427844368,104.258512694619,104.75659754487,105.254682395122,105.752767245373,
106.176669420977),.UNSPECIFIED.);
#5912=B_SPLINE_CURVE_WITH_KNOTS('',3,(#26374,#26375,#26376,#26377,#26378,
#26379),.UNSPECIFIED.,.F.,.F.,(4,1,1,4),(103.672557568463,103.942187199755,
104.440272050006,104.938356900257),.UNSPECIFIED.);
#5913=B_SPLINE_CURVE_WITH_KNOTS('',3,(#26384,#26385,#26386,#26387,#26388,
#26389,#26390,#26391,#26392,#26393,#26394,#26395,#26396,#26397,#26398,#26399),
 .UNSPECIFIED.,.F.,.F.,(4,1,1,1,1,1,1,1,1,1,1,1,1,4),(97.3893722612836,
97.7834096413558,98.2814944916068,98.7795793418579,99.2776641921089,99.77574904236,
100.273833892611,100.771918742862,101.270003593113,101.768088443364,102.266173293615,
102.764258143866,103.262342994117,103.672557568463),.UNSPECIFIED.);
#5914=B_SPLINE_CURVE_WITH_KNOTS('',3,(#26400,#26401,#26402,#26403,#26404,
#26405,#26406,#26407,#26408,#26409,#26410,#26411,#26412,#26413,#26414,#26415,
#26416),.UNSPECIFIED.,.F.,.F.,(4,1,1,1,1,1,1,1,1,1,1,1,1,1,4),(97.3893722612836,
97.4670841464912,97.9651689967422,98.4632538469933,98.9613386972443,99.4594235474954,
99.9575083977464,100.455593247997,100.953678098249,101.4517629485,101.949847798751,
102.447932649002,102.946017499253,103.444102349504,103.672557568463),
 .UNSPECIFIED.);
#5915=B_SPLINE_CURVE_WITH_KNOTS('',3,(#26421,#26422,#26423,#26424,#26425,
#26426,#26427,#26428,#26429,#26430,#26431,#26432,#26433,#26434,#26435,#26436,
#26437),.UNSPECIFIED.,.F.,.F.,(4,1,1,1,1,1,1,1,1,1,1,1,1,1,4),(91.106186954104,
91.3083065880921,91.8063914383432,92.3044762885942,92.8025611388453,93.3006459890963,
93.7987308393474,94.2968156895984,94.7949005398495,95.2929853901005,95.7910702403516,
96.2891550906026,96.7872399408537,97.2853247911047,97.3893722612836),
 .UNSPECIFIED.);
#5916=B_SPLINE_CURVE_WITH_KNOTS('',3,(#26438,#26439,#26440,#26441,#26442,
#26443,#26444,#26445,#26446,#26447,#26448,#26449,#26450,#26451,#26452,#26453),
 .UNSPECIFIED.,.F.,.F.,(4,1,1,1,1,1,1,1,1,1,1,1,1,4),(91.106186954104,91.4900659434786,
91.9881507937297,92.4862356439807,92.9843204942318,93.4824053444828,93.9804901947338,
94.4785750449849,94.976659895236,95.474744745487,95.972829595738,96.4709144459891,
96.9689992962401,97.3893722612836),.UNSPECIFIED.);
#5917=B_SPLINE_CURVE_WITH_KNOTS('',3,(#26458,#26459,#26460,#26461,#26462,
#26463,#26464,#26465,#26466,#26467,#26468,#26469,#26470,#26471,#26472,#26473,
#26474),.UNSPECIFIED.,.F.,.F.,(4,1,1,1,1,1,1,1,1,1,1,1,1,1,4),(84.8230016469244,
84.8332035348285,85.3312883850795,85.8293732353306,86.3274580855816,86.8255429358327,
87.3236277860837,87.8217126363348,88.3197974865858,88.8178823368369,89.3159671870879,
89.814052037339,90.31213688759,90.8102217378411,91.106186954104),
 .UNSPECIFIED.);
#5918=B_SPLINE_CURVE_WITH_KNOTS('',3,(#26475,#26476,#26477,#26478,#26479,
#26480,#26481,#26482,#26483,#26484,#26485,#26486,#26487,#26488,#26489,#26490,
#26491),.UNSPECIFIED.,.F.,.F.,(4,1,1,1,1,1,1,1,1,1,1,1,1,1,4),(84.8230016469244,
85.014962890215,85.513047740466,86.0111325907171,86.5092174409681,87.0073022912192,
87.5053871414702,88.0034719917213,88.5015568419723,88.9996416922233,89.4977265424744,
89.9958113927255,90.4938962429765,90.9919810932276,91.106186954104),
 .UNSPECIFIED.);
#5919=B_SPLINE_CURVE_WITH_KNOTS('',3,(#26496,#26497,#26498,#26499,#26500,
#26501,#26502,#26503,#26504,#26505,#26506,#26507,#26508,#26509,#26510,#26511),
 .UNSPECIFIED.,.F.,.F.,(4,1,1,1,1,1,1,1,1,1,1,1,1,4),(78.5398163397448,
78.8561853318159,79.3542701820669,79.852355032318,80.350439882569,80.8485247328201,
81.3466095830711,81.8446944333222,82.3427792835733,82.8408641338243,83.3389489840753,
83.8370338343264,84.3351186845774,84.8230016469244),.UNSPECIFIED.);
#5920=B_SPLINE_CURVE_WITH_KNOTS('',3,(#26512,#26513,#26514,#26515,#26516,
#26517,#26518,#26519,#26520,#26521,#26522,#26523,#26524,#26525,#26526,#26527,
#26528),.UNSPECIFIED.,.F.,.F.,(4,1,1,1,1,1,1,1,1,1,1,1,1,1,4),(78.5398163397448,
78.5398598369513,79.0379446872024,79.5360295374534,80.0341143877045,80.5321992379555,
81.0302840882066,81.5283689384576,82.0264537887087,82.5245386389597,83.0226234892108,
83.5207083394618,84.0187931897129,84.5168780399639,84.8230016469244),
 .UNSPECIFIED.);
#5921=B_SPLINE_CURVE_WITH_KNOTS('',3,(#26533,#26534,#26535,#26536,#26537,
#26538,#26539,#26540,#26541,#26542,#26543,#26544,#26545,#26546,#26547,#26548,
#26549),.UNSPECIFIED.,.F.,.F.,(4,1,1,1,1,1,1,1,1,1,1,1,1,1,4),(72.2566310325652,
72.3810822785523,72.8791671288033,73.3772519790544,73.8753368293054,74.3734216795565,
74.8715065298075,75.3695913800586,75.8676762303096,76.3657610805606,76.8638459308117,
77.3619307810628,77.8600156313138,78.3581004815648,78.5398163397448),
 .UNSPECIFIED.);
#5922=B_SPLINE_CURVE_WITH_KNOTS('',3,(#26550,#26551,#26552,#26553,#26554,
#26555,#26556,#26557,#26558,#26559,#26560,#26561,#26562,#26563,#26564,#26565),
 .UNSPECIFIED.,.F.,.F.,(4,1,1,1,1,1,1,1,1,1,1,1,1,4),(72.2566310325652,
72.5628416339387,73.0609264841898,73.5590113344408,74.0570961846919,74.5551810349429,
75.053265885194,75.551350735445,76.0494355856961,76.5475204359471,77.0456052861982,
77.5436901364492,78.0417749867003,78.5398163397448),.UNSPECIFIED.);
#5923=B_SPLINE_CURVE_WITH_KNOTS('',3,(#26570,#26571,#26572,#26573,#26574,
#26575,#26576,#26577,#26578,#26579,#26580,#26581,#26582,#26583,#26584,#26585),
 .UNSPECIFIED.,.F.,.F.,(4,1,1,1,1,1,1,1,1,1,1,1,1,4),(65.9734457253856,
66.4040640755397,66.9021489257907,67.4002337760418,67.8983186262928,68.3964034765439,
68.8944883267949,69.392573177046,69.890658027297,70.3887428775481,70.8868277277991,
71.3849125780502,71.8829974283012,72.2566310325652),.UNSPECIFIED.);
#5924=B_SPLINE_CURVE_WITH_KNOTS('',3,(#26586,#26587,#26588,#26589,#26590,
#26591,#26592,#26593,#26594,#26595,#26596,#26597,#26598,#26599,#26600,#26601,
#26602),.UNSPECIFIED.,.F.,.F.,(4,1,1,1,1,1,1,1,1,1,1,1,1,1,4),(65.9734457253856,
66.0877385806751,66.5858234309261,67.0839082811772,67.5819931314282,68.0800779816793,
68.5781628319303,69.0762476821814,69.5743325324324,70.0724173826835,70.5705022329345,
71.0685870831856,71.5666719334366,72.0647567836877,72.2566310325652),
 .UNSPECIFIED.);
#5925=B_SPLINE_CURVE_WITH_KNOTS('',3,(#26607,#26608,#26609,#26610,#26611,
#26612,#26613,#26614,#26615,#26616,#26617,#26618,#26619,#26620,#26621),
 .UNSPECIFIED.,.F.,.F.,(4,1,1,1,1,1,1,1,1,1,1,1,4),(59.6902604182061,60.4270458725271,
61.4232155730292,61.9213004232802,62.4193852735313,62.9174701237823,63.4155549740334,
63.9136398242844,64.4117246745355,64.9098095247865,65.4078943750376,65.9059792252886,
65.9734457253856),.UNSPECIFIED.);
#5926=B_SPLINE_CURVE_WITH_KNOTS('',3,(#26622,#26623,#26624,#26625,#26626,
#26627,#26628,#26629,#26630,#26631,#26632,#26633,#26634,#26635,#26636,#26637),
 .UNSPECIFIED.,.F.,.F.,(4,1,1,1,1,1,1,1,1,1,1,1,1,4),(59.690260418206,60.1107203776625,
60.6088052279135,61.1068900781646,61.6049749284156,62.1030597786667,62.6011446289178,
63.0992294791688,63.5973143294198,64.0953991796709,64.5934840299219,65.091568880173,
65.589653730424,65.9734457253856),.UNSPECIFIED.);
#5927=B_SPLINE_CURVE_WITH_KNOTS('',3,(#26642,#26643,#26644,#26645,#26646,
#26647,#26648,#26649,#26650,#26651,#26652,#26653,#26654,#26655,#26656,#26657),
 .UNSPECIFIED.,.F.,.F.,(4,1,1,1,1,1,1,1,1,1,1,1,1,4),(53.4070751110264,
53.4538579690124,53.9519428192634,54.4500276695145,54.9481125197655,55.4461973700166,
55.9442822202676,56.4423670705187,56.9404519207697,57.4385367710208,57.9366216212718,
58.4347064715229,59.430876172025,59.6902604182061),.UNSPECIFIED.);
#5928=B_SPLINE_CURVE_WITH_KNOTS('',3,(#26658,#26659,#26660,#26661,#26662,
#26663,#26664,#26665,#26666,#26667,#26668,#26669,#26670,#26671),
 .UNSPECIFIED.,.F.,.F.,(4,1,1,1,1,1,1,1,1,1,1,4),(53.4070751110264,53.6356173243989,
54.1337021746499,54.631787024901,55.129871875152,56.1260415756541,57.1222112761562,
58.1183809766583,58.6164658269093,59.1145506771604,59.6126355274115,59.690260418206),
 .UNSPECIFIED.);
#5929=B_SPLINE_CURVE_WITH_KNOTS('',3,(#26676,#26677,#26678,#26679,#26680,
#26681,#26682,#26683,#26684,#26685,#26686,#26687,#26688,#26689,#26690,#26691),
 .UNSPECIFIED.,.F.,.F.,(4,1,1,1,1,1,1,1,1,1,1,1,1,4),(47.1238898038469,
47.4768397659998,47.9749246162508,48.4730094665019,48.9710943167529,49.469179167004,
49.967264017255,50.4653488675061,50.9634337177571,51.4615185680082,51.9596034182592,
52.4576882685103,52.9557731187613,53.4070751110264),.UNSPECIFIED.);
#5930=B_SPLINE_CURVE_WITH_KNOTS('',3,(#26692,#26693,#26694,#26695,#26696,
#26697,#26698,#26699,#26700,#26701,#26702,#26703,#26704,#26705,#26706,#26707,
#26708),.UNSPECIFIED.,.F.,.F.,(4,1,1,1,1,1,1,1,1,1,1,1,1,1,4),(47.1238898038469,
47.1605142711352,47.6585991213863,48.1566839716373,48.6547688218884,49.1528536721394,
49.6509385223905,50.1490233726415,50.6471082228926,51.1451930731436,51.6432779233947,
52.1413627736457,52.6394476238968,53.1375324741478,53.4070751110264),
 .UNSPECIFIED.);
#5931=B_SPLINE_CURVE_WITH_KNOTS('',3,(#26713,#26714,#26715,#26716,#26717,
#26718,#26719,#26720,#26721,#26722,#26723,#26724,#26725,#26726,#26727,#26728,
#26729),.UNSPECIFIED.,.F.,.F.,(4,1,1,1,1,1,1,1,1,1,1,1,1,1,4),(40.8407044966673,
41.0017367127361,41.4998215629872,41.9979064132382,42.4959912634893,42.9940761137403,
43.4921609639914,43.9902458142424,44.4883306644935,44.9864155147445,45.4845003649956,
45.9825852152466,46.4806700654977,46.9787549157487,47.1238898038469),
 .UNSPECIFIED.);
#5932=B_SPLINE_CURVE_WITH_KNOTS('',3,(#26730,#26731,#26732,#26733,#26734,
#26735,#26736,#26737,#26738,#26739,#26740,#26741,#26742,#26743,#26744,#26745),
 .UNSPECIFIED.,.F.,.F.,(4,1,1,1,1,1,1,1,1,1,1,1,1,4),(40.8407044966673,
41.1834960681226,41.6815809183737,42.1796657686247,42.6777506188758,43.1758354691268,
43.6739203193779,44.1720051696289,44.67009001988,45.168174870131,45.6662597203821,
46.1643445706331,46.6624294208842,47.1238898038469),.UNSPECIFIED.);
#5933=B_SPLINE_CURVE_WITH_KNOTS('',3,(#26750,#26751,#26752,#26753,#26754,
#26755,#26756,#26757,#26758,#26759,#26760,#26761,#26762,#26763,#26764,#26765),
 .UNSPECIFIED.,.F.,.F.,(4,1,1,1,1,1,1,1,1,1,1,1,1,4),(34.5575191894876,
35.0247185097235,35.5228033599746,36.0208882102256,36.5189730604767,37.0170579107277,
37.5151427609788,38.0132276112299,38.5113124614809,39.0093973117319,39.507482161983,
40.005567012234,40.5036518624851,40.8407044966673),.UNSPECIFIED.);
#5934=B_SPLINE_CURVE_WITH_KNOTS('',3,(#26766,#26767,#26768,#26769,#26770,
#26771,#26772,#26773,#26774,#26775,#26776,#26777,#26778,#26779,#26780,#26781,
#26782),.UNSPECIFIED.,.F.,.F.,(4,1,1,1,1,1,1,1,1,1,1,1,1,1,4),(34.5575191894876,
34.708393014859,35.20647786511,35.7045627153611,36.2026475656121,36.7007324158632,
37.1988172661142,37.6969021163653,38.1949869666163,38.6930718168674,39.1911566671184,
39.6892415173695,40.1873263676205,40.6854112178716,40.8407044966673),
 .UNSPECIFIED.);
#5935=B_SPLINE_CURVE_WITH_KNOTS('',3,(#26787,#26788,#26789,#26790,#26791,
#26792,#26793,#26794,#26795,#26796,#26797,#26798,#26799,#26800,#26801,#26802,
#26803),.UNSPECIFIED.,.F.,.F.,(4,1,1,1,1,1,1,1,1,1,1,1,1,1,4),(28.2743338823081,
28.5496154564599,29.047700306711,29.545785156962,30.0438700072131,30.5419548574641,
31.0400397077152,31.5381245579662,32.0362094082173,32.5342942584683,33.0323791087194,
33.5304639589704,34.0285488092214,34.5266336594725,34.5575191894876),
 .UNSPECIFIED.);
#5936=B_SPLINE_CURVE_WITH_KNOTS('',3,(#26804,#26805,#26806,#26807,#26808,
#26809,#26810,#26811,#26812,#26813,#26814,#26815,#26816,#26817,#26818,#26819),
 .UNSPECIFIED.,.F.,.F.,(4,1,1,1,1,1,1,1,1,1,1,1,1,4),(28.274333882308,28.7313748118464,
29.2294596620974,29.7275445123485,30.2256293625995,30.7237142128506,31.2217990631016,
31.7198839133527,32.2179687636037,32.7160536138548,33.2141384641058,33.7122233143569,
34.2103081646079,34.5575191894876),.UNSPECIFIED.);
#5937=B_SPLINE_CURVE_WITH_KNOTS('',3,(#26824,#26825,#26826,#26827,#26828,
#26829,#26830,#26831,#26832,#26833,#26834,#26835,#26836,#26837,#26838,#26839,
#26840),.UNSPECIFIED.,.F.,.F.,(4,1,1,1,1,1,1,1,1,1,1,1,1,1,4),(21.9911485751285,
22.0745124031963,22.5725972534473,23.0706821036984,23.5687669539494,24.0668518042005,
24.5649366544515,25.0630215047026,25.5611063549536,26.0591912052047,26.5572760554557,
27.0553609057068,27.5534457559578,28.0515306062089,28.2743338823081),
 .UNSPECIFIED.);
#5938=B_SPLINE_CURVE_WITH_KNOTS('',3,(#26841,#26842,#26843,#26844,#26845,
#26846,#26847,#26848,#26849,#26850,#26851,#26852,#26853,#26854,#26855,#26856,
#26857),.UNSPECIFIED.,.F.,.F.,(4,1,1,1,1,1,1,1,1,1,1,1,1,1,4),(21.9911485751285,
22.2562717585827,22.7543566088338,23.2524414590848,23.7505263093359,24.2486111595869,
24.746696009838,25.244780860089,25.7428657103401,26.2409505605911,26.7390354108422,
27.2371202610932,27.7352051113443,28.2332899615953,28.274333882308),
 .UNSPECIFIED.);
#5939=B_SPLINE_CURVE_WITH_KNOTS('',3,(#26862,#26863,#26864,#26865,#26866,
#26867,#26868,#26869,#26870,#26871,#26872,#26873,#26874,#26875,#26876,#26877),
 .UNSPECIFIED.,.F.,.F.,(4,1,1,1,1,1,1,1,1,1,1,1,1,4),(15.7079632679489,
16.0974942001837,16.5955790504347,17.0936639006858,17.5917487509368,18.0898336011879,
18.5879184514389,19.08600330169,19.584088151941,20.0821730021921,20.5802578524431,
21.0783427026942,21.5764275529452,21.9911485751285),.UNSPECIFIED.);
#5940=B_SPLINE_CURVE_WITH_KNOTS('',3,(#26878,#26879,#26880,#26881,#26882,
#26883,#26884,#26885,#26886,#26887,#26888,#26889,#26890,#26891,#26892,#26893,
#26894),.UNSPECIFIED.,.F.,.F.,(4,1,1,1,1,1,1,1,1,1,1,1,1,1,4),(15.7079632679489,
15.7811687053191,16.2792535555702,16.7773384058212,17.2754232560723,17.7735081063233,
18.2715929565744,18.7696778068254,19.2677626570764,19.7658475073275,20.2639323575785,
20.7620172078296,21.2601020580806,21.7581869083317,21.9911485751285),
 .UNSPECIFIED.);
#5941=B_SPLINE_CURVE_WITH_KNOTS('',3,(#26900,#26901,#26902,#26903,#26904,
#26905,#26906,#26907,#26908,#26909,#26910,#26911,#26912,#26913,#26914,#26915),
 .UNSPECIFIED.,.F.,.F.,(4,3,3,3,3,4),(-4.09323272002468,-3.9846788020084,
-3.48659395175735,-2.9885091015063,-2.49042425125525,-2.06652207565086),
 .UNSPECIFIED.);
#5942=B_SPLINE_CURVE_WITH_KNOTS('',3,(#26918,#26919,#26920,#26921,#26922,
#26923,#26924,#26925,#26926,#26927),.UNSPECIFIED.,.F.,.F.,(4,3,3,4),(0.,
0.498084850251037,0.996169700502091,1.11488200921589),.UNSPECIFIED.);
#5943=B_SPLINE_CURVE_WITH_KNOTS('',3,(#26932,#26933,#26934,#26935,#26936,
#26937,#26938,#26939,#26940,#26941,#26942,#26943,#26944,#26945,#26946,#26947,
#26948,#26949,#26950,#26951,#26952,#26953,#26954,#26955,#26956,#26957,#26958,
#26959,#26960,#26961,#26962,#26963,#26964,#26965,#26966,#26967,#26968,#26969,
#26970,#26971),.UNSPECIFIED.,.F.,.F.,(4,3,3,3,3,3,3,3,3,3,3,3,3,4),(-10.3764180272043,
-9.96169700502099,-9.46361215476994,-8.96552730451889,-8.46744245426784,
-7.96935760401679,-7.47127275376574,-6.97318790351469,-6.47510305326364,
-5.97701820301259,-5.47893335276154,-4.98084850251049,-4.48276365225945,
-4.09323272002468),.UNSPECIFIED.);
#5944=B_SPLINE_CURVE_WITH_KNOTS('',3,(#26972,#26973,#26974,#26975,#26976,
#26977,#26978,#26979,#26980,#26981,#26982,#26983,#26984,#26985,#26986,#26987,
#26988,#26989,#26990,#26991,#26992,#26993,#26994,#26995,#26996,#26997,#26998,
#26999,#27000,#27001,#27002,#27003,#27004,#27005,#27006,#27007,#27008,#27009,
#27010,#27011),.UNSPECIFIED.,.F.,.F.,(4,3,3,3,3,3,3,3,3,3,3,3,3,4),(1.11488200921589,
1.49425455075314,1.99233940100419,2.49042425125524,2.98850910150629,3.48659395175734,
3.98467880200839,4.48276365225944,4.98084850251049,5.47893335276154,5.97701820301259,
6.47510305326364,6.97318790351469,7.39806731639547),.UNSPECIFIED.);
#5945=B_SPLINE_CURVE_WITH_KNOTS('',3,(#27016,#27017,#27018,#27019,#27020,
#27021,#27022,#27023,#27024,#27025,#27026,#27027,#27028,#27029,#27030,#27031,
#27032,#27033,#27034,#27035,#27036,#27037,#27038,#27039,#27040,#27041,#27042,
#27043,#27044,#27045,#27046,#27047,#27048,#27049,#27050,#27051,#27052,#27053,
#27054,#27055,#27056,#27057,#27058),.UNSPECIFIED.,.F.,.F.,(4,3,3,3,3,3,
3,3,3,3,3,3,3,3,4),(-16.6596033343839,-16.4368000582846,-15.9387152080336,
-15.4406303577825,-14.9425455075315,-14.4444606572804,-13.9463758070294,
-13.4482909567783,-12.9502061065273,-12.4521212562762,-11.9540364060252,
-11.4559515557741,-10.9578667055231,-10.459781855272,-10.3764180272043),
 .UNSPECIFIED.);
#5946=B_SPLINE_CURVE_WITH_KNOTS('',3,(#27059,#27060,#27061,#27062,#27063,
#27064,#27065,#27066,#27067,#27068,#27069,#27070,#27071,#27072,#27073,#27074,
#27075,#27076,#27077,#27078,#27079,#27080,#27081,#27082,#27083,#27084,#27085,
#27086,#27087,#27088,#27089,#27090,#27091,#27092,#27093,#27094,#27095,#27096,
#27097,#27098,#27099,#27100,#27101),.UNSPECIFIED.,.F.,.F.,(4,3,3,3,3,3,
3,3,3,3,3,3,3,3,4),(7.39806731639547,7.47127275376574,7.96935760401679,
8.46744245426784,8.96552730451889,9.46361215476994,9.96169700502099,10.459781855272,
10.9578667055231,11.4559515557741,11.9540364060252,12.4521212562762,12.9502061065273,
13.4482909567783,13.681252623575),.UNSPECIFIED.);
#5947=B_SPLINE_CURVE_WITH_KNOTS('',3,(#27106,#27107,#27108,#27109,#27110,
#27111,#27112,#27113,#27114,#27115,#27116,#27117,#27118,#27119,#27120,#27121,
#27122,#27123,#27124,#27125,#27126,#27127,#27128,#27129,#27130,#27131,#27132,
#27133,#27134,#27135,#27136,#27137,#27138,#27139,#27140,#27141,#27142,#27143,
#27144,#27145,#27146,#27147,#27148),.UNSPECIFIED.,.F.,.F.,(4,3,3,3,3,3,
3,3,3,3,3,3,3,3,4),(-22.9427886415634,-22.9119031115483,-22.4138182612972,
-21.9157334110462,-21.4176485607951,-20.9195637105441,-20.421478860293,
-19.923394010042,-19.4253091597909,-18.9272243095399,-18.4291394592888,
-17.9310546090378,-17.4329697587867,-16.9348849085357,-16.6596033343839),
 .UNSPECIFIED.);
#5948=B_SPLINE_CURVE_WITH_KNOTS('',3,(#27149,#27150,#27151,#27152,#27153,
#27154,#27155,#27156,#27157,#27158,#27159,#27160,#27161,#27162,#27163,#27164,
#27165,#27166,#27167,#27168,#27169,#27170,#27171,#27172,#27173,#27174,#27175,
#27176,#27177,#27178,#27179,#27180,#27181,#27182,#27183,#27184,#27185,#27186,
#27187,#27188,#27189,#27190,#27191),.UNSPECIFIED.,.F.,.F.,(4,3,3,3,3,3,
3,3,3,3,3,3,3,3,4),(13.681252623575,13.9463758070294,14.4444606572804,14.9425455075315,
15.4406303577825,15.9387152080336,16.4368000582846,16.9348849085357,17.4329697587867,
17.9310546090378,18.4291394592888,18.9272243095399,19.4253091597909,19.923394010042,
19.9644379307546),.UNSPECIFIED.);
#5949=B_SPLINE_CURVE_WITH_KNOTS('',3,(#27196,#27197,#27198,#27199,#27200,
#27201,#27202,#27203,#27204,#27205,#27206,#27207,#27208,#27209,#27210,#27211,
#27212,#27213,#27214,#27215,#27216,#27217,#27218,#27219,#27220,#27221,#27222,
#27223,#27224,#27225,#27226,#27227,#27228,#27229,#27230,#27231,#27232,#27233,
#27234,#27235),.UNSPECIFIED.,.F.,.F.,(4,3,3,3,3,3,3,3,3,3,3,3,3,4),(-29.225973948743,
-28.8889213145609,-28.3908364643098,-27.8927516140588,-27.3946667638077,
-26.8965819135567,-26.3984970633056,-25.9004122130546,-25.4023273628035,
-24.9042425125525,-24.4061576623014,-23.9080728120504,-23.4099879617993,
-22.9427886415634),.UNSPECIFIED.);
#5950=B_SPLINE_CURVE_WITH_KNOTS('',3,(#27236,#27237,#27238,#27239,#27240,
#27241,#27242,#27243,#27244,#27245,#27246,#27247,#27248,#27249,#27250,#27251,
#27252,#27253,#27254,#27255,#27256,#27257,#27258,#27259,#27260,#27261,#27262,
#27263,#27264,#27265,#27266,#27267,#27268,#27269,#27270,#27271,#27272,#27273,
#27274,#27275),.UNSPECIFIED.,.F.,.F.,(4,3,3,3,3,3,3,3,3,3,3,3,3,4),(19.9644379307546,
20.421478860293,20.9195637105441,21.4176485607951,21.9157334110462,22.4138182612972,
22.9119031115483,23.4099879617993,23.9080728120504,24.4061576623014,24.9042425125525,
25.4023273628035,25.9004122130546,26.2476232379342),.UNSPECIFIED.);
#5951=B_SPLINE_CURVE_WITH_KNOTS('',3,(#27280,#27281,#27282,#27283,#27284,
#27285,#27286,#27287,#27288,#27289,#27290,#27291,#27292,#27293,#27294,#27295,
#27296,#27297,#27298,#27299,#27300,#27301,#27302,#27303,#27304,#27305,#27306,
#27307,#27308,#27309,#27310,#27311,#27312,#27313,#27314,#27315,#27316,#27317,
#27318,#27319,#27320,#27321,#27322),.UNSPECIFIED.,.F.,.F.,(4,3,3,3,3,3,
3,3,3,3,3,3,3,3,4),(-35.5091592559226,-35.3640243678245,-34.8659395175735,
-34.3678546673224,-33.8697698170714,-33.3716849668203,-32.8736001165693,
-32.3755152663182,-31.8774304160672,-31.3793455658161,-30.8812607155651,
-30.383175865314,-29.885091015063,-29.3870061648119,-29.225973948743),
 .UNSPECIFIED.);
#5952=B_SPLINE_CURVE_WITH_KNOTS('',3,(#27323,#27324,#27325,#27326,#27327,
#27328,#27329,#27330,#27331,#27332,#27333,#27334,#27335,#27336,#27337,#27338,
#27339,#27340,#27341,#27342,#27343,#27344,#27345,#27346,#27347,#27348,#27349,
#27350,#27351,#27352,#27353,#27354,#27355,#27356,#27357,#27358,#27359,#27360,
#27361,#27362,#27363,#27364,#27365),.UNSPECIFIED.,.F.,.F.,(4,3,3,3,3,3,
3,3,3,3,3,3,3,3,4),(26.2476232379342,26.3984970633056,26.8965819135567,
27.3946667638077,27.8927516140588,28.3908364643098,28.8889213145609,29.3870061648119,
29.885091015063,30.383175865314,30.8812607155651,31.3793455658161,31.8774304160672,
32.3755152663182,32.5308085451138),.UNSPECIFIED.);
#5953=B_SPLINE_CURVE_WITH_KNOTS('',3,(#27370,#27371,#27372,#27373,#27374,
#27375,#27376,#27377,#27378,#27379,#27380,#27381,#27382,#27383,#27384,#27385,
#27386,#27387,#27388,#27389,#27390,#27391,#27392,#27393,#27394,#27395,#27396,
#27397,#27398,#27399,#27400,#27401,#27402,#27403,#27404,#27405,#27406,#27407,
#27408,#27409),.UNSPECIFIED.,.F.,.F.,(4,3,3,3,3,3,3,3,3,3,3,3,3,4),(-41.7923445631022,
-41.3410425708371,-40.842957720586,-40.344872870335,-39.846788020084,-39.3487031698329,
-38.8506183195819,-38.3525334693308,-37.8544486190798,-37.3563637688287,
-36.8582789185777,-36.3601940683266,-35.8621092180756,-35.5091592559226),
 .UNSPECIFIED.);
#5954=B_SPLINE_CURVE_WITH_KNOTS('',3,(#27410,#27411,#27412,#27413,#27414,
#27415,#27416,#27417,#27418,#27419,#27420,#27421,#27422,#27423,#27424,#27425,
#27426,#27427,#27428,#27429,#27430,#27431,#27432,#27433,#27434,#27435,#27436,
#27437,#27438,#27439,#27440,#27441,#27442,#27443,#27444,#27445,#27446,#27447,
#27448,#27449),.UNSPECIFIED.,.F.,.F.,(4,3,3,3,3,3,3,3,3,3,3,3,3,4),(32.5308085451138,
32.8736001165693,33.3716849668203,33.8697698170714,34.3678546673224,34.8659395175735,
35.3640243678245,35.8621092180756,36.3601940683266,36.8582789185777,37.3563637688287,
37.8544486190798,38.3525334693308,38.8139938522934),.UNSPECIFIED.);
#5955=B_SPLINE_CURVE_WITH_KNOTS('',3,(#27454,#27455,#27456,#27457,#27458,
#27459,#27460,#27461,#27462,#27463,#27464,#27465,#27466,#27467,#27468,#27469,
#27470,#27471,#27472,#27473,#27474,#27475,#27476,#27477,#27478,#27479,#27480,
#27481,#27482,#27483,#27484,#27485,#27486,#27487,#27488,#27489,#27490,#27491,
#27492,#27493),.UNSPECIFIED.,.F.,.F.,(4,3,3,3,3,3,3,3,3,3,3,3,3,4),(-48.0755298702818,
-47.8161456241007,-46.8199759235987,-46.3218910733476,-45.8238062230965,
-45.3257213728455,-44.8276365225945,-44.3295516723434,-43.8314668220924,
-43.3333819718413,-42.8352971215903,-42.3372122713392,-41.8391274210882,
-41.7923445631022),.UNSPECIFIED.);
#5956=B_SPLINE_CURVE_WITH_KNOTS('',3,(#27494,#27495,#27496,#27497,#27498,
#27499,#27500,#27501,#27502,#27503,#27504,#27505,#27506,#27507,#27508,#27509,
#27510,#27511,#27512,#27513,#27514,#27515,#27516,#27517,#27518,#27519,#27520,
#27521,#27522,#27523,#27524,#27525,#27526,#27527,#27528,#27529,#27530,#27531,
#27532,#27533,#27534,#27535,#27536),.UNSPECIFIED.,.F.,.F.,(4,3,3,3,3,3,
3,3,3,3,3,3,3,3,4),(38.8139938522934,38.8506183195819,39.3487031698329,
39.846788020084,40.344872870335,40.842957720586,41.3410425708371,41.8391274210882,
42.3372122713392,42.8352971215903,43.3333819718413,43.8314668220923,44.3295516723434,
44.8276365225945,45.097179159473),.UNSPECIFIED.);
#5957=B_SPLINE_CURVE_WITH_KNOTS('',3,(#27541,#27542,#27543,#27544,#27545,
#27546,#27547,#27548,#27549,#27550,#27551,#27552,#27553,#27554,#27555,#27556,
#27557,#27558,#27559,#27560,#27561,#27562,#27563,#27564,#27565,#27566,#27567,
#27568,#27569,#27570,#27571,#27572,#27573,#27574,#27575,#27576,#27577),
 .UNSPECIFIED.,.F.,.F.,(4,3,3,3,3,3,3,3,3,3,3,3,4),(-54.3587151774614,-54.2912486773644,
-53.7931638271133,-53.2950789768623,-52.7969941266112,-52.2989092763602,
-51.8008244261091,-51.3027395758581,-50.804654725607,-50.306569875356,-49.808485025105,
-48.8123153246028,-48.0755298702818),.UNSPECIFIED.);
#5958=B_SPLINE_CURVE_WITH_KNOTS('',3,(#27578,#27579,#27580,#27581,#27582,
#27583,#27584,#27585,#27586,#27587,#27588,#27589,#27590,#27591,#27592,#27593,
#27594,#27595,#27596,#27597,#27598,#27599,#27600,#27601,#27602,#27603,#27604,
#27605,#27606,#27607,#27608,#27609,#27610,#27611),.UNSPECIFIED.,.F.,.F.,
(4,3,3,3,3,3,3,3,3,3,3,4),(45.097179159473,45.3257213728455,45.8238062230965,
46.3218910733476,46.8199759235987,47.8161456241007,48.8123153246028,49.808485025105,
50.306569875356,50.8046547256071,51.3027395758581,51.3803644666526),
 .UNSPECIFIED.);
#5959=B_SPLINE_CURVE_WITH_KNOTS('',3,(#27616,#27617,#27618,#27619,#27620,
#27621,#27622,#27623,#27624,#27625,#27626,#27627,#27628,#27629,#27630,#27631,
#27632,#27633,#27634,#27635,#27636,#27637,#27638,#27639,#27640,#27641,#27642,
#27643,#27644,#27645,#27646,#27647,#27648,#27649,#27650,#27651,#27652,#27653,
#27654,#27655),.UNSPECIFIED.,.F.,.F.,(4,3,3,3,3,3,3,3,3,3,3,3,3,4),(-60.641900484641,
-60.268266880377,-59.7701820301259,-59.2720971798749,-58.7740123296238,
-58.2759274793728,-57.7778426291217,-57.2797577788707,-56.7816729286196,
-56.2835880783686,-55.7855032281175,-55.2874183778665,-54.7893335276154,
-54.3587151774614),.UNSPECIFIED.);
#5960=B_SPLINE_CURVE_WITH_KNOTS('',3,(#27656,#27657,#27658,#27659,#27660,
#27661,#27662,#27663,#27664,#27665,#27666,#27667,#27668,#27669,#27670,#27671,
#27672,#27673,#27674,#27675,#27676,#27677,#27678,#27679,#27680,#27681,#27682,
#27683,#27684,#27685,#27686,#27687,#27688,#27689,#27690,#27691,#27692,#27693,
#27694,#27695),.UNSPECIFIED.,.F.,.F.,(4,3,3,3,3,3,3,3,3,3,3,3,3,4),(51.3803644666526,
51.8008244261092,52.2989092763602,52.7969941266112,53.2950789768623,53.7931638271133,
54.2912486773644,54.7893335276154,55.2874183778665,55.7855032281175,56.2835880783686,
56.7816729286196,57.2797577788707,57.6635497738322),.UNSPECIFIED.);
#5961=B_SPLINE_CURVE_WITH_KNOTS('',3,(#27700,#27701,#27702,#27703,#27704,
#27705,#27706,#27707,#27708,#27709,#27710,#27711,#27712,#27713,#27714,#27715,
#27716,#27717,#27718,#27719,#27720,#27721,#27722,#27723,#27724,#27725,#27726,
#27727,#27728,#27729,#27730,#27731,#27732,#27733,#27734,#27735,#27736,#27737,
#27738,#27739,#27740,#27741,#27742),.UNSPECIFIED.,.F.,.F.,(4,3,3,3,3,3,
3,3,3,3,3,3,3,3,4),(-66.9250857918206,-66.7433699336406,-66.2452850833896,
-65.7472002331385,-65.2491153828875,-64.7510305326364,-64.2529456823854,
-63.7548608321343,-63.2567759818833,-62.7586911316322,-62.2606062813812,
-61.7625214311301,-61.2644365808791,-60.766351730628,-60.641900484641),
 .UNSPECIFIED.);
#5962=B_SPLINE_CURVE_WITH_KNOTS('',3,(#27743,#27744,#27745,#27746,#27747,
#27748,#27749,#27750,#27751,#27752,#27753,#27754,#27755,#27756,#27757,#27758,
#27759,#27760,#27761,#27762,#27763,#27764,#27765,#27766,#27767,#27768,#27769,
#27770,#27771,#27772,#27773,#27774,#27775,#27776,#27777,#27778,#27779,#27780,
#27781,#27782,#27783,#27784,#27785),.UNSPECIFIED.,.F.,.F.,(4,3,3,3,3,3,
3,3,3,3,3,3,3,3,4),(57.6635497738322,57.7778426291217,58.2759274793728,
58.7740123296238,59.2720971798749,59.7701820301259,60.268266880377,60.766351730628,
61.2644365808791,61.7625214311301,62.2606062813812,62.7586911316322,63.2567759818833,
63.7548608321343,63.9467350810118),.UNSPECIFIED.);
#5963=B_SPLINE_CURVE_WITH_KNOTS('',3,(#27790,#27791,#27792,#27793,#27794,
#27795,#27796,#27797,#27798,#27799,#27800,#27801,#27802,#27803,#27804,#27805,
#27806,#27807,#27808,#27809,#27810,#27811,#27812,#27813,#27814,#27815,#27816,
#27817,#27818,#27819,#27820,#27821,#27822,#27823,#27824,#27825,#27826,#27827,
#27828,#27829),.UNSPECIFIED.,.F.,.F.,(4,3,3,3,3,3,3,3,3,3,3,3,3,4),(-73.2082710990002,
-72.7203881366532,-72.2223032864022,-71.7242184361511,-71.2261335859001,
-70.728048735649,-70.229963885398,-69.7318790351469,-69.2337941848959,-68.7357093346448,
-68.2376244843938,-67.7395396341427,-67.2414547838917,-66.9250857918206),
 .UNSPECIFIED.);
#5964=B_SPLINE_CURVE_WITH_KNOTS('',3,(#27830,#27831,#27832,#27833,#27834,
#27835,#27836,#27837,#27838,#27839,#27840,#27841,#27842,#27843,#27844,#27845,
#27846,#27847,#27848,#27849,#27850,#27851,#27852,#27853,#27854,#27855,#27856,
#27857,#27858,#27859,#27860,#27861,#27862,#27863,#27864,#27865,#27866,#27867,
#27868,#27869),.UNSPECIFIED.,.F.,.F.,(4,3,3,3,3,3,3,3,3,3,3,3,3,4),(63.9467350810118,
64.2529456823854,64.7510305326364,65.2491153828875,65.7472002331385,66.2452850833896,
66.7433699336406,67.2414547838917,67.7395396341427,68.2376244843938,68.7357093346448,
69.2337941848959,69.7318790351469,70.2299203881914),.UNSPECIFIED.);
#5965=B_SPLINE_CURVE_WITH_KNOTS('',3,(#27874,#27875,#27876,#27877,#27878,
#27879,#27880,#27881,#27882,#27883,#27884,#27885,#27886,#27887,#27888,#27889,
#27890,#27891,#27892,#27893,#27894,#27895,#27896,#27897,#27898,#27899,#27900,
#27901,#27902,#27903,#27904,#27905,#27906,#27907,#27908,#27909,#27910,#27911,
#27912,#27913,#27914,#27915,#27916),.UNSPECIFIED.,.F.,.F.,(4,3,3,3,3,3,
3,3,3,3,3,3,3,3,4),(-79.4914564061798,-79.1954911899169,-78.6974063396658,
-78.1993214894148,-77.7012366391637,-77.2031517889127,-76.7050669386616,
-76.2069820884106,-75.7088972381595,-75.2108123879085,-74.7127275376574,
-74.2146426874064,-73.7165578371553,-73.2184729869043,-73.2082710990002),
 .UNSPECIFIED.);
#5966=B_SPLINE_CURVE_WITH_KNOTS('',3,(#27917,#27918,#27919,#27920,#27921,
#27922,#27923,#27924,#27925,#27926,#27927,#27928,#27929,#27930,#27931,#27932,
#27933,#27934,#27935,#27936,#27937,#27938,#27939,#27940,#27941,#27942,#27943,
#27944,#27945,#27946,#27947,#27948,#27949,#27950,#27951,#27952,#27953,#27954,
#27955,#27956),.UNSPECIFIED.,.F.,.F.,(4,3,3,3,3,3,3,3,3,3,3,3,3,4),(70.2299203881914,
70.728048735649,71.2261335859001,71.7242184361511,72.2223032864022,72.7203881366532,
73.2184729869043,73.7165578371553,74.2146426874064,74.7127275376574,75.2108123879085,
75.7088972381595,76.2069820884106,76.513105695371),.UNSPECIFIED.);
#5967=B_SPLINE_CURVE_WITH_KNOTS('',3,(#27961,#27962,#27963,#27964,#27965,
#27966,#27967,#27968,#27969,#27970,#27971,#27972,#27973,#27974,#27975,#27976,
#27977,#27978,#27979,#27980,#27981,#27982,#27983,#27984,#27985,#27986,#27987,
#27988,#27989,#27990,#27991,#27992,#27993,#27994,#27995,#27996,#27997,#27998,
#27999,#28000,#28001,#28002,#28003),.UNSPECIFIED.,.F.,.F.,(4,3,3,3,3,3,
3,3,3,3,3,3,3,3,4),(-85.7746417133593,-85.6705942431805,-85.1725093929295,
-84.6744245426784,-84.1763396924274,-83.6782548421763,-83.1801699919253,
-82.6820851416742,-82.1840002914232,-81.6859154411721,-81.1878305909211,
-80.68974574067,-80.191660890419,-79.6935760401679,-79.4914564061798),
 .UNSPECIFIED.);
#5968=B_SPLINE_CURVE_WITH_KNOTS('',3,(#28004,#28005,#28006,#28007,#28008,
#28009,#28010,#28011,#28012,#28013,#28014,#28015,#28016,#28017,#28018,#28019,
#28020,#28021,#28022,#28023,#28024,#28025,#28026,#28027,#28028,#28029,#28030,
#28031,#28032,#28033,#28034,#28035,#28036,#28037,#28038,#28039,#28040,#28041,
#28042,#28043,#28044,#28045,#28046),.UNSPECIFIED.,.F.,.F.,(4,3,3,3,3,3,
3,3,3,3,3,3,3,3,4),(76.513105695371,76.7050669386616,77.2031517889126,77.7012366391637,
78.1993214894147,78.6974063396658,79.1954911899169,79.6935760401679,80.1916608904189,
80.68974574067,81.1878305909211,81.6859154411721,82.1840002914231,82.6820851416742,
82.7962910025506),.UNSPECIFIED.);
#5969=B_SPLINE_CURVE_WITH_KNOTS('',3,(#28051,#28052,#28053,#28054,#28055,
#28056,#28057,#28058,#28059,#28060,#28061,#28062,#28063,#28064,#28065,#28066,
#28067,#28068,#28069,#28070,#28071,#28072,#28073,#28074,#28075,#28076,#28077,
#28078,#28079,#28080,#28081,#28082,#28083,#28084,#28085,#28086,#28087,#28088,
#28089,#28090),.UNSPECIFIED.,.F.,.F.,(4,3,3,3,3,3,3,3,3,3,3,3,3,4),(-92.057827020539,
-91.6476124461931,-91.1495275959421,-90.651442745691,-90.15335789544,-89.6552730451889,
-89.1571881949379,-88.6591033446868,-88.1610184944358,-87.6629336441847,
-87.1648487939337,-86.6667639436826,-86.1686790934316,-85.7746417133593),
 .UNSPECIFIED.);
#5970=B_SPLINE_CURVE_WITH_KNOTS('',3,(#28091,#28092,#28093,#28094,#28095,
#28096,#28097,#28098,#28099,#28100,#28101,#28102,#28103,#28104,#28105,#28106,
#28107,#28108,#28109,#28110,#28111,#28112,#28113,#28114,#28115,#28116,#28117,
#28118,#28119,#28120,#28121,#28122,#28123,#28124,#28125,#28126,#28127,#28128,
#28129,#28130),.UNSPECIFIED.,.F.,.F.,(4,3,3,3,3,3,3,3,3,3,3,3,3,4),(82.7962910025506,
83.1801699919252,83.6782548421763,84.1763396924274,84.6744245426784,85.1725093929295,
85.6705942431805,86.1686790934316,86.6667639436826,87.1648487939337,87.6629336441847,
88.1610184944358,88.6591033446868,89.0794763097302),.UNSPECIFIED.);
#5971=B_SPLINE_CURVE_WITH_KNOTS('',3,(#28136,#28137,#28138,#28139,#28140,
#28141,#28142,#28143,#28144),.UNSPECIFIED.,.F.,.F.,(4,1,1,1,1,1,4),(103.672557568463,
103.760427844368,104.258512694619,104.75659754487,105.254682395122,105.752767245373,
106.176669420977),.UNSPECIFIED.);
#5972=B_SPLINE_CURVE_WITH_KNOTS('',3,(#28147,#28148,#28149,#28150,#28151,
#28152),.UNSPECIFIED.,.F.,.F.,(4,1,1,4),(103.672557568463,103.942187199755,
104.440272050006,104.938356900257),.UNSPECIFIED.);
#5973=B_SPLINE_CURVE_WITH_KNOTS('',3,(#28157,#28158,#28159,#28160,#28161,
#28162,#28163,#28164,#28165,#28166,#28167,#28168,#28169,#28170,#28171,#28172),
 .UNSPECIFIED.,.F.,.F.,(4,1,1,1,1,1,1,1,1,1,1,1,1,4),(97.3893722612836,
97.7834096413558,98.2814944916068,98.7795793418579,99.2776641921089,99.77574904236,
100.273833892611,100.771918742862,101.270003593113,101.768088443364,102.266173293615,
102.764258143866,103.262342994117,103.672557568463),.UNSPECIFIED.);
#5974=B_SPLINE_CURVE_WITH_KNOTS('',3,(#28173,#28174,#28175,#28176,#28177,
#28178,#28179,#28180,#28181,#28182,#28183,#28184,#28185,#28186,#28187,#28188,
#28189),.UNSPECIFIED.,.F.,.F.,(4,1,1,1,1,1,1,1,1,1,1,1,1,1,4),(97.3893722612835,
97.4670841464912,97.9651689967422,98.4632538469933,98.9613386972443,99.4594235474954,
99.9575083977464,100.455593247997,100.953678098249,101.4517629485,101.949847798751,
102.447932649002,102.946017499253,103.444102349504,103.672557568463),
 .UNSPECIFIED.);
#5975=B_SPLINE_CURVE_WITH_KNOTS('',3,(#28194,#28195,#28196,#28197,#28198,
#28199,#28200,#28201,#28202,#28203,#28204,#28205,#28206,#28207,#28208,#28209,
#28210),.UNSPECIFIED.,.F.,.F.,(4,1,1,1,1,1,1,1,1,1,1,1,1,1,4),(91.106186954104,
91.3083065880921,91.8063914383432,92.3044762885942,92.8025611388453,93.3006459890963,
93.7987308393474,94.2968156895984,94.7949005398495,95.2929853901005,95.7910702403516,
96.2891550906026,96.7872399408537,97.2853247911047,97.3893722612836),
 .UNSPECIFIED.);
#5976=B_SPLINE_CURVE_WITH_KNOTS('',3,(#28211,#28212,#28213,#28214,#28215,
#28216,#28217,#28218,#28219,#28220,#28221,#28222,#28223,#28224,#28225,#28226),
 .UNSPECIFIED.,.F.,.F.,(4,1,1,1,1,1,1,1,1,1,1,1,1,4),(91.106186954104,91.4900659434786,
91.9881507937296,92.4862356439807,92.9843204942317,93.4824053444828,93.9804901947338,
94.4785750449849,94.9766598952359,95.474744745487,95.972829595738,96.4709144459891,
96.9689992962401,97.3893722612835),.UNSPECIFIED.);
#5977=B_SPLINE_CURVE_WITH_KNOTS('',3,(#28231,#28232,#28233,#28234,#28235,
#28236,#28237,#28238,#28239,#28240,#28241,#28242,#28243,#28244,#28245,#28246,
#28247),.UNSPECIFIED.,.F.,.F.,(4,1,1,1,1,1,1,1,1,1,1,1,1,1,4),(84.8230016469244,
84.8332035348285,85.3312883850795,85.8293732353306,86.3274580855816,86.8255429358327,
87.3236277860837,87.8217126363348,88.3197974865858,88.8178823368369,89.3159671870879,
89.814052037339,90.31213688759,90.8102217378411,91.106186954104),
 .UNSPECIFIED.);
#5978=B_SPLINE_CURVE_WITH_KNOTS('',3,(#28248,#28249,#28250,#28251,#28252,
#28253,#28254,#28255,#28256,#28257,#28258,#28259,#28260,#28261,#28262,#28263,
#28264),.UNSPECIFIED.,.F.,.F.,(4,1,1,1,1,1,1,1,1,1,1,1,1,1,4),(84.8230016469244,
85.0149628902149,85.513047740466,86.011132590717,86.5092174409681,87.0073022912191,
87.5053871414702,88.0034719917212,88.5015568419723,88.9996416922233,89.4977265424744,
89.9958113927254,90.4938962429765,90.9919810932275,91.106186954104),
 .UNSPECIFIED.);
#5979=B_SPLINE_CURVE_WITH_KNOTS('',3,(#28269,#28270,#28271,#28272,#28273,
#28274,#28275,#28276,#28277,#28278,#28279,#28280,#28281,#28282,#28283,#28284),
 .UNSPECIFIED.,.F.,.F.,(4,1,1,1,1,1,1,1,1,1,1,1,1,4),(78.5398163397448,
78.8561853318159,79.3542701820669,79.852355032318,80.350439882569,80.8485247328201,
81.3466095830711,81.8446944333222,82.3427792835732,82.8408641338243,83.3389489840753,
83.8370338343264,84.3351186845774,84.8230016469244),.UNSPECIFIED.);
#5980=B_SPLINE_CURVE_WITH_KNOTS('',3,(#28285,#28286,#28287,#28288,#28289,
#28290,#28291,#28292,#28293,#28294,#28295,#28296,#28297,#28298,#28299,#28300,
#28301),.UNSPECIFIED.,.F.,.F.,(4,1,1,1,1,1,1,1,1,1,1,1,1,1,4),(78.5398163397448,
78.5398598369513,79.0379446872024,79.5360295374534,80.0341143877044,80.5321992379555,
81.0302840882066,81.5283689384576,82.0264537887087,82.5245386389597,83.0226234892107,
83.5207083394618,84.0187931897129,84.5168780399639,84.8230016469244),
 .UNSPECIFIED.);
#5981=B_SPLINE_CURVE_WITH_KNOTS('',3,(#28306,#28307,#28308,#28309,#28310,
#28311,#28312,#28313,#28314,#28315,#28316,#28317,#28318,#28319,#28320,#28321,
#28322),.UNSPECIFIED.,.F.,.F.,(4,1,1,1,1,1,1,1,1,1,1,1,1,1,4),(72.2566310325652,
72.3810822785522,72.8791671288033,73.3772519790543,73.8753368293054,74.3734216795564,
74.8715065298075,75.3695913800585,75.8676762303096,76.3657610805606,76.8638459308117,
77.3619307810627,77.8600156313138,78.3581004815648,78.5398163397448),
 .UNSPECIFIED.);
#5982=B_SPLINE_CURVE_WITH_KNOTS('',3,(#28323,#28324,#28325,#28326,#28327,
#28328,#28329,#28330,#28331,#28332,#28333,#28334,#28335,#28336,#28337,#28338),
 .UNSPECIFIED.,.F.,.F.,(4,1,1,1,1,1,1,1,1,1,1,1,1,4),(72.2566310325652,
72.5628416339387,73.0609264841898,73.5590113344408,74.0570961846919,74.5551810349429,
75.053265885194,75.551350735445,76.0494355856961,76.5475204359471,77.0456052861982,
77.5436901364492,78.0417749867003,78.5398163397448),.UNSPECIFIED.);
#5983=B_SPLINE_CURVE_WITH_KNOTS('',3,(#28343,#28344,#28345,#28346,#28347,
#28348,#28349,#28350,#28351,#28352,#28353,#28354,#28355,#28356,#28357,#28358),
 .UNSPECIFIED.,.F.,.F.,(4,1,1,1,1,1,1,1,1,1,1,1,1,4),(65.9734457253856,
66.4040640755397,66.9021489257907,67.4002337760417,67.8983186262928,68.3964034765438,
68.8944883267949,69.3925731770459,69.890658027297,70.388742877548,70.8868277277991,
71.3849125780501,71.8829974283012,72.2566310325652),.UNSPECIFIED.);
#5984=B_SPLINE_CURVE_WITH_KNOTS('',3,(#28359,#28360,#28361,#28362,#28363,
#28364,#28365,#28366,#28367,#28368,#28369,#28370,#28371,#28372,#28373,#28374,
#28375),.UNSPECIFIED.,.F.,.F.,(4,1,1,1,1,1,1,1,1,1,1,1,1,1,4),(65.9734457253856,
66.0877385806751,66.5858234309261,67.0839082811772,67.5819931314282,68.0800779816793,
68.5781628319303,69.0762476821814,69.5743325324324,70.0724173826835,70.5705022329345,
71.0685870831856,71.5666719334366,72.0647567836877,72.2566310325652),
 .UNSPECIFIED.);
#5985=B_SPLINE_CURVE_WITH_KNOTS('',3,(#28380,#28381,#28382,#28383,#28384,
#28385,#28386,#28387,#28388,#28389,#28390,#28391,#28392,#28393,#28394),
 .UNSPECIFIED.,.F.,.F.,(4,1,1,1,1,1,1,1,1,1,1,1,4),(59.690260418206,60.427045872527,
61.4232155730292,61.9213004232802,62.4193852735312,62.9174701237823,63.4155549740333,
63.9136398242844,64.4117246745354,64.9098095247865,65.4078943750375,65.9059792252886,
65.9734457253856),.UNSPECIFIED.);
#5986=B_SPLINE_CURVE_WITH_KNOTS('',3,(#28395,#28396,#28397,#28398,#28399,
#28400,#28401,#28402,#28403,#28404,#28405,#28406,#28407,#28408,#28409,#28410),
 .UNSPECIFIED.,.F.,.F.,(4,1,1,1,1,1,1,1,1,1,1,1,1,4),(59.690260418206,60.1107203776625,
60.6088052279135,61.1068900781646,61.6049749284156,62.1030597786667,62.6011446289177,
63.0992294791688,63.5973143294198,64.0953991796709,64.5934840299219,65.091568880173,
65.589653730424,65.9734457253856),.UNSPECIFIED.);
#5987=B_SPLINE_CURVE_WITH_KNOTS('',3,(#28415,#28416,#28417,#28418,#28419,
#28420,#28421,#28422,#28423,#28424,#28425,#28426,#28427,#28428,#28429,#28430),
 .UNSPECIFIED.,.F.,.F.,(4,1,1,1,1,1,1,1,1,1,1,1,1,4),(53.4070751110264,
53.4538579690124,53.9519428192634,54.4500276695145,54.9481125197655,55.4461973700166,
55.9442822202676,56.4423670705187,56.9404519207697,57.4385367710208,57.9366216212718,
58.4347064715229,59.430876172025,59.690260418206),.UNSPECIFIED.);
#5988=B_SPLINE_CURVE_WITH_KNOTS('',3,(#28431,#28432,#28433,#28434,#28435,
#28436,#28437,#28438,#28439,#28440,#28441,#28442,#28443,#28444),
 .UNSPECIFIED.,.F.,.F.,(4,1,1,1,1,1,1,1,1,1,1,4),(53.4070751110264,53.6356173243988,
54.1337021746499,54.6317870249009,55.129871875152,56.1260415756541,57.1222112761562,
58.1183809766583,58.6164658269093,59.1145506771604,59.6126355274114,59.690260418206),
 .UNSPECIFIED.);
#5989=B_SPLINE_CURVE_WITH_KNOTS('',3,(#28449,#28450,#28451,#28452,#28453,
#28454,#28455,#28456,#28457,#28458,#28459,#28460,#28461,#28462,#28463,#28464),
 .UNSPECIFIED.,.F.,.F.,(4,1,1,1,1,1,1,1,1,1,1,1,1,4),(47.1238898038469,
47.4768397659998,47.9749246162508,48.4730094665019,48.9710943167529,49.469179167004,
49.967264017255,50.4653488675061,50.9634337177571,51.4615185680082,51.9596034182592,
52.4576882685103,52.9557731187613,53.4070751110264),.UNSPECIFIED.);
#5990=B_SPLINE_CURVE_WITH_KNOTS('',3,(#28465,#28466,#28467,#28468,#28469,
#28470,#28471,#28472,#28473,#28474,#28475,#28476,#28477,#28478,#28479,#28480,
#28481),.UNSPECIFIED.,.F.,.F.,(4,1,1,1,1,1,1,1,1,1,1,1,1,1,4),(47.1238898038468,
47.1605142711352,47.6585991213862,48.1566839716373,48.6547688218883,49.1528536721394,
49.6509385223904,50.1490233726415,50.6471082228925,51.1451930731436,51.6432779233946,
52.1413627736457,52.6394476238967,53.1375324741478,53.4070751110264),
 .UNSPECIFIED.);
#5991=B_SPLINE_CURVE_WITH_KNOTS('',3,(#28486,#28487,#28488,#28489,#28490,
#28491,#28492,#28493,#28494,#28495,#28496,#28497,#28498,#28499,#28500,#28501,
#28502),.UNSPECIFIED.,.F.,.F.,(4,1,1,1,1,1,1,1,1,1,1,1,1,1,4),(40.8407044966673,
41.0017367127361,41.4998215629872,41.9979064132382,42.4959912634893,42.9940761137403,
43.4921609639914,43.9902458142424,44.4883306644935,44.9864155147445,45.4845003649956,
45.9825852152466,46.4806700654977,46.9787549157487,47.1238898038469),
 .UNSPECIFIED.);
#5992=B_SPLINE_CURVE_WITH_KNOTS('',3,(#28503,#28504,#28505,#28506,#28507,
#28508,#28509,#28510,#28511,#28512,#28513,#28514,#28515,#28516,#28517,#28518),
 .UNSPECIFIED.,.F.,.F.,(4,1,1,1,1,1,1,1,1,1,1,1,1,4),(40.8407044966672,
41.1834960681226,41.6815809183737,42.1796657686247,42.6777506188757,43.1758354691268,
43.6739203193778,44.1720051696289,44.67009001988,45.168174870131,45.666259720382,
46.1643445706331,46.6624294208841,47.1238898038468),.UNSPECIFIED.);
#5993=B_SPLINE_CURVE_WITH_KNOTS('',3,(#28523,#28524,#28525,#28526,#28527,
#28528,#28529,#28530,#28531,#28532,#28533,#28534,#28535,#28536,#28537,#28538),
 .UNSPECIFIED.,.F.,.F.,(4,1,1,1,1,1,1,1,1,1,1,1,1,4),(34.5575191894877,
35.0247185097235,35.5228033599746,36.0208882102256,36.5189730604767,37.0170579107277,
37.5151427609788,38.0132276112298,38.5113124614809,39.0093973117319,39.507482161983,
40.005567012234,40.5036518624851,40.8407044966673),.UNSPECIFIED.);
#5994=B_SPLINE_CURVE_WITH_KNOTS('',3,(#28539,#28540,#28541,#28542,#28543,
#28544,#28545,#28546,#28547,#28548,#28549,#28550,#28551,#28552,#28553,#28554,
#28555),.UNSPECIFIED.,.F.,.F.,(4,1,1,1,1,1,1,1,1,1,1,1,1,1,4),(34.5575191894876,
34.708393014859,35.20647786511,35.7045627153611,36.2026475656121,36.7007324158632,
37.1988172661142,37.6969021163653,38.1949869666163,38.6930718168674,39.1911566671184,
39.6892415173695,40.1873263676205,40.6854112178715,40.8407044966672),
 .UNSPECIFIED.);
#5995=B_SPLINE_CURVE_WITH_KNOTS('',3,(#28560,#28561,#28562,#28563,#28564,
#28565,#28566,#28567,#28568,#28569,#28570,#28571,#28572,#28573,#28574,#28575,
#28576),.UNSPECIFIED.,.F.,.F.,(4,1,1,1,1,1,1,1,1,1,1,1,1,1,4),(28.2743338823081,
28.5496154564599,29.0477003067109,29.545785156962,30.043870007213,30.5419548574641,
31.0400397077151,31.5381245579662,32.0362094082172,32.5342942584683,33.0323791087193,
33.5304639589704,34.0285488092214,34.5266336594725,34.5575191894877),
 .UNSPECIFIED.);
#5996=B_SPLINE_CURVE_WITH_KNOTS('',3,(#28577,#28578,#28579,#28580,#28581,
#28582,#28583,#28584,#28585,#28586,#28587,#28588,#28589,#28590,#28591,#28592),
 .UNSPECIFIED.,.F.,.F.,(4,1,1,1,1,1,1,1,1,1,1,1,1,4),(28.2743338823081,
28.7313748118464,29.2294596620974,29.7275445123485,30.2256293625995,30.7237142128506,
31.2217990631016,31.7198839133527,32.2179687636037,32.7160536138548,33.2141384641058,
33.7122233143569,34.2103081646079,34.5575191894876),.UNSPECIFIED.);
#5997=B_SPLINE_CURVE_WITH_KNOTS('',3,(#28597,#28598,#28599,#28600,#28601,
#28602,#28603,#28604,#28605,#28606,#28607,#28608,#28609,#28610,#28611,#28612,
#28613),.UNSPECIFIED.,.F.,.F.,(4,1,1,1,1,1,1,1,1,1,1,1,1,1,4),(21.9911485751285,
22.0745124031962,22.5725972534473,23.0706821036983,23.5687669539494,24.0668518042004,
24.5649366544515,25.0630215047025,25.5611063549536,26.0591912052046,26.5572760554557,
27.0553609057067,27.5534457559578,28.0515306062088,28.2743338823081),
 .UNSPECIFIED.);
#5998=B_SPLINE_CURVE_WITH_KNOTS('',3,(#28614,#28615,#28616,#28617,#28618,
#28619,#28620,#28621,#28622,#28623,#28624,#28625,#28626,#28627,#28628,#28629,
#28630),.UNSPECIFIED.,.F.,.F.,(4,1,1,1,1,1,1,1,1,1,1,1,1,1,4),(21.9911485751285,
22.2562717585827,22.7543566088338,23.2524414590848,23.7505263093359,24.2486111595869,
24.746696009838,25.244780860089,25.7428657103401,26.2409505605911,26.7390354108422,
27.2371202610932,27.7352051113443,28.2332899615953,28.2743338823081),
 .UNSPECIFIED.);
#5999=B_SPLINE_CURVE_WITH_KNOTS('',3,(#28635,#28636,#28637,#28638,#28639,
#28640,#28641,#28642,#28643,#28644,#28645,#28646,#28647,#28648,#28649,#28650),
 .UNSPECIFIED.,.F.,.F.,(4,1,1,1,1,1,1,1,1,1,1,1,1,4),(15.7079632679489,
16.0974942001837,16.5955790504347,17.0936639006858,17.5917487509368,18.0898336011878,
18.5879184514389,19.0860033016899,19.584088151941,20.082173002192,20.5802578524431,
21.0783427026941,21.5764275529452,21.9911485751285),.UNSPECIFIED.);
#6000=B_SPLINE_CURVE_WITH_KNOTS('',3,(#28651,#28652,#28653,#28654,#28655,
#28656,#28657,#28658,#28659,#28660,#28661,#28662,#28663,#28664,#28665,#28666,
#28667),.UNSPECIFIED.,.F.,.F.,(4,1,1,1,1,1,1,1,1,1,1,1,1,1,4),(15.7079632679489,
15.7811687053191,16.2792535555701,16.7773384058212,17.2754232560722,17.7735081063233,
18.2715929565743,18.7696778068254,19.2677626570764,19.7658475073275,20.2639323575785,
20.7620172078296,21.2601020580806,21.7581869083317,21.9911485751285),
 .UNSPECIFIED.);
#6001=B_SPLINE_CURVE_WITH_KNOTS('',3,(#28670,#28671,#28672,#28673,#28674,
#28675,#28676,#28677,#28678,#28679,#28680,#28681,#28682,#28683,#28684,#28685,
#28686,#28687,#28688,#28689,#28690,#28691,#28692,#28693,#28694,#28695,#28696,
#28697,#28698,#28699,#28700,#28701,#28702,#28703,#28704,#28705,#28706,#28707,
#28708,#28709,#28710,#28711,#28712,#28713,#28714,#28715,#28716,#28717,#28718,
#28719,#28720,#28721,#28722,#28723,#28724,#28725,#28726,#28727,#28728,#28729,
#28730,#28731,#28732,#28733,#28734,#28735,#28736,#28737,#28738,#28739,#28740,
#28741,#28742,#28743,#28744,#28745,#28746,#28747,#28748,#28749,#28750,#28751,
#28752,#28753,#28754,#28755,#28756,#28757,#28758,#28759,#28760,#28761,#28762,
#28763,#28764,#28765,#28766,#28767,#28768,#28769,#28770,#28771,#28772,#28773,
#28774,#28775,#28776,#28777,#28778,#28779,#28780,#28781),.UNSPECIFIED.,
 .F.,.F.,(4,3,3,3,3,3,3,3,3,3,3,3,3,3,3,3,3,3,3,3,3,3,3,3,3,3,3,3,3,3,3,
3,3,3,3,3,3,4),(-0.937740963081762,-0.907140654471692,-0.869270994512239,
-0.847580464190145,-0.836481370332155,-0.829351939903567,-0.823129304558617,
-0.784196549339193,-0.745021726803261,-0.731277450917006,-0.71832202012087,
-0.712280445222016,-0.695746751935488,-0.656667790671875,-0.616960744636697,
-0.581187597295744,-0.55435773679003,-0.548462240506954,-0.542574359443091,
-0.501604130349,-0.473868155272887,-0.433137517704096,-0.392064137358273,
-0.380617560497555,-0.373704777408693,-0.367641533845849,-0.325920769696254,
-0.283682092026838,-0.241892561201202,-0.211655991051052,-0.198277640892043,
-0.190678095127374,-0.184988742540942,-0.142742067998012,-0.0995960223031999,
-0.0562915317555258,-0.0133559795731416,0.),.UNSPECIFIED.);
#6002=B_SPLINE_CURVE_WITH_KNOTS('',3,(#28786,#28787,#28788,#28789,#28790,
#28791,#28792,#28793,#28794,#28795,#28796,#28797,#28798,#28799,#28800,#28801,
#28802,#28803,#28804,#28805,#28806,#28807,#28808,#28809,#28810,#28811,#28812,
#28813,#28814,#28815,#28816,#28817,#28818,#28819,#28820,#28821,#28822,#28823,
#28824,#28825,#28826,#28827,#28828,#28829,#28830,#28831,#28832,#28833,#28834,
#28835,#28836,#28837,#28838,#28839,#28840,#28841,#28842,#28843,#28844,#28845,
#28846,#28847,#28848,#28849,#28850,#28851,#28852,#28853,#28854,#28855,#28856,
#28857,#28858,#28859,#28860,#28861,#28862,#28863,#28864,#28865,#28866,#28867,
#28868,#28869,#28870,#28871,#28872,#28873,#28874,#28875,#28876,#28877,#28878,
#28879,#28880,#28881,#28882,#28883,#28884,#28885,#28886,#28887,#28888,#28889,
#28890,#28891,#28892,#28893,#28894),.UNSPECIFIED.,.F.,.F.,(4,3,3,3,3,3,
3,3,3,3,3,3,3,3,3,3,3,3,3,3,3,3,3,3,3,3,3,3,3,3,3,3,3,3,3,3,4),(-0.933975894023124,
-0.897518245917797,-0.85418730917007,-0.828760118608177,-0.810932623488333,
-0.801688081435698,-0.75915821677069,-0.716968557512012,-0.68769245742961,
-0.681621420340466,-0.675695062647656,-0.658416357347208,-0.61685703941993,
-0.575176630920201,-0.534137469845906,-0.507834227956848,-0.502068244191955,
-0.496724770966358,-0.456296287597963,-0.428924502289673,-0.388319492614483,
-0.348042200526848,-0.337185447634125,-0.330206209215421,-0.324918360767453,
-0.285434308044378,-0.246386225108482,-0.209399208416579,-0.183224307364507,
-0.169375884861305,-0.161952755019649,-0.156778294147562,-0.117583720610671,
-0.0792968209528158,-0.0396484104764079,-0.00263560956954647,0.),
 .UNSPECIFIED.);
#6003=B_SPLINE_CURVE_WITH_KNOTS('',3,(#29671,#29672,#29673,#29674,#29675,
#29676,#29677,#29678,#29679,#29680,#29681,#29682,#29683,#29684,#29685,#29686,
#29687,#29688,#29689,#29690,#29691,#29692,#29693,#29694,#29695,#29696,#29697,
#29698,#29699,#29700,#29701,#29702,#29703,#29704,#29705,#29706,#29707),
 .UNSPECIFIED.,.F.,.F.,(4,3,3,3,3,3,3,3,3,3,3,3,4),(89.0794763097302,89.1571881949378,
89.6552730451889,90.1533578954399,90.651442745691,91.149527595942,91.6476124461931,
92.1456972964441,92.6437821466952,93.1418669969462,93.6399518471973,94.1380366974483,
94.5619388730527),.UNSPECIFIED.);
#6004=B_SPLINE_CURVE_WITH_KNOTS('',3,(#29709,#29710,#29711,#29712,#29713,
#29714,#29715,#29716,#29717,#29718,#29719,#29720,#29721,#29722,#29723,#29724,
#29725,#29726,#29727,#29728,#29729,#29730,#29731,#29732,#29733,#29734,#29735,
#29736,#29737,#29738,#29739,#29740,#29741,#29742,#29743,#29744,#29745,#29746,
#29747,#29748,#29749,#29750,#29751,#29752,#29753,#29754,#29755,#29756,#29757,
#29758,#29759,#29760,#29761,#29762,#29763,#29764,#29765,#29766,#29767,#29768,
#29769,#29770,#29771,#29772,#29773,#29774,#29775,#29776,#29777,#29778,#29779,
#29780,#29781,#29782,#29783,#29784,#29785,#29786,#29787,#29788,#29789,#29790,
#29791,#29792,#29793,#29794,#29795,#29796,#29797,#29798,#29799,#29800,#29801,
#29802,#29803,#29804,#29805,#29806,#29807,#29808,#29809,#29810,#29811,#29812,
#29813,#29814,#29815,#29816,#29817,#29818,#29819,#29820),.UNSPECIFIED.,
 .F.,.F.,(4,3,3,3,3,3,3,3,3,3,3,3,3,3,3,3,3,3,3,3,3,3,3,3,3,3,3,3,3,3,3,
3,3,3,3,3,3,4),(-0.937740963081777,-0.907140654471705,-0.869270990721146,
-0.847580460872939,-0.836481370719858,-0.829351942923115,-0.823129305042622,
-0.784196547851699,-0.745021725430866,-0.731277450252294,-0.718322019189878,
-0.71228044507783,-0.695746751935491,-0.656667795916307,-0.616960751834722,
-0.581187602694266,-0.554357740838925,-0.548462261493557,-0.542574361216013,
-0.501604132790064,-0.4738681552729,-0.43313752173811,-0.392064143224716,
-0.380617571602666,-0.373704828437967,-0.367641520509243,-0.325920760345294,
-0.283682082032713,-0.241892561201202,-0.211655991051052,-0.19827764062779,
-0.190678095304841,-0.184988742699727,-0.142742050577153,-0.0995959952880378,
-0.0562915047899489,-0.0133559696020479,0.),.UNSPECIFIED.);
#6005=B_SPLINE_CURVE_WITH_KNOTS('',3,(#29821,#29822,#29823,#29824,#29825,
#29826,#29827,#29828,#29829,#29830,#29831,#29832,#29833,#29834),
 .UNSPECIFIED.,.F.,.F.,(4,1,1,1,1,1,1,1,1,1,1,4),(10.3764180272042,10.8003202028086,
11.2984050530596,11.7964899033107,12.2945747535617,12.7926596038128,13.2907444540638,
13.7888293043149,14.2869141545659,14.784999004817,15.283083855068,15.7079632679489),
 .UNSPECIFIED.);
#6006=B_SPLINE_CURVE_WITH_KNOTS('',3,(#29838,#29839,#29840,#29841,#29842,
#29843,#29844,#29845,#29846,#29847,#29848,#29849),.UNSPECIFIED.,.F.,.F.,
(4,1,1,1,1,1,1,1,1,4),(11.6147305479242,12.1128153981753,12.6109002484263,
13.1089850986774,13.6070699489284,14.1051547991795,14.6032396494305,15.1013244996816,
15.5994093499326,15.7079632679489),.UNSPECIFIED.);
#6007=B_SPLINE_CURVE_WITH_KNOTS('',3,(#30626,#30627,#30628,#30629,#30630,
#30631,#30632,#30633,#30634,#30635,#30636,#30637,#30638,#30639,#30640,#30641,
#30642,#30643,#30644,#30645,#30646,#30647,#30648,#30649,#30650,#30651,#30652,
#30653,#30654,#30655,#30656,#30657,#30658,#30659,#30660,#30661,#30662,#30663,
#30664,#30665,#30666,#30667,#30668,#30669,#30670,#30671,#30672,#30673,#30674,
#30675,#30676,#30677,#30678,#30679,#30680,#30681,#30682,#30683,#30684,#30685,
#30686,#30687,#30688,#30689,#30690,#30691,#30692,#30693,#30694,#30695,#30696,
#30697,#30698,#30699,#30700,#30701,#30702,#30703,#30704,#30705,#30706,#30707,
#30708,#30709,#30710,#30711,#30712,#30713,#30714,#30715,#30716,#30717,#30718,
#30719,#30720,#30721,#30722,#30723,#30724,#30725,#30726,#30727,#30728,#30729,
#30730,#30731,#30732,#30733,#30734),.UNSPECIFIED.,.F.,.F.,(4,3,3,3,3,3,
3,3,3,3,3,3,3,3,3,3,3,3,3,3,3,3,3,3,3,3,3,3,3,3,3,3,3,3,3,3,4),(-0.93397589402311,
-0.897518245917774,-0.854187309108942,-0.828760118100427,-0.810932622175928,
-0.80168808147928,-0.759158216888781,-0.71696855880315,-0.68769245807517,
-0.681621420864493,-0.67569506273405,-0.65841635734719,-0.616857039876412,
-0.575176628785756,-0.534137456961281,-0.50783421829338,-0.502068149909085,
-0.496724747629148,-0.456296258740099,-0.428924502289679,-0.388319496329734,
-0.348042218766811,-0.337185483602948,-0.330206404188209,-0.324918477526632,
-0.285434428793379,-0.246386363191161,-0.209399208416591,-0.183224307364517,
-0.169375887565707,-0.161952767222463,-0.156778312515109,-0.117583734386332,
-0.0792968228051709,-0.0396484114025855,-0.00263558281026646,0.),
 .UNSPECIFIED.);
#6008=B_SPLINE_CURVE_WITH_KNOTS('',3,(#30735,#30736,#30737,#30738,#30739,
#30740,#30741,#30742,#30743,#30744,#30745,#30746,#30747,#30748,#30749,#30750,
#30751,#30752,#30753,#30754,#30755,#30756,#30757,#30758,#30759,#30760,#30761,
#30762,#30763,#30764,#30765),.UNSPECIFIED.,.F.,.F.,(4,3,3,3,3,3,3,3,3,3,
4),(-96.6284609487036,-96.1303760984525,-95.6322912482015,-95.1342063979505,
-94.6361215476994,-94.1380366974484,-93.6399518471973,-93.1418669969463,
-92.6437821466952,-92.1456972964442,-92.057827020539),.UNSPECIFIED.);
#6009=B_SPLINE_CURVE_WITH_KNOTS('',3,(#31545,#31546,#31547,#31548,#31549,
#31550,#31551,#31552,#31553,#31554,#31555,#31556,#31557,#31558,#31559,#31560,
#31561,#31562,#31563,#31564,#31565,#31566,#31567,#31568,#31569,#31570,#31571,
#31572,#31573,#31574,#31575,#31576,#31577,#31578,#31579,#31580,#31581,#31582,
#31583,#31584,#31585,#31586,#31587,#31588,#31589,#31590,#31591,#31592,#31593,
#31594,#31595,#31596,#31597,#31598,#31599,#31600,#31601,#31602,#31603,#31604,
#31605,#31606,#31607,#31608,#31609,#31610,#31611,#31612,#31613,#31614,#31615,
#31616,#31617,#31618,#31619,#31620,#31621,#31622,#31623,#31624,#31625,#31626,
#31627,#31628,#31629,#31630,#31631,#31632,#31633,#31634,#31635,#31636,#31637,
#31638,#31639,#31640,#31641,#31642,#31643,#31644,#31645,#31646,#31647,#31648,
#31649,#31650,#31651,#31652,#31653),.UNSPECIFIED.,.F.,.F.,(4,3,3,3,3,3,
3,3,3,3,3,3,3,3,3,3,3,3,3,3,3,3,3,3,3,3,3,3,3,3,3,3,3,3,3,3,4),(-0.933975894023072,
-0.897518245917738,-0.854187309124176,-0.828760118193598,-0.810932622421368,
-0.801688081392097,-0.759158216787806,-0.71696855847361,-0.68769245791039,
-0.681621420681061,-0.675695062695478,-0.65841635734717,-0.616857039787599,
-0.57517662920082,-0.534137459479038,-0.507834220181699,-0.50206816750527,
-0.496724751985825,-0.456296264177866,-0.428924502289679,-0.388319495603713,
-0.348042215202905,-0.337185476574032,-0.330206366049313,-0.324918454649377,
-0.285434405134626,-0.246386336138671,-0.209399208416599,-0.183224307364524,
-0.16937588703651,-0.161952764832493,-0.156778308884714,-0.117583731663536,
-0.07929682241449,-0.039648411207245,-0.00263558803031834,0.),
 .UNSPECIFIED.);
#6010=B_SPLINE_CURVE_WITH_KNOTS('',3,(#31654,#31655,#31656,#31657,#31658,
#31659,#31660,#31661,#31662,#31663,#31664,#31665,#31666,#31667,#31668,#31669,
#31670,#31671,#31672,#31673,#31674,#31675,#31676,#31677,#31678,#31679,#31680,
#31681,#31682,#31683,#31684,#31685,#31686,#31687,#31688,#31689,#31690),
 .UNSPECIFIED.,.F.,.F.,(4,3,3,3,3,3,3,3,3,3,3,3,4),(89.0794763097301,89.1571881949378,
89.6552730451889,90.1533578954399,90.651442745691,91.149527595942,91.6476124461931,
92.1456972964441,92.6437821466952,93.1418669969462,93.6399518471973,94.1380366974483,
94.5619388730527),.UNSPECIFIED.);
#6011=B_SPLINE_CURVE_WITH_KNOTS('',3,(#31692,#31693,#31694,#31695,#31696,
#31697,#31698,#31699,#31700,#31701,#31702,#31703,#31704,#31705,#31706,#31707,
#31708,#31709,#31710,#31711,#31712,#31713,#31714,#31715,#31716,#31717,#31718,
#31719,#31720,#31721,#31722,#31723,#31724,#31725,#31726,#31727,#31728,#31729,
#31730,#31731,#31732,#31733,#31734,#31735,#31736,#31737,#31738,#31739,#31740,
#31741,#31742,#31743,#31744,#31745,#31746,#31747,#31748,#31749,#31750,#31751,
#31752,#31753,#31754,#31755,#31756,#31757,#31758,#31759,#31760,#31761,#31762,
#31763,#31764,#31765,#31766,#31767,#31768,#31769,#31770,#31771,#31772,#31773,
#31774,#31775,#31776,#31777,#31778,#31779,#31780,#31781,#31782,#31783,#31784,
#31785,#31786,#31787,#31788,#31789,#31790,#31791,#31792,#31793,#31794,#31795,
#31796,#31797,#31798,#31799,#31800,#31801,#31802,#31803),.UNSPECIFIED.,
 .F.,.F.,(4,3,3,3,3,3,3,3,3,3,3,3,3,3,3,3,3,3,3,3,3,3,3,3,3,3,3,3,3,3,3,
3,3,3,3,3,3,4),(-0.937740963081779,-0.907140654471699,-0.869270993771617,
-0.847580463542101,-0.836481370403699,-0.829351940484709,-0.823129304651435,
-0.784196549047682,-0.745021726528349,-0.731277450780518,-0.718322019931952,
-0.71228044519251,-0.695746751935487,-0.656667791699655,-0.616960746051451,
-0.581187598356812,-0.554357737585833,-0.548462244751326,-0.542574359801447,
-0.501604130842675,-0.473868155272894,-0.43313751849459,-0.392064138499691,
-0.380617562658136,-0.373704787334874,-0.367641531325938,-0.325920767956713,
-0.283682090161745,-0.241892561201193,-0.211655991051044,-0.198277640840565,
-0.190678095160864,-0.184988742533586,-0.142742064539499,-0.0995960169687047,
-0.0562915264308693,-0.0133559775752571,0.),.UNSPECIFIED.);
#6012=B_SPLINE_CURVE_WITH_KNOTS('',3,(#31804,#31805,#31806,#31807,#31808,
#31809,#31810,#31811,#31812,#31813,#31814,#31815,#31816,#31817),
 .UNSPECIFIED.,.F.,.F.,(4,1,1,1,1,1,1,1,1,1,1,4),(10.3764180272042,10.8003202028086,
11.2984050530597,11.7964899033107,12.2945747535618,12.7926596038128,13.2907444540639,
13.7888293043149,14.286914154566,14.784999004817,15.2830838550681,15.7079632679489),
 .UNSPECIFIED.);
#6013=B_SPLINE_CURVE_WITH_KNOTS('',3,(#31823,#31824,#31825,#31826,#31827,
#31828,#31829,#31830,#31831,#31832,#31833,#31834,#31835,#31836,#31837,#31838,
#31839,#31840,#31841,#31842,#31843,#31844,#31845,#31846,#31847,#31848,#31849,
#31850,#31851,#31852,#31853,#31854,#31855,#31856,#31857,#31858,#31859,#31860,
#31861,#31862,#31863,#31864,#31865,#31866,#31867,#31868,#31869,#31870,#31871,
#31872,#31873,#31874,#31875,#31876,#31877,#31878,#31879,#31880,#31881,#31882,
#31883,#31884,#31885,#31886,#31887,#31888,#31889,#31890,#31891,#31892,#31893,
#31894,#31895,#31896,#31897,#31898,#31899,#31900,#31901,#31902,#31903,#31904,
#31905,#31906,#31907,#31908,#31909,#31910,#31911,#31912,#31913,#31914,#31915,
#31916,#31917,#31918,#31919,#31920,#31921,#31922,#31923,#31924,#31925,#31926,
#31927,#31928,#31929,#31930,#31931),.UNSPECIFIED.,.F.,.F.,(4,3,3,3,3,3,
3,3,3,3,3,3,3,3,3,3,3,3,3,3,3,3,3,3,3,3,3,3,3,3,3,3,3,3,3,3,4),(-0.933975894023121,
-0.897518245917767,-0.854187309175765,-0.828760118641236,-0.810932623574739,
-0.801688081325471,-0.759158216653522,-0.716968557323443,-0.687692457335314,
-0.681621420365228,-0.675695062658239,-0.658416357347185,-0.616857039390373,
-0.575176631065956,-0.534137470686732,-0.507834228587468,-0.502068250144193,
-0.496724772439772,-0.456296289429253,-0.428924502289677,-0.388319492373081,
-0.348042199363598,-0.337185445339697,-0.330206196889632,-0.324918353494149,
-0.285434300515691,-0.246386216454576,-0.209399208416591,-0.183224307364517,
-0.169375884685895,-0.161952754236312,-0.156778292889002,-0.117583719666752,
-0.079296820779602,-0.039648410389801,-0.00263561129235572,0.),
 .UNSPECIFIED.);
#6014=B_SPLINE_CURVE_WITH_KNOTS('',3,(#31934,#31935,#31936,#31937,#31938,
#31939,#31940,#31941,#31942,#31943,#31944,#31945),.UNSPECIFIED.,.F.,.F.,
(4,1,1,1,1,1,1,1,1,4),(11.6147305479242,12.1128153981753,12.6109002484263,
13.1089850986774,13.6070699489284,14.1051547991795,14.6032396494305,15.1013244996816,
15.5994093499326,15.7079632679489),.UNSPECIFIED.);
#6015=B_SPLINE_CURVE_WITH_KNOTS('',3,(#32723,#32724,#32725,#32726,#32727,
#32728,#32729,#32730,#32731,#32732,#32733,#32734,#32735,#32736,#32737,#32738,
#32739,#32740,#32741,#32742,#32743,#32744,#32745,#32746,#32747,#32748,#32749,
#32750,#32751,#32752,#32753,#32754,#32755,#32756,#32757,#32758,#32759,#32760,
#32761,#32762,#32763,#32764,#32765,#32766,#32767,#32768,#32769,#32770,#32771,
#32772,#32773,#32774,#32775,#32776,#32777,#32778,#32779,#32780,#32781,#32782,
#32783,#32784,#32785,#32786,#32787,#32788,#32789,#32790,#32791,#32792,#32793,
#32794,#32795,#32796,#32797,#32798,#32799,#32800,#32801,#32802,#32803,#32804,
#32805,#32806,#32807,#32808,#32809,#32810,#32811,#32812,#32813,#32814,#32815,
#32816,#32817,#32818,#32819,#32820,#32821,#32822,#32823,#32824,#32825,#32826,
#32827,#32828,#32829,#32830,#32831,#32832,#32833,#32834),.UNSPECIFIED.,
 .F.,.F.,(4,3,3,3,3,3,3,3,3,3,3,3,3,3,3,3,3,3,3,3,3,3,3,3,3,3,3,3,3,3,3,
3,3,3,3,3,3,4),(-0.93774096308169,-0.907140654471617,-0.869270990472425,
-0.847580460655302,-0.836481370750679,-0.829351942943646,-0.823129305038796,
-0.784196547713336,-0.7450217252948,-0.731277450146466,-0.71832201906501,
-0.712280445054707,-0.695746751935441,-0.656667796256735,-0.616960752300126,
-0.581187603043312,-0.554357741100701,-0.548462262818575,-0.542574361327803,
-0.501604132950922,-0.473868155272869,-0.433137521996099,-0.392064143603576,
-0.380617572320162,-0.373704831737396,-0.367641519570074,-0.325920759661173,
-0.283682081306335,-0.241892561201191,-0.211655991051042,-0.19827764061072,
-0.190678095317729,-0.184988742720608,-0.142742049467821,-0.099595993558808,
-0.0562915030637826,-0.0133559689776526,0.),.UNSPECIFIED.);
#6016=B_SPLINE_CURVE_WITH_KNOTS('',3,(#32835,#32836,#32837,#32838,#32839,
#32840,#32841,#32842,#32843,#32844,#32845,#32846,#32847,#32848,#32849,#32850,
#32851,#32852,#32853,#32854,#32855,#32856,#32857,#32858,#32859,#32860,#32861,
#32862,#32863,#32864,#32865),.UNSPECIFIED.,.F.,.F.,(4,3,3,3,3,3,3,3,3,3,
4),(-96.6284609487036,-96.1303760984525,-95.6322912482015,-95.1342063979505,
-94.6361215476994,-94.1380366974483,-93.6399518471973,-93.1418669969462,
-92.6437821466952,-92.1456972964441,-92.0578270205389),.UNSPECIFIED.);
#6017=B_SPLINE_CURVE_WITH_KNOTS('',3,(#32893,#32894,#32895,#32896,#32897,
#32898,#32899,#32900,#32901,#32902,#32903,#32904,#32905,#32906,#32907,#32908,
#32909,#32910,#32911),.UNSPECIFIED.,.F.,.F.,(4,3,3,3,3,3,4),(-0.174178071089695,
-0.154986673198929,-0.114885588774786,-0.0950808983971497,-0.0541575034664912,
-0.015183211178068,0.),.UNSPECIFIED.);
#6018=B_SPLINE_CURVE_WITH_KNOTS('',3,(#32915,#32916,#32917,#32918,#32919,
#32920,#32921,#32922,#32923,#32924,#32925,#32926,#32927,#32928,#32929,#32930,
#32931,#32932,#32933,#32934,#32935,#32936,#32937,#32938,#32939,#32940,#32941,
#32942,#32943,#32944,#32945),.UNSPECIFIED.,.F.,.F.,(4,3,3,3,3,3,3,3,3,3,
4),(-0.34833302504866,-0.308790232636103,-0.273824003014673,-0.230071300138895,
-0.208094185883636,-0.154986673198912,-0.114885588774754,-0.0950808983971323,
-0.0541600893914876,-0.0151890133852294,0.),.UNSPECIFIED.);
#6019=B_SPLINE_CURVE_WITH_KNOTS('',3,(#32949,#32950,#32951,#32952,#32953,
#32954,#32955,#32956,#32957,#32958,#32959,#32960,#32961,#32962,#32963,#32964,
#32965,#32966,#32967,#32968,#32969,#32970,#32971,#32972,#32973,#32974,#32975,
#32976,#32977,#32978,#32979),.UNSPECIFIED.,.F.,.F.,(4,3,3,3,3,3,3,3,3,3,
4),(-0.348333025048798,-0.308790232635593,-0.273824003014727,-0.230071300139576,
-0.208094185883622,-0.154986673198899,-0.11488558877477,-0.0950808983971356,
-0.0541600893922442,-0.0151890133860279,0.),.UNSPECIFIED.);
#6020=B_SPLINE_CURVE_WITH_KNOTS('',3,(#32983,#32984,#32985,#32986,#32987,
#32988,#32989,#32990,#32991,#32992,#32993,#32994,#32995,#32996,#32997,#32998,
#32999,#33000,#33001,#33002,#33003,#33004,#33005,#33006,#33007,#33008,#33009,
#33010,#33011,#33012,#33013),.UNSPECIFIED.,.F.,.F.,(4,3,3,3,3,3,3,3,3,3,
4),(-0.348333025048671,-0.308960696547653,-0.273824003014609,-0.233470249531217,
-0.208094185883577,-0.154986673198894,-0.109241611791192,-0.0950808983971477,
-0.0540895389701423,-0.0149322342172363,0.),.UNSPECIFIED.);
#6021=B_SPLINE_CURVE_WITH_KNOTS('',3,(#33017,#33018,#33019,#33020,#33021,
#33022,#33023,#33024,#33025,#33026,#33027,#33028,#33029,#33030,#33031,#33032,
#33033,#33034,#33035,#33036,#33037,#33038,#33039,#33040,#33041,#33042,#33043,
#33044,#33045,#33046,#33047),.UNSPECIFIED.,.F.,.F.,(4,3,3,3,3,3,3,3,3,3,
4),(-0.348333025048856,-0.308790232636422,-0.273824003014757,-0.230071300137989,
-0.208094185883696,-0.154986673198961,-0.114885588774838,-0.0950808983971696,
-0.0541600893923865,-0.0151890133862364,0.),.UNSPECIFIED.);
#6022=B_SPLINE_CURVE_WITH_KNOTS('',3,(#33051,#33052,#33053,#33054,#33055,
#33056,#33057,#33058,#33059,#33060,#33061,#33062,#33063,#33064,#33065,#33066,
#33067,#33068,#33069,#33070,#33071,#33072,#33073,#33074,#33075,#33076,#33077,
#33078,#33079,#33080,#33081),.UNSPECIFIED.,.F.,.F.,(4,3,3,3,3,3,3,3,3,3,
4),(-0.348333025048835,-0.308963919628448,-0.273824003014722,-0.233470249531327,
-0.208094185883678,-0.154986673198948,-0.10923981221781,-0.0950808983971581,
-0.0540902649808351,-0.0149340303411883,0.),.UNSPECIFIED.);
#6023=B_SPLINE_CURVE_WITH_KNOTS('',3,(#33084,#33085,#33086,#33087,#33088,
#33089,#33090,#33091,#33092,#33093,#33094,#33095,#33096,#33097,#33098,#33099),
 .UNSPECIFIED.,.F.,.F.,(4,3,3,3,3,4),(-0.348333025048838,-0.308789249901995,
-0.273824003014767,-0.230071618690294,-0.208094185883669,-0.174178071089695),
 .UNSPECIFIED.);
#6024=B_SPLINE_CURVE_WITH_KNOTS('',3,(#33121,#33122,#33123,#33124),
 .UNSPECIFIED.,.F.,.F.,(4,4),(0.849509741836718,1.12995138480819),
 .UNSPECIFIED.);
#6025=B_SPLINE_CURVE_WITH_KNOTS('',3,(#33126,#33127,#33128,#33129,#33130,
#33131),.UNSPECIFIED.,.F.,.F.,(4,2,4),(-0.0577179767645,-0.0288553777371,
0.),.UNSPECIFIED.);
#6026=B_SPLINE_CURVE_WITH_KNOTS('',3,(#33133,#33134,#33135,#33136,#33137),
 .UNSPECIFIED.,.F.,.F.,(4,1,4),(-1.12682976866335,-0.583467062619184,-0.176725437122352),
 .UNSPECIFIED.);
#6027=B_SPLINE_CURVE_WITH_KNOTS('',3,(#33139,#33140,#33141,#33142,#33143,
#33144),.UNSPECIFIED.,.F.,.F.,(4,2,4),(-0.0577179733807837,-0.0288622045317409,
0.),.UNSPECIFIED.);
#6028=B_SPLINE_CURVE_WITH_KNOTS('',3,(#33145,#33146,#33147,#33148),
 .UNSPECIFIED.,.F.,.F.,(4,4),(0.173603820977428,0.454045463948879),
 .UNSPECIFIED.);
#6029=B_SPLINE_CURVE_WITH_KNOTS('',3,(#33170,#33171,#33172,#33173),
 .UNSPECIFIED.,.F.,.F.,(4,4),(0.84950974183672,1.12995138480819),
 .UNSPECIFIED.);
#6030=B_SPLINE_CURVE_WITH_KNOTS('',3,(#33175,#33176,#33177,#33178,#33179,
#33180),.UNSPECIFIED.,.F.,.F.,(4,2,4),(-0.0577179767754509,-0.0288553777398763,
0.),.UNSPECIFIED.);
#6031=B_SPLINE_CURVE_WITH_KNOTS('',3,(#33182,#33183,#33184,#33185,#33186),
 .UNSPECIFIED.,.F.,.F.,(4,1,4),(-1.12682976866335,-0.720088143166436,-0.176725437122352),
 .UNSPECIFIED.);
#6032=B_SPLINE_CURVE_WITH_KNOTS('',3,(#33187,#33188,#33189,#33190,#33191,
#33192),.UNSPECIFIED.,.F.,.F.,(4,2,4),(-0.0577179733846878,-0.0288622045324974,
0.),.UNSPECIFIED.);
#6033=B_SPLINE_CURVE_WITH_KNOTS('',3,(#33193,#33194,#33195,#33196),
 .UNSPECIFIED.,.F.,.F.,(4,4),(0.173603820977427,0.454045463948881),
 .UNSPECIFIED.);
#6034=B_SPLINE_CURVE_WITH_KNOTS('',3,(#33199,#33200,#33201,#33202),
 .UNSPECIFIED.,.F.,.F.,(4,4),(0.173603820977428,0.454045463948881),
 .UNSPECIFIED.);
#6035=B_SPLINE_CURVE_WITH_KNOTS('',3,(#33205,#33206,#33207,#33208),
 .UNSPECIFIED.,.F.,.F.,(4,4),(0.173603820977428,0.45404546394888),
 .UNSPECIFIED.);
#6036=B_SPLINE_CURVE_WITH_KNOTS('',3,(#33209,#33210,#33211,#33212),
 .UNSPECIFIED.,.F.,.F.,(4,4),(0.84950974183672,1.12995138480819),
 .UNSPECIFIED.);
#6037=B_SPLINE_CURVE_WITH_KNOTS('',3,(#33215,#33216,#33217,#33218),
 .UNSPECIFIED.,.F.,.F.,(4,4),(0.173603820977428,0.454045463948881),
 .UNSPECIFIED.);
#6038=B_SPLINE_CURVE_WITH_KNOTS('',3,(#33219,#33220,#33221,#33222),
 .UNSPECIFIED.,.F.,.F.,(4,4),(0.849509741836719,1.12995138480819),
 .UNSPECIFIED.);
#6039=B_SPLINE_CURVE_WITH_KNOTS('',3,(#33225,#33226,#33227,#33228),
 .UNSPECIFIED.,.F.,.F.,(4,4),(0.173603820977427,0.45404546394888),
 .UNSPECIFIED.);
#6040=B_SPLINE_CURVE_WITH_KNOTS('',3,(#33229,#33230,#33231,#33232),
 .UNSPECIFIED.,.F.,.F.,(4,4),(0.849509741836718,1.12995138480819),
 .UNSPECIFIED.);
#6041=B_SPLINE_CURVE_WITH_KNOTS('',3,(#33234,#33235,#33236,#33237),
 .UNSPECIFIED.,.F.,.F.,(4,4),(0.849509741836719,1.12995138480819),
 .UNSPECIFIED.);
#6042=B_SPLINE_CURVE_WITH_KNOTS('',3,(#33259,#33260,#33261,#33262,#33263,
#33264),.UNSPECIFIED.,.F.,.F.,(4,2,4),(-0.0577179767668117,-0.0288553777377456,
0.),.UNSPECIFIED.);
#6043=B_SPLINE_CURVE_WITH_KNOTS('',3,(#33266,#33267,#33268,#33269,#33270),
 .UNSPECIFIED.,.F.,.F.,(4,1,4),(-1.12682976866335,-0.583467062619184,-0.176725437122352),
 .UNSPECIFIED.);
#6044=B_SPLINE_CURVE_WITH_KNOTS('',3,(#33271,#33272,#33273,#33274,#33275,
#33276),.UNSPECIFIED.,.F.,.F.,(4,2,4),(-0.0577179733828224,-0.0288622045316709,
0.),.UNSPECIFIED.);
#6045=B_SPLINE_CURVE_WITH_KNOTS('',3,(#33284,#33285,#33286,#33287,#33288,
#33289),.UNSPECIFIED.,.F.,.F.,(4,2,4),(-0.0577179733841313,-0.0288622045319975,
0.),.UNSPECIFIED.);
#6046=B_SPLINE_CURVE_WITH_KNOTS('',3,(#33295,#33296,#33297,#33298,#33299,
#33300),.UNSPECIFIED.,.F.,.F.,(4,2,4),(-0.0577179767666892,-0.0288553777374165,
0.),.UNSPECIFIED.);
#6047=B_SPLINE_CURVE_WITH_KNOTS('',3,(#33302,#33303,#33304,#33305,#33306,
#33307),.UNSPECIFIED.,.F.,.F.,(4,2,4),(-0.0577179733770289,-0.0288622045288615,
0.),.UNSPECIFIED.);
#6048=B_SPLINE_CURVE_WITH_KNOTS('',3,(#33312,#33313,#33314,#33315,#33316,
#33317),.UNSPECIFIED.,.F.,.F.,(4,2,4),(-0.0577179767699769,-0.0288553777383127,
0.),.UNSPECIFIED.);
#6049=B_SPLINE_CURVE_WITH_KNOTS('',3,(#33320,#33321,#33322,#33323,#33324,
#33325),.UNSPECIFIED.,.F.,.F.,(4,2,4),(-0.0577179767634003,-0.0288553777369938,
0.),.UNSPECIFIED.);
#6050=B_SPLINE_CURVE_WITH_KNOTS('',3,(#33327,#33328,#33329,#33330,#33331,
#33332),.UNSPECIFIED.,.F.,.F.,(4,2,4),(-0.0577179733866089,-0.0288622045330813,
0.),.UNSPECIFIED.);
#6051=B_SPLINE_CURVE_WITH_KNOTS('',3,(#33354,#33355,#33356,#33357,#33358),
 .UNSPECIFIED.,.F.,.F.,(4,1,4),(-1.12682976866335,-0.720088143166436,-0.176725437122352),
 .UNSPECIFIED.);
#6052=B_SPLINE_CURVE_WITH_KNOTS('',3,(#33387,#33388,#33389,#33390,#33391),
 .UNSPECIFIED.,.F.,.F.,(4,1,4),(-1.12682976866335,-0.583467062619184,-0.176725437122352),
 .UNSPECIFIED.);
#6053=B_SPLINE_CURVE_WITH_KNOTS('',3,(#33428,#33429,#33430,#33431,#33432),
 .UNSPECIFIED.,.F.,.F.,(4,1,4),(-1.12682976866335,-0.583467062619184,-0.176725437122352),
 .UNSPECIFIED.);
#6054=B_SPLINE_CURVE_WITH_KNOTS('',3,(#34071,#34072,#34073,#34074,#34075,
#34076,#34077,#34078,#34079,#34080,#34081,#34082,#34083,#34084,#34085,#34086),
 .UNSPECIFIED.,.F.,.F.,(4,3,3,3,3,4),(-4.09299088010938,-3.9996212418776,
-3.4996685866429,-2.9997159314082,-2.4997632761735,-2.07752579179387),
 .UNSPECIFIED.);
#6055=B_SPLINE_CURVE_WITH_KNOTS('',3,(#34089,#34090,#34091,#34092,#34093,
#34094,#34095,#34096,#34097,#34098),.UNSPECIFIED.,.F.,.F.,(4,3,3,4),(0.,
0.4999526552347,0.999905310469399,1.12612756527404),.UNSPECIFIED.);
#6056=B_SPLINE_CURVE_WITH_KNOTS('',3,(#34103,#34104,#34105,#34106,#34107,
#34108,#34109,#34110,#34111,#34112,#34113,#34114,#34115,#34116,#34117,#34118,
#34119,#34120,#34121,#34122,#34123,#34124,#34125,#34126,#34127,#34128,#34129,
#34130,#34131,#34132,#34133,#34134,#34135,#34136,#34137,#34138,#34139,#34140,
#34141,#34142),.UNSPECIFIED.,.F.,.F.,(4,3,3,3,3,3,3,3,3,3,3,3,3,4),(-10.376176187289,
-9.999053104694,-9.4991004494593,-8.9991477942246,-8.4991951389899,-7.9992424837552,
-7.4992898285205,-6.9993371732858,-6.4993845180511,-5.9994318628164,-5.4994792075817,
-4.999526552347,-4.4995738971123,-4.09299088010938),.UNSPECIFIED.);
#6057=B_SPLINE_CURVE_WITH_KNOTS('',3,(#34143,#34144,#34145,#34146,#34147,
#34148,#34149,#34150,#34151,#34152,#34153,#34154,#34155,#34156,#34157,#34158,
#34159,#34160,#34161,#34162,#34163,#34164,#34165,#34166,#34167,#34168,#34169,
#34170,#34171,#34172,#34173,#34174,#34175,#34176,#34177,#34178,#34179,#34180,
#34181,#34182),.UNSPECIFIED.,.F.,.F.,(4,3,3,3,3,3,3,3,3,3,3,3,3,4),(1.12612756527404,
1.4998579657041,1.9998106209388,2.4997632761735,2.9997159314082,3.4996685866429,
3.9996212418776,4.4995738971123,4.999526552347,5.4994792075817,5.9994318628164,
6.4993845180511,6.9993371732858,7.40931287245364),.UNSPECIFIED.);
#6058=B_SPLINE_CURVE_WITH_KNOTS('',3,(#34187,#34188,#34189,#34190,#34191,
#34192,#34193,#34194,#34195,#34196,#34197,#34198,#34199,#34200,#34201,#34202,
#34203,#34204,#34205,#34206,#34207,#34208,#34209,#34210,#34211,#34212,#34213,
#34214,#34215,#34216,#34217,#34218,#34219,#34220,#34221,#34222,#34223,#34224,
#34225,#34226,#34227,#34228,#34229),.UNSPECIFIED.,.F.,.F.,(4,3,3,3,3,3,
3,3,3,3,3,3,3,3,4),(-16.6593614944686,-16.4984376227451,-15.9984849675104,
-15.4985323122757,-14.998579657041,-14.4986270018063,-13.9986743465716,
-13.4987216913369,-12.9987690361022,-12.4988163808675,-11.9988637256328,
-11.4989110703981,-10.9989584151634,-10.4990057599287,-10.376176187289),
 .UNSPECIFIED.);
#6059=B_SPLINE_CURVE_WITH_KNOTS('',3,(#34230,#34231,#34232,#34233,#34234,
#34235,#34236,#34237,#34238,#34239,#34240,#34241,#34242,#34243,#34244,#34245,
#34246,#34247,#34248,#34249,#34250,#34251,#34252,#34253,#34254,#34255,#34256,
#34257,#34258,#34259,#34260,#34261,#34262,#34263,#34264,#34265,#34266,#34267,
#34268,#34269,#34270,#34271,#34272),.UNSPECIFIED.,.F.,.F.,(4,3,3,3,3,3,
3,3,3,3,3,3,3,3,4),(7.40931287245364,7.4992898285205,7.9992424837552,8.4991951389899,
8.9991477942246,9.49910044945929,9.999053104694,10.4990057599287,10.9989584151634,
11.4989110703981,11.9988637256328,12.4988163808675,12.9987690361022,13.4987216913369,
13.6924981796332),.UNSPECIFIED.);
#6060=B_SPLINE_CURVE_WITH_KNOTS('',3,(#34277,#34278,#34279,#34280,#34281,
#34282,#34283,#34284,#34285,#34286,#34287,#34288,#34289,#34290,#34291,#34292,
#34293,#34294,#34295,#34296,#34297,#34298,#34299,#34300,#34301,#34302,#34303,
#34304,#34305,#34306,#34307,#34308,#34309,#34310,#34311,#34312,#34313,#34314,
#34315,#34316),.UNSPECIFIED.,.F.,.F.,(4,3,3,3,3,3,3,3,3,3,3,3,3,4),(-22.9425468016482,
-22.4978694855615,-21.9979168303268,-21.4979641750921,-20.9980115198574,
-20.4980588646227,-19.998106209388,-19.4981535541533,-18.9982008989186,
-18.4982482436839,-17.9982955884492,-17.4983429332145,-16.9983902779798,
-16.6593614944686),.UNSPECIFIED.);
#6061=B_SPLINE_CURVE_WITH_KNOTS('',3,(#34317,#34318,#34319,#34320,#34321,
#34322,#34323,#34324,#34325,#34326,#34327,#34328,#34329,#34330,#34331,#34332,
#34333,#34334,#34335,#34336,#34337,#34338,#34339,#34340,#34341,#34342,#34343,
#34344,#34345,#34346,#34347,#34348,#34349,#34350,#34351,#34352,#34353,#34354,
#34355,#34356),.UNSPECIFIED.,.F.,.F.,(4,3,3,3,3,3,3,3,3,3,3,3,3,4),(13.6924981796332,
13.9986743465716,14.4986270018063,14.998579657041,15.4985323122757,15.9984849675104,
16.4984376227451,16.9983902779798,17.4983429332145,17.9982955884492,18.4982482436839,
18.9982008989186,19.4981535541533,19.9756834868128),.UNSPECIFIED.);
#6062=B_SPLINE_CURVE_WITH_KNOTS('',3,(#34361,#34362,#34363,#34364,#34365,
#34366,#34367,#34368,#34369,#34370,#34371,#34372,#34373,#34374,#34375,#34376,
#34377,#34378,#34379,#34380,#34381,#34382,#34383,#34384,#34385,#34386,#34387,
#34388,#34389,#34390,#34391,#34392,#34393,#34394,#34395,#34396,#34397,#34398,
#34399,#34400,#34401,#34402,#34403),.UNSPECIFIED.,.F.,.F.,(4,3,3,3,3,3,
3,3,3,3,3,3,3,3,4),(-29.2257321088278,-28.9972540036126,-28.4973013483779,
-27.9973486931432,-27.4973960379085,-26.9974433826738,-26.4974907274391,
-25.9975380722044,-25.4975854169697,-24.997632761735,-24.4976801065003,
-23.9977274512656,-23.4977747960309,-22.9978221407962,-22.9425468016482),
 .UNSPECIFIED.);
#6063=B_SPLINE_CURVE_WITH_KNOTS('',3,(#34404,#34405,#34406,#34407,#34408,
#34409,#34410,#34411,#34412,#34413,#34414,#34415,#34416,#34417,#34418,#34419,
#34420,#34421,#34422,#34423,#34424,#34425,#34426,#34427,#34428,#34429,#34430,
#34431,#34432,#34433,#34434,#34435,#34436,#34437,#34438,#34439,#34440,#34441,
#34442,#34443,#34444,#34445,#34446),.UNSPECIFIED.,.F.,.F.,(4,3,3,3,3,3,
3,3,3,3,3,3,3,3,4),(19.9756834868128,19.998106209388,20.4980588646227,20.9980115198574,
21.4979641750921,21.9979168303268,22.4978694855615,22.9978221407962,23.4977747960309,
23.9977274512656,24.4976801065003,24.997632761735,25.4975854169697,25.9975380722044,
26.2588687939924),.UNSPECIFIED.);
#6064=B_SPLINE_CURVE_WITH_KNOTS('',3,(#34451,#34452,#34453,#34454,#34455,
#34456,#34457,#34458,#34459,#34460,#34461,#34462,#34463,#34464,#34465,#34466,
#34467,#34468,#34469,#34470,#34471,#34472,#34473,#34474,#34475,#34476,#34477,
#34478,#34479,#34480,#34481,#34482,#34483,#34484,#34485,#34486,#34487,#34488,
#34489,#34490,#34491,#34492,#34493),.UNSPECIFIED.,.F.,.F.,(4,3,3,3,3,3,
3,3,3,3,3,3,3,3,4),(-35.5089174160073,-35.4966385216637,-34.996685866429,
-34.4967332111943,-33.9967805559596,-33.4968279007249,-32.9968752454902,
-32.4969225902555,-31.9969699350208,-31.4970172797861,-30.9970646245514,
-30.4971119693167,-29.997159314082,-29.4972066588473,-29.2257321088278),
 .UNSPECIFIED.);
#6065=B_SPLINE_CURVE_WITH_KNOTS('',3,(#34494,#34495,#34496,#34497,#34498,
#34499,#34500,#34501,#34502,#34503,#34504,#34505,#34506,#34507,#34508,#34509,
#34510,#34511,#34512,#34513,#34514,#34515,#34516,#34517,#34518,#34519,#34520,
#34521,#34522,#34523,#34524,#34525,#34526,#34527,#34528,#34529,#34530,#34531,
#34532,#34533,#34534,#34535,#34536),.UNSPECIFIED.,.F.,.F.,(4,3,3,3,3,3,
3,3,3,3,3,3,3,3,4),(26.2588687939924,26.4974907274391,26.9974433826738,
27.4973960379085,27.9973486931432,28.4973013483779,28.9972540036126,29.4972066588473,
29.997159314082,30.4971119693167,30.9970646245514,31.4970172797861,31.9969699350208,
32.4969225902555,32.542054101172),.UNSPECIFIED.);
#6066=B_SPLINE_CURVE_WITH_KNOTS('',3,(#34542,#34543,#34544,#34545),
 .UNSPECIFIED.,.F.,.F.,(4,4),(47.1238898038469,47.5338483938829),
 .UNSPECIFIED.);
#6067=B_SPLINE_CURVE_WITH_KNOTS('',3,(#34551,#34552,#34553,#34554,#34555,
#34556,#34557,#34558,#34559,#34560,#34561,#34562,#34563,#34564,#34565,#34566,
#34567),.UNSPECIFIED.,.F.,.F.,(4,1,1,1,1,1,1,1,1,1,1,1,1,1,4),(40.8407044966673,
41.1121790466869,41.6121317019216,42.1120843571563,42.612037012391,43.1119896676257,
43.6119423228604,44.1118949780951,44.6118476333298,45.1118002885645,45.6117529437992,
46.1117055990339,46.6116582542686,47.1116109095033,47.1238898038469),
 .UNSPECIFIED.);
#6068=B_SPLINE_CURVE_WITH_KNOTS('',3,(#34570,#34571,#34572,#34573,#34574,
#34575,#34576,#34577,#34578,#34579,#34580,#34581,#34582,#34583),
 .UNSPECIFIED.,.F.,.F.,(4,1,1,1,1,1,1,1,1,1,1,4),(40.8407044966673,41.2955256409855,
41.7954782962202,42.2954309514549,42.7953836066896,43.2953362619243,43.795288917159,
44.2952415723937,44.7951942276284,45.2951468828631,45.7950995380978,46.2950521933325),
 .UNSPECIFIED.);
#6069=B_SPLINE_CURVE_WITH_KNOTS('',3,(#34588,#34589,#34590,#34591,#34592,
#34593,#34594,#34595,#34596,#34597,#34598,#34599,#34600,#34601,#34602,#34603,
#34604),.UNSPECIFIED.,.F.,.F.,(4,1,1,1,1,1,1,1,1,1,1,1,1,1,4),(34.5575191894877,
34.6127945286358,35.1127471838705,35.6126998391052,36.1126524943399,36.6126051495746,
37.1125578048093,37.612510460044,38.1124631152787,38.6124157705134,39.1123684257481,
39.6123210809828,40.1122737362175,40.6122263914522,40.8407044966673),
 .UNSPECIFIED.);
#6070=B_SPLINE_CURVE_WITH_KNOTS('',3,(#34605,#34606,#34607,#34608,#34609,
#34610,#34611,#34612,#34613,#34614,#34615,#34616,#34617,#34618,#34619,#34620,
#34621),.UNSPECIFIED.,.F.,.F.,(4,1,1,1,1,1,1,1,1,1,1,1,1,1,4),(34.5575191894877,
34.7961411229344,35.2960937781691,35.7960464334038,36.2959990886385,36.7959517438732,
37.2959043991079,37.7958570543426,38.2958097095773,38.795762364812,39.2957150200467,
39.7956676752814,40.2956203305161,40.7955729857508,40.8407044966673),
 .UNSPECIFIED.);
#6071=B_SPLINE_CURVE_WITH_KNOTS('',3,(#34626,#34627,#34628,#34629,#34630,
#34631,#34632,#34633,#34634,#34635,#34636,#34637,#34638,#34639,#34640,#34641),
 .UNSPECIFIED.,.F.,.F.,(4,1,1,1,1,1,1,1,1,1,1,1,1,4),(28.2743338823081,
28.6133626658194,29.1133153210541,29.6132679762888,30.1132206315235,30.6131732867582,
31.1131259419929,31.6130785972276,32.1130312524623,32.612983907697,33.1129365629317,
33.6128892181664,34.1128418734011,34.5575191894877),.UNSPECIFIED.);
#6072=B_SPLINE_CURVE_WITH_KNOTS('',3,(#34642,#34643,#34644,#34645,#34646,
#34647,#34648,#34649,#34650,#34651,#34652,#34653,#34654,#34655,#34656,#34657,
#34658),.UNSPECIFIED.,.F.,.F.,(4,1,1,1,1,1,1,1,1,1,1,1,1,1,4),(28.2743338823082,
28.2967566048833,28.796709260118,29.2966619153527,29.7966145705874,30.2965672258221,
30.7965198810568,31.2964725362915,31.7964251915262,32.2963778467609,32.7963305019956,
33.2962831572303,33.796235812465,34.2961884676997,34.5575191894877),
 .UNSPECIFIED.);
#6073=B_SPLINE_CURVE_WITH_KNOTS('',3,(#34663,#34664,#34665,#34666,#34667,
#34668,#34669,#34670,#34671,#34672,#34673,#34674,#34675,#34676,#34677,#34678,
#34679),.UNSPECIFIED.,.F.,.F.,(4,1,1,1,1,1,1,1,1,1,1,1,1,1,4),(21.9911485751286,
22.1139781477683,22.613930803003,23.1138834582377,23.6138361134724,24.1137887687071,
24.6137414239418,25.1136940791765,25.6136467344112,26.1135993896459,26.6135520448806,
27.1135047001153,27.61345735535,28.1134100105847,28.2743338823081),
 .UNSPECIFIED.);
#6074=B_SPLINE_CURVE_WITH_KNOTS('',3,(#34680,#34681,#34682,#34683,#34684,
#34685,#34686,#34687,#34688,#34689,#34690,#34691,#34692,#34693,#34694,#34695),
 .UNSPECIFIED.,.F.,.F.,(4,1,1,1,1,1,1,1,1,1,1,1,1,4),(21.9911485751286,
22.2973247420669,22.7972773973016,23.2972300525363,23.797182707771,24.2971353630057,
24.7970880182404,25.2970406734751,25.7969933287098,26.2969459839445,26.7968986391792,
27.2968512944139,27.7968039496486,28.2743338823082),.UNSPECIFIED.);
#6075=B_SPLINE_CURVE_WITH_KNOTS('',3,(#34700,#34701,#34702,#34703,#34704,
#34705,#34706,#34707,#34708,#34709,#34710,#34711,#34712,#34713,#34714,#34715),
 .UNSPECIFIED.,.F.,.F.,(4,1,1,1,1,1,1,1,1,1,1,1,1,4),(15.707963267949,16.1145462849519,
16.6144989401866,17.1144515954213,17.614404250656,18.1143569058907,18.6143095611254,
19.1142622163601,19.6142148715948,20.1141675268295,20.6141201820642,21.1140728372989,
21.6140254925336,21.9911485751286),.UNSPECIFIED.);
#6076=B_SPLINE_CURVE_WITH_KNOTS('',3,(#34716,#34717,#34718,#34719,#34720,
#34721,#34722,#34723,#34724,#34725,#34726,#34727,#34728,#34729,#34730,#34731,
#34732),.UNSPECIFIED.,.F.,.F.,(4,1,1,1,1,1,1,1,1,1,1,1,1,1,4),(15.707963267949,
15.7979402240158,16.2978928792505,16.7978455344852,17.2977981897199,17.7977508449546,
18.2977035001893,18.797656155424,19.2976088106587,19.7975614658934,20.2975141211281,
20.7974667763628,21.2974194315975,21.7973720868322,21.9911485751286),
 .UNSPECIFIED.);
#6077=B_SPLINE_CURVE_WITH_KNOTS('',3,(#34749,#34750,#34751,#34752,#34753,
#34754,#34755,#34756,#34757,#34758,#34759,#34760,#34761,#34762,#34763,#34764,
#34765,#34766,#34767,#34768,#34769,#34770,#34771,#34772,#34773,#34774,#34775,
#34776,#34777,#34778,#34779,#34780,#34781,#34782,#34783,#34784,#34785,#34786,
#34787,#34788,#34789,#34790,#34791,#34792,#34793,#34794,#34795,#34796,#34797,
#34798,#34799,#34800,#34801,#34802,#34803,#34804,#34805,#34806,#34807,#34808,
#34809,#34810,#34811,#34812,#34813,#34814,#34815,#34816,#34817,#34818,#34819,
#34820,#34821,#34822,#34823,#34824,#34825,#34826,#34827,#34828,#34829,#34830,
#34831,#34832,#34833,#34834,#34835,#34836,#34837,#34838,#34839,#34840,#34841,
#34842,#34843,#34844,#34845,#34846,#34847,#34848,#34849,#34850,#34851,#34852,
#34853,#34854,#34855,#34856,#34857,#34858,#34859,#34860,#34861,#34862,#34863,
#34864,#34865,#34866,#34867,#34868,#34869,#34870,#34871,#34872,#34873,#34874,
#34875,#34876,#34877,#34878,#34879,#34880,#34881),.UNSPECIFIED.,.F.,.F.,
(4,3,3,3,3,3,3,3,3,3,3,3,3,3,3,3,3,3,3,3,3,3,3,3,3,3,3,3,3,3,3,3,3,3,3,
3,3,3,3,3,3,3,3,3,4),(-2.39439908413783,-2.30957006706654,-2.30182447788038,
-2.21683915448865,-2.13179789072762,-2.10408753243577,-2.08510252693198,
-2.07378115843186,-1.9893556355058,-1.90508589622026,-1.8214508359809,-1.79406927604186,
-1.78088810955347,-1.77088744261425,-1.71192459622473,-1.62862729255915,
-1.54477045309122,-1.46093260268497,-1.37847744264543,-1.3475567576306,
-1.32641194433753,-1.31774824536313,-1.23483340159521,-1.15208726906264,
-1.13111196252681,-1.04809579862442,-0.965185364599438,-0.914579669022902,
-0.892439677208167,-0.877969102190866,-0.870243944296804,-0.788175403641409,
-0.706044208898441,-0.624661556162812,-0.56033979998715,-0.490297324988757,
-0.459653742176959,-0.439904400552519,-0.429071911295872,-0.348385668380925,
-0.267119040059977,-0.186022607101873,-0.105553521737276,-0.0264973312222494,
0.),.UNSPECIFIED.);
#6078=B_SPLINE_CURVE_WITH_KNOTS('',3,(#34884,#34885,#34886,#34887,#34888,
#34889,#34890,#34891,#34892,#34893,#34894,#34895,#34896,#34897,#34898,#34899,
#34900,#34901,#34902,#34903,#34904,#34905,#34906,#34907,#34908,#34909,#34910,
#34911,#34912,#34913,#34914,#34915,#34916,#34917,#34918,#34919,#34920,#34921,
#34922,#34923,#34924,#34925,#34926,#34927,#34928,#34929,#34930,#34931,#34932,
#34933,#34934,#34935,#34936,#34937,#34938,#34939,#34940,#34941,#34942,#34943,
#34944,#34945,#34946,#34947,#34948,#34949,#34950,#34951,#34952,#34953,#34954,
#34955,#34956,#34957,#34958,#34959,#34960,#34961,#34962,#34963,#34964,#34965,
#34966,#34967,#34968,#34969,#34970,#34971,#34972,#34973,#34974,#34975,#34976,
#34977,#34978,#34979,#34980,#34981,#34982,#34983,#34984,#34985,#34986,#34987,
#34988,#34989,#34990,#34991,#34992,#34993,#34994,#34995,#34996,#34997,#34998,
#34999,#35000,#35001,#35002,#35003,#35004,#35005,#35006,#35007,#35008,#35009,
#35010,#35011,#35012,#35013,#35014,#35015,#35016),.UNSPECIFIED.,.F.,.F.,
(4,3,3,3,3,3,3,3,3,3,3,3,3,3,3,3,3,3,3,3,3,3,3,3,3,3,3,3,3,3,3,3,3,3,3,
3,3,3,3,3,3,3,3,3,4),(-2.39814946016211,-2.31696654854078,-2.31176064552941,
-2.2311333678253,-2.15001222659785,-2.12500103373431,-2.11084475967138,
-2.10007493179954,-2.01881508560754,-1.93699475602997,-1.85542103054389,
-1.82902405810322,-1.81445850161468,-1.80514353455762,-1.7498331407812,
-1.66857359850511,-1.58641199849619,-1.50382302505166,-1.42203537088144,
-1.39136500056761,-1.37149659188763,-1.36296522535554,-1.27990647763488,
-1.19645107967923,-1.17667240837077,-1.09362128325192,-1.01021569736535,
-0.958095766843359,-0.935293297239988,-0.920835977756462,-0.912266009922214,
-0.828465696793338,-0.744201354938751,-0.660092638546984,-0.593256253189411,
-0.519099221540735,-0.486655520194439,-0.46739399444203,-0.456346246303998,
-0.372642943242295,-0.287971923540297,-0.202778852160483,-0.117861506263224,
-0.0340642945208537,0.),.UNSPECIFIED.);
#6079=B_SPLINE_CURVE_WITH_KNOTS('',3,(#35086,#35087,#35088,#35089,#35090,
#35091,#35092,#35093,#35094,#35095,#35096,#35097,#35098,#35099,#35100,#35101,
#35102,#35103,#35104,#35105,#35106,#35107,#35108,#35109,#35110,#35111,#35112,
#35113,#35114,#35115,#35116,#35117,#35118,#35119,#35120,#35121,#35122,#35123,
#35124,#35125,#35126,#35127,#35128,#35129,#35130,#35131,#35132,#35133,#35134,
#35135,#35136,#35137,#35138,#35139,#35140,#35141,#35142,#35143,#35144,#35145,
#35146,#35147,#35148,#35149,#35150,#35151,#35152,#35153,#35154,#35155,#35156,
#35157,#35158,#35159,#35160,#35161,#35162,#35163,#35164,#35165,#35166,#35167,
#35168,#35169,#35170,#35171,#35172,#35173,#35174,#35175,#35176,#35177,#35178,
#35179,#35180,#35181,#35182,#35183,#35184,#35185,#35186,#35187,#35188,#35189,
#35190,#35191,#35192,#35193,#35194,#35195,#35196,#35197,#35198,#35199,#35200,
#35201,#35202,#35203,#35204,#35205,#35206,#35207,#35208,#35209,#35210,#35211,
#35212,#35213,#35214,#35215,#35216,#35217,#35218),.UNSPECIFIED.,.F.,.F.,
(4,3,3,3,3,3,3,3,3,3,3,3,3,3,3,3,3,3,3,3,3,3,3,3,3,3,3,3,3,3,3,3,3,3,3,
3,3,3,3,3,3,3,3,3,4),(-2.39814946016209,-2.31696654798685,-2.31176064552942,
-2.23113336581782,-2.15001222437096,-2.1250010316466,-2.11084475490401,
-2.10007493009901,-2.01881508213026,-1.93699475310395,-1.85542102865954,
-1.82902405668996,-1.81445849842888,-1.80514353011277,-1.74983314078119,
-1.66857360092947,-1.58641200157897,-1.50382302878938,-1.42203537368473,
-1.39136500302049,-1.37149659340416,-1.36296522675857,-1.27990647947373,
-1.19645108306756,-1.17667240837078,-1.09362128874921,-1.01021570226622,
-0.958095771131617,-0.935293301260229,-0.92083598151022,-0.912266014498421,
-0.828465707020358,-0.744201365768398,-0.660092636593609,-0.593256253189404,
-0.519099221540729,-0.486655520194433,-0.467393994895198,-0.456346246608538,
-0.372642917004424,-0.287971879301221,-0.202778810971215,-0.117861482515254,
-0.0340643074044279,0.),.UNSPECIFIED.);
#6080=B_SPLINE_CURVE_WITH_KNOTS('',3,(#35223,#35224,#35225,#35226,#35227,
#35228,#35229,#35230,#35231,#35232,#35233,#35234,#35235,#35236,#35237,#35238,
#35239,#35240,#35241,#35242,#35243,#35244,#35245,#35246,#35247,#35248,#35249,
#35250,#35251,#35252,#35253,#35254,#35255,#35256,#35257,#35258,#35259,#35260,
#35261,#35262,#35263,#35264,#35265,#35266,#35267,#35268,#35269,#35270,#35271,
#35272,#35273,#35274,#35275,#35276,#35277,#35278,#35279,#35280,#35281,#35282,
#35283,#35284,#35285,#35286,#35287,#35288,#35289,#35290,#35291,#35292,#35293,
#35294,#35295,#35296,#35297,#35298,#35299,#35300,#35301,#35302,#35303,#35304,
#35305,#35306,#35307,#35308,#35309,#35310,#35311,#35312,#35313,#35314,#35315,
#35316,#35317,#35318,#35319,#35320,#35321,#35322,#35323,#35324,#35325,#35326,
#35327,#35328,#35329,#35330,#35331,#35332,#35333,#35334,#35335,#35336,#35337,
#35338,#35339,#35340,#35341,#35342,#35343,#35344,#35345,#35346,#35347,#35348,
#35349,#35350,#35351,#35352,#35353,#35354,#35355),.UNSPECIFIED.,.F.,.F.,
(4,3,3,3,3,3,3,3,3,3,3,3,3,3,3,3,3,3,3,3,3,3,3,3,3,3,3,3,3,3,3,3,3,3,3,
3,3,3,3,3,3,3,3,3,4),(-2.39439908413779,-2.3095700684437,-2.30182447788042,
-2.21683915479781,-2.1317978905798,-2.10408753251614,-2.08510252752977,
-2.07378115868177,-1.9893556358529,-1.90508589613195,-1.82145083606717,
-1.79406927610656,-1.78088810966333,-1.77088744287616,-1.71192459622475,
-1.62862729253653,-1.54477045235636,-1.46093259841181,-1.37847743944056,
-1.34755675482634,-1.32641194414506,-1.31774824508864,-1.2348333999042,
-1.15208726165353,-1.13111196252682,-1.04809579835495,-0.965185374476776,
-0.914579677665573,-0.892439685310672,-0.877969115241355,-0.870243964987608,
-0.788175424134281,-0.706044237682933,-0.624661608660605,-0.560339799987152,
-0.490297324988758,-0.459653742176961,-0.439904400316136,-0.429071911044687,
-0.348385687679688,-0.267119065290005,-0.186022614582263,-0.105553499032249,
-0.0264972650708247,0.),.UNSPECIFIED.);
#6081=B_SPLINE_CURVE_WITH_KNOTS('',3,(#35672,#35673,#35674,#35675,#35676,
#35677,#35678,#35679,#35680,#35681,#35682,#35683,#35684,#35685,#35686,#35687,
#35688,#35689,#35690,#35691,#35692,#35693),.UNSPECIFIED.,.F.,.F.,(4,3,3,
3,3,3,3,4),(32.542054101172,32.9968752454902,33.4968279007249,33.9967805559596,
34.4967332111943,34.996685866429,35.4966385216637,35.9188760060433),
 .UNSPECIFIED.);
#6082=B_SPLINE_CURVE_WITH_KNOTS('',3,(#35694,#35695,#35696,#35697,#35698,
#35699,#35700,#35701,#35702,#35703,#35704,#35705,#35706,#35707),
 .UNSPECIFIED.,.F.,.F.,(4,1,1,1,1,1,1,1,1,1,1,4),(10.3761761872892,10.7984136716688,
11.2983663269035,11.7983189821382,12.2982716373729,12.7982242926076,13.2981769478423,
13.798129603077,14.2980822583117,14.7980349135464,15.2979875687811,15.707963267949),
 .UNSPECIFIED.);
#6083=B_SPLINE_CURVE_WITH_KNOTS('',3,(#35709,#35710,#35711,#35712,#35713,
#35714,#35715,#35716,#35717,#35718,#35719,#35720),.UNSPECIFIED.,.F.,.F.,
(4,1,1,1,1,1,1,1,1,4),(11.6149723878396,12.1149250430743,12.614877698309,
13.1148303535437,13.6147830087784,14.1147356640131,14.6146883192478,15.1146409744825,
15.6145936297172,15.707963267949),.UNSPECIFIED.);
#6084=B_SPLINE_CURVE_WITH_KNOTS('',3,(#36037,#36038,#36039,#36040,#36041,
#36042,#36043,#36044,#36045,#36046,#36047,#36048,#36049,#36050,#36051,#36052),
 .UNSPECIFIED.,.F.,.F.,(4,3,3,3,3,4),(-37.9964017978372,-37.4964491426025,
-36.9964964873678,-36.4965438321331,-35.9965911768984,-35.5089174160073),
 .UNSPECIFIED.);
#6085=B_SPLINE_CURVE_WITH_KNOTS('',3,(#36741,#36742,#36743,#36744,#36745,
#36746,#36747,#36748,#36749,#36750),.UNSPECIFIED.,.F.,.F.,(4,3,3,4),(-4.09274904019423,
-3.94775640367428,-2.96081730275571,-2.06120159751578),.UNSPECIFIED.);
#6086=B_SPLINE_CURVE_WITH_KNOTS('',3,(#36753,#36754,#36755,#36756,#36757,
#36758,#36759),.UNSPECIFIED.,.F.,.F.,(4,3,4),(0.,0.986939100918566,1.11004521091131),
 .UNSPECIFIED.);
#6087=B_SPLINE_CURVE_WITH_KNOTS('',3,(#36764,#36765,#36766,#36767,#36768,
#36769,#36770,#36771,#36772,#36773,#36774,#36775,#36776,#36777,#36778,#36779,
#36780,#36781,#36782,#36783,#36784,#36785),.UNSPECIFIED.,.F.,.F.,(4,3,3,
3,3,3,3,4),(-10.3759343473738,-9.8693910091857,-8.88245190826713,-7.89551280734856,
-6.90857370642999,-5.92163460551142,-4.93469550459285,-4.09274904019423),
 .UNSPECIFIED.);
#6088=B_SPLINE_CURVE_WITH_KNOTS('',3,(#36786,#36787,#36788,#36789,#36790,
#36791,#36792,#36793,#36794,#36795,#36796,#36797,#36798,#36799,#36800,#36801,
#36802,#36803,#36804,#36805,#36806,#36807),.UNSPECIFIED.,.F.,.F.,(4,3,3,
3,3,3,3,4),(1.11004521091131,1.97387820183714,2.96081730275571,3.94775640367428,
4.93469550459285,5.92163460551142,6.90857370642999,7.39323051809089),
 .UNSPECIFIED.);
#6089=B_SPLINE_CURVE_WITH_KNOTS('',3,(#36812,#36813,#36814,#36815,#36816,
#36817,#36818,#36819,#36820,#36821,#36822,#36823,#36824,#36825,#36826,#36827,
#36828,#36829,#36830,#36831,#36832,#36833),.UNSPECIFIED.,.F.,.F.,(4,3,3,
3,3,3,3,4),(-16.6591196545534,-15.7910256146971,-14.8040865137786,-13.81714741286,
-12.8302083119414,-11.8432692110228,-10.8563301101043,-10.3759343473738),
 .UNSPECIFIED.);
#6090=B_SPLINE_CURVE_WITH_KNOTS('',3,(#36834,#36835,#36836,#36837,#36838,
#36839,#36840,#36841,#36842,#36843,#36844,#36845,#36846,#36847,#36848,#36849,
#36850,#36851,#36852,#36853,#36854,#36855),.UNSPECIFIED.,.F.,.F.,(4,3,3,
3,3,3,3,4),(7.39323051809089,7.89551280734856,8.88245190826713,9.8693910091857,
10.8563301101043,11.8432692110228,12.8302083119414,13.6764158252705),
 .UNSPECIFIED.);
#6091=B_SPLINE_CURVE_WITH_KNOTS('',3,(#36860,#36861,#36862,#36863,#36864,
#36865,#36866,#36867,#36868,#36869,#36870,#36871,#36872,#36873,#36874,#36875,
#36876,#36877,#36878,#36879,#36880,#36881,#36882,#36883,#36884),
 .UNSPECIFIED.,.F.,.F.,(4,3,3,3,3,3,3,3,4),(-22.942304961733,-22.6995993211271,
-21.7126602202085,-20.72572111929,-19.7387820183714,-18.7518429174528,-17.7649038165343,
-16.7779647156157,-16.6591196545534),.UNSPECIFIED.);
#6092=B_SPLINE_CURVE_WITH_KNOTS('',3,(#36885,#36886,#36887,#36888,#36889,
#36890,#36891,#36892,#36893,#36894,#36895,#36896,#36897,#36898,#36899,#36900,
#36901,#36902,#36903,#36904,#36905,#36906,#36907,#36908,#36909),
 .UNSPECIFIED.,.F.,.F.,(4,3,3,3,3,3,3,3,4),(13.6764158252705,13.81714741286,
14.8040865137786,15.7910256146971,16.7779647156157,17.7649038165343,18.7518429174528,
19.7387820183714,19.9596011324501),.UNSPECIFIED.);
#6093=B_SPLINE_CURVE_WITH_KNOTS('',3,(#36914,#36915,#36916,#36917,#36918,
#36919,#36920,#36921,#36922,#36923,#36924,#36925,#36926,#36927,#36928,#36929,
#36930,#36931,#36932,#36933,#36934,#36935),.UNSPECIFIED.,.F.,.F.,(4,3,3,
3,3,3,3,4),(-29.2254902689126,-28.6212339266385,-27.63429482572,-26.6473557248014,
-25.6604166238828,-24.6734775229643,-23.6865384220457,-22.942304961733),
 .UNSPECIFIED.);
#6094=B_SPLINE_CURVE_WITH_KNOTS('',3,(#36936,#36937,#36938,#36939,#36940,
#36941,#36942,#36943,#36944,#36945,#36946,#36947,#36948,#36949,#36950,#36951,
#36952,#36953,#36954,#36955,#36956,#36957),.UNSPECIFIED.,.F.,.F.,(4,3,3,
3,3,3,3,4),(19.9596011324501,20.72572111929,21.7126602202085,22.6995993211271,
23.6865384220457,24.6734775229642,25.6604166238828,26.2427864396297),
 .UNSPECIFIED.);
#6095=B_SPLINE_CURVE_WITH_KNOTS('',3,(#36962,#36963,#36964,#36965,#36966,
#36967,#36968,#36969,#36970,#36971,#36972,#36973,#36974,#36975,#36976,#36977,
#36978,#36979,#36980,#36981,#36982,#36983),.UNSPECIFIED.,.F.,.F.,(4,3,3,
3,3,3,3,4),(-35.5086755760922,-34.54286853215,-33.5559294312314,-32.5689903303128,
-31.5820512293942,-30.5951121284757,-29.6081730275571,-29.2254902689126),
 .UNSPECIFIED.);
#6096=B_SPLINE_CURVE_WITH_KNOTS('',3,(#36984,#36985,#36986,#36987,#36988,
#36989,#36990,#36991,#36992,#36993,#36994,#36995,#36996,#36997,#36998,#36999,
#37000,#37001,#37002,#37003,#37004,#37005),.UNSPECIFIED.,.F.,.F.,(4,3,3,
3,3,3,3,4),(26.2427864396297,26.6473557248014,27.63429482572,28.6212339266385,
29.6081730275571,30.5951121284757,31.5820512293942,32.5259717468092),
 .UNSPECIFIED.);
#6097=B_SPLINE_CURVE_WITH_KNOTS('',3,(#37010,#37011,#37012,#37013,#37014,
#37015,#37016,#37017,#37018,#37019,#37020,#37021,#37022,#37023,#37024,#37025,
#37026,#37027,#37028,#37029,#37030,#37031,#37032,#37033,#37034),
 .UNSPECIFIED.,.F.,.F.,(4,3,3,3,3,3,3,3,4),(-41.7918608832717,-41.4514422385799,
-40.4645031376614,-39.4775640367428,-38.4906249358242,-37.5036858349057,
-36.5167467339871,-35.5298076330685,-35.5086755760922),.UNSPECIFIED.);
#6098=B_SPLINE_CURVE_WITH_KNOTS('',3,(#37035,#37036,#37037,#37038,#37039,
#37040,#37041,#37042,#37043,#37044,#37045,#37046,#37047,#37048,#37049,#37050,
#37051,#37052,#37053,#37054,#37055,#37056,#37057,#37058,#37059),
 .UNSPECIFIED.,.F.,.F.,(4,3,3,3,3,3,3,3,4),(32.5259717468092,32.5689903303128,
33.5559294312314,34.54286853215,35.5298076330685,36.5167467339871,37.5036858349057,
38.4906249358242,38.8091570539888),.UNSPECIFIED.);
#6099=B_SPLINE_CURVE_WITH_KNOTS('',3,(#37064,#37065,#37066,#37067,#37068,
#37069,#37070,#37071,#37072,#37073,#37074,#37075,#37076,#37077,#37078,#37079,
#37080,#37081,#37082,#37083,#37084,#37085),.UNSPECIFIED.,.F.,.F.,(4,3,3,
3,3,3,3,4),(-48.0750461904514,-47.3730768440914,-46.3861377431728,-45.3991986422542,
-44.4122595413357,-43.4253204404171,-42.4383813394985,-41.7918608832717),
 .UNSPECIFIED.);
#6100=B_SPLINE_CURVE_WITH_KNOTS('',3,(#37086,#37087,#37088,#37089,#37090,
#37091,#37092,#37093,#37094,#37095,#37096,#37097,#37098,#37099,#37100,#37101,
#37102,#37103,#37104,#37105,#37106,#37107),.UNSPECIFIED.,.F.,.F.,(4,3,3,
3,3,3,3,4),(38.8091570539888,39.4775640367428,40.4645031376614,41.4514422385799,
42.4383813394985,43.4253204404171,44.4122595413357,45.0923423611684),
 .UNSPECIFIED.);
#6101=B_SPLINE_CURVE_WITH_KNOTS('',3,(#37112,#37113,#37114,#37115,#37116,
#37117,#37118,#37119,#37120,#37121,#37122,#37123,#37124,#37125,#37126,#37127,
#37128,#37129,#37130,#37131,#37132,#37133,#37134,#37135,#37136),
 .UNSPECIFIED.,.F.,.F.,(4,3,3,3,3,3,3,3,4),(-54.3582314976309,-54.2816505505214,
-53.2947114496028,-52.3077723486842,-51.3208332477656,-50.3338941468471,
-49.3469550459285,-48.3600159450099,-48.0750461904514),.UNSPECIFIED.);
#6102=B_SPLINE_CURVE_WITH_KNOTS('',3,(#37137,#37138,#37139,#37140,#37141,
#37142,#37143,#37144,#37145,#37146,#37147,#37148,#37149,#37150,#37151,#37152,
#37153,#37154,#37155,#37156,#37157,#37158,#37159,#37160,#37161),
 .UNSPECIFIED.,.F.,.F.,(4,3,3,3,3,3,3,3,4),(45.0923423611684,45.3991986422542,
46.3861377431728,47.3730768440914,48.3600159450099,49.3469550459285,50.3338941468471,
51.3208332477656,51.375527668348),.UNSPECIFIED.);
#6103=B_SPLINE_CURVE_WITH_KNOTS('',3,(#37168,#37169,#37170,#37171,#37172,
#37173,#37174,#37175,#37176,#37177,#37178,#37179,#37180,#37181,#37182,#37183,
#37184,#37185,#37186),.UNSPECIFIED.,.F.,.F.,(4,3,3,3,3,3,4),(-60.2032851560328,
-59.2163460551142,-58.2294069541956,-57.2424678532771,-56.2555287523585,
-55.2685896514399,-54.3582314976309),.UNSPECIFIED.);
#6104=B_SPLINE_CURVE_WITH_KNOTS('',3,(#37187,#37188,#37189,#37190,#37191,
#37192,#37193,#37194,#37195,#37196,#37197,#37198,#37199,#37200,#37201,#37202,
#37203,#37204,#37205,#37206,#37207,#37208),.UNSPECIFIED.,.F.,.F.,(4,3,3,
3,3,3,3,4),(51.375527668348,52.3077723486842,53.2947114496028,54.2816505505213,
55.2685896514399,56.2555287523585,57.242467853277,57.6587129755276),
 .UNSPECIFIED.);
#6105=B_SPLINE_CURVE_WITH_KNOTS('',3,(#37214,#37215,#37216,#37217,#37218,
#37219,#37220),.UNSPECIFIED.,.F.,.F.,(4,1,1,1,4),(65.9734457253856,66.8838038791946,
67.8707429801132,68.8576820810318,69.7572977862717),.UNSPECIFIED.);
#6106=B_SPLINE_CURVE_WITH_KNOTS('',3,(#37223,#37224,#37225,#37226,#37227,
#37228),.UNSPECIFIED.,.F.,.F.,(4,1,1,4),(65.9734457253856,66.5441397040536,
67.5310788049722,68.5180179058908),.UNSPECIFIED.);
#6107=B_SPLINE_CURVE_WITH_KNOTS('',3,(#37233,#37234,#37235,#37236,#37237,
#37238,#37239,#37240,#37241,#37242,#37243),.UNSPECIFIED.,.F.,.F.,(4,1,1,
1,1,1,1,1,4),(59.6902604182061,59.9752301727646,60.9621692736832,61.9491083746018,
62.9360474755203,63.9229865764389,64.9099256773575,65.8968647782761,65.9734457253856),
 .UNSPECIFIED.);
#6108=B_SPLINE_CURVE_WITH_KNOTS('',3,(#37244,#37245,#37246,#37247,#37248,
#37249,#37250,#37251,#37252,#37253),.UNSPECIFIED.,.F.,.F.,(4,1,1,1,1,1,
1,4),(59.6902604182061,60.6225050985422,61.6094441994608,62.5963833003793,
63.5833224012979,64.5702615022165,65.557200603135,65.9734457253856),
 .UNSPECIFIED.);
#6109=B_SPLINE_CURVE_WITH_KNOTS('',3,(#37258,#37259,#37260,#37261,#37262,
#37263,#37264,#37265,#37266,#37267),.UNSPECIFIED.,.F.,.F.,(4,1,1,1,1,1,
1,4),(53.4070751110265,54.0535955672532,55.0405346681718,56.0274737690903,
57.0144128700089,58.0013519709275,58.9882910718461,59.6902604182061),
 .UNSPECIFIED.);
#6110=B_SPLINE_CURVE_WITH_KNOTS('',3,(#37268,#37269,#37270,#37271,#37272,
#37273,#37274,#37275,#37276,#37277,#37278),.UNSPECIFIED.,.F.,.F.,(4,1,1,
1,1,1,1,1,4),(53.4070751110265,53.7139313921122,54.7008704930308,55.6878095939493,
56.6747486948679,57.6616877957865,58.6486268967051,59.6355659976236,59.6902604182061),
 .UNSPECIFIED.);
#6111=B_SPLINE_CURVE_WITH_KNOTS('',3,(#37283,#37284,#37285,#37286,#37287,
#37288,#37289,#37290,#37291,#37292,#37293),.UNSPECIFIED.,.F.,.F.,(4,1,1,
1,1,1,1,1,4),(47.1238898038469,47.1450218608232,48.1319609617418,49.1189000626604,
50.1058391635789,51.0927782644975,52.0797173654161,53.0666564663346,53.4070751110265),
 .UNSPECIFIED.);
#6112=B_SPLINE_CURVE_WITH_KNOTS('',3,(#37294,#37295,#37296,#37297,#37298,
#37299,#37300,#37301,#37302,#37303),.UNSPECIFIED.,.F.,.F.,(4,1,1,1,1,1,
1,4),(47.1238898038469,47.7922967866008,48.7792358875193,49.7661749884379,
50.7531140893565,51.7400531902751,52.7269922911936,53.4070751110265),
 .UNSPECIFIED.);
#6113=B_SPLINE_CURVE_WITH_KNOTS('',3,(#37308,#37309,#37310,#37311,#37312,
#37313,#37314,#37315,#37316,#37317),.UNSPECIFIED.,.F.,.F.,(4,1,1,1,1,1,
1,4),(40.8407044966673,41.2233872553118,42.2103263562304,43.1972654571489,
44.1842045580675,45.1711436589861,46.1580827599046,47.1238898038469),
 .UNSPECIFIED.);
#6114=B_SPLINE_CURVE_WITH_KNOTS('',3,(#37318,#37319,#37320,#37321,#37322,
#37323,#37324,#37325,#37326,#37327,#37328),.UNSPECIFIED.,.F.,.F.,(4,1,1,
1,1,1,1,1,4),(40.8407044966673,40.8837230801708,41.8706621810894,42.8576012820079,
43.8445403829265,44.8314794838451,45.8184185847636,46.8053576856822,47.1238898038469),
 .UNSPECIFIED.);
#6115=B_SPLINE_CURVE_WITH_KNOTS('',3,(#37333,#37334,#37335,#37336,#37337,
#37338,#37339,#37340,#37341,#37342),.UNSPECIFIED.,.F.,.F.,(4,1,1,1,1,1,
1,4),(34.5575191894877,35.3017526498004,36.2886917507189,37.2756308516375,
38.2625699525561,39.2495090534747,40.2364481543932,40.8407044966673),
 .UNSPECIFIED.);
#6116=B_SPLINE_CURVE_WITH_KNOTS('',3,(#37343,#37344,#37345,#37346,#37347,
#37348,#37349,#37350,#37351,#37352),.UNSPECIFIED.,.F.,.F.,(4,1,1,1,1,1,
1,4),(34.5575191894877,34.9620884746594,35.9490275755779,36.9359666764965,
37.9229057774151,38.9098448783337,39.8967839792522,40.8407044966673),
 .UNSPECIFIED.);
#6117=B_SPLINE_CURVE_WITH_KNOTS('',3,(#37357,#37358,#37359,#37360,#37361,
#37362,#37363,#37364,#37365,#37366,#37367),.UNSPECIFIED.,.F.,.F.,(4,1,1,
1,1,1,1,1,4),(28.2743338823081,28.3931789433704,29.380118044289,30.3670571452075,
31.3539962461261,32.3409353470447,33.3278744479632,34.3148135488818,34.5575191894877),
 .UNSPECIFIED.);
#6118=B_SPLINE_CURVE_WITH_KNOTS('',3,(#37368,#37369,#37370,#37371,#37372,
#37373,#37374,#37375,#37376,#37377),.UNSPECIFIED.,.F.,.F.,(4,1,1,1,1,1,
1,4),(28.2743338823081,29.040453869148,30.0273929700665,31.0143320709851,
32.0012711719037,32.9882102728222,33.9751493737408,34.5575191894877),
 .UNSPECIFIED.);
#6119=B_SPLINE_CURVE_WITH_KNOTS('',3,(#37382,#37383,#37384,#37385,#37386,
#37387,#37388,#37389,#37390,#37391),.UNSPECIFIED.,.F.,.F.,(4,1,1,1,1,1,
1,4),(21.9911485751285,22.471544337859,23.4584834387775,24.4454225396961,
25.4323616406147,26.4193007415332,27.4062398424518,28.2743338823081),
 .UNSPECIFIED.);
#6120=B_SPLINE_CURVE_WITH_KNOTS('',3,(#37392,#37393,#37394,#37395,#37396,
#37397,#37398,#37399,#37400,#37401,#37402),.UNSPECIFIED.,.F.,.F.,(4,1,1,
1,1,1,1,1,4),(21.9911485751285,22.131880162718,23.1188192636365,24.1057583645551,
25.0926974654737,26.0796365663922,27.0665756673108,28.0535147682294,28.2743338823081),
 .UNSPECIFIED.);
#6121=B_SPLINE_CURVE_WITH_KNOTS('',3,(#37407,#37408,#37409,#37410,#37411,
#37412,#37413,#37414,#37415,#37416),.UNSPECIFIED.,.F.,.F.,(4,1,1,1,1,1,
1,4),(15.7079632679489,16.5499097323475,17.5368488332661,18.5237879341847,
19.5107270351033,20.4976661360218,21.4846052369404,21.9911485751285),
 .UNSPECIFIED.);
#6122=B_SPLINE_CURVE_WITH_KNOTS('',3,(#37417,#37418,#37419,#37420,#37421,
#37422,#37423,#37424,#37425,#37426),.UNSPECIFIED.,.F.,.F.,(4,1,1,1,1,1,
1,4),(15.7079632679489,16.2102455572066,17.1971846581251,18.1841237590437,
19.1710628599623,20.1580019608808,21.1449410617994,21.9911485751285),
 .UNSPECIFIED.);
#6123=B_SPLINE_CURVE_WITH_KNOTS('',3,(#37453,#37454,#37455,#37456,#37457,
#37458,#37459,#37460,#37461,#37462,#37463,#37464,#37465,#37466,#37467,#37468,
#37469,#37470,#37471,#37472,#37473,#37474,#37475,#37476,#37477,#37478,#37479,
#37480,#37481,#37482,#37483,#37484,#37485,#37486,#37487,#37488,#37489,#37490,
#37491,#37492,#37493,#37494,#37495,#37496,#37497,#37498,#37499,#37500,#37501,
#37502,#37503,#37504,#37505,#37506,#37507,#37508,#37509,#37510,#37511,#37512,
#37513,#37514,#37515,#37516,#37517,#37518,#37519,#37520,#37521,#37522,#37523,
#37524,#37525,#37526,#37527,#37528,#37529,#37530,#37531,#37532,#37533,#37534,
#37535,#37536,#37537,#37538,#37539,#37540,#37541,#37542,#37543,#37544,#37545,
#37546,#37547,#37548,#37549),.UNSPECIFIED.,.F.,.F.,(4,3,3,3,3,3,3,3,3,3,
3,3,3,3,3,3,3,3,3,3,3,3,3,3,3,3,3,3,3,3,3,3,4),(-0.744397949170625,-0.71583061742043,
-0.684607549726404,-0.665225811669408,-0.65913755838546,-0.653541781901175,
-0.621561581432833,-0.590678851355536,-0.576678185830625,-0.57109179287764,
-0.537836542473585,-0.504009698787253,-0.47015729823496,-0.446242908879834,
-0.439103797305219,-0.43297135889342,-0.398062560014724,-0.374499740814454,
-0.340715815821642,-0.306315596621499,-0.298239329175978,-0.292491744365664,
-0.258101152324883,-0.222604526272566,-0.186772073569507,-0.163425564373319,
-0.155579823557629,-0.15073619345339,-0.145686377983342,-0.108957740119569,
-0.0721606235587895,-0.0360477125188044,0.),.UNSPECIFIED.);
#6124=B_SPLINE_CURVE_WITH_KNOTS('',3,(#37552,#37553,#37554,#37555,#37556,
#37557,#37558,#37559,#37560,#37561,#37562,#37563,#37564,#37565,#37566,#37567,
#37568,#37569,#37570,#37571,#37572,#37573,#37574,#37575,#37576,#37577,#37578,
#37579,#37580,#37581,#37582,#37583,#37584,#37585,#37586,#37587,#37588,#37589,
#37590,#37591,#37592,#37593,#37594,#37595,#37596,#37597,#37598,#37599,#37600,
#37601,#37602,#37603,#37604,#37605,#37606,#37607,#37608,#37609,#37610,#37611,
#37612,#37613,#37614,#37615,#37616,#37617,#37618,#37619,#37620,#37621,#37622,
#37623,#37624,#37625,#37626,#37627,#37628,#37629,#37630,#37631,#37632,#37633,
#37634,#37635,#37636,#37637,#37638,#37639,#37640,#37641,#37642,#37643,#37644,
#37645,#37646,#37647,#37648),.UNSPECIFIED.,.F.,.F.,(4,3,3,3,3,3,3,3,3,3,
3,3,3,3,3,3,3,3,3,3,3,3,3,3,3,3,3,3,3,3,3,3,4),(-0.741270768406444,-0.707014008746377,
-0.670388059051889,-0.649568879284289,-0.641049525894248,-0.635068301219589,
-0.597844911413426,-0.565274445333034,-0.551024866422862,-0.542258222203151,
-0.537238417066858,-0.501842280952796,-0.466685322391887,-0.432561860623243,
-0.408741691160004,-0.399271293306569,-0.394872553388672,-0.361244518471948,
-0.337281182770287,-0.302985270379873,-0.268599115564268,-0.261938858357407,
-0.257215965685261,-0.223801404360543,-0.190343263618923,-0.157286202950517,
-0.137625427581702,-0.128383055216145,-0.123812703710246,-0.0916026903308386,
-0.0598378393002095,-0.0290475787521256,0.),.UNSPECIFIED.);
#6125=B_SPLINE_CURVE_WITH_KNOTS('',3,(#37905,#37906,#37907,#37908),
 .UNSPECIFIED.,.F.,.F.,(4,4),(57.6587129755276,58.142083558517),
 .UNSPECIFIED.);
#6126=B_SPLINE_CURVE_WITH_KNOTS('',3,(#37910,#37911,#37912,#37913,#37914,
#37915,#37916,#37917,#37918,#37919,#37920,#37921,#37922,#37923,#37924,#37925,
#37926,#37927,#37928,#37929,#37930,#37931,#37932,#37933,#37934,#37935,#37936,
#37937,#37938,#37939,#37940,#37941,#37942,#37943,#37944,#37945,#37946,#37947,
#37948,#37949,#37950,#37951,#37952,#37953,#37954,#37955,#37956,#37957,#37958,
#37959,#37960,#37961,#37962,#37963,#37964,#37965,#37966,#37967,#37968,#37969,
#37970,#37971,#37972,#37973,#37974,#37975,#37976,#37977,#37978,#37979,#37980,
#37981,#37982,#37983,#37984,#37985,#37986,#37987,#37988,#37989,#37990,#37991,
#37992,#37993,#37994,#37995,#37996,#37997,#37998,#37999,#38000,#38001,#38002,
#38003,#38004,#38005,#38006),.UNSPECIFIED.,.F.,.F.,(4,3,3,3,3,3,3,3,3,3,
3,3,3,3,3,3,3,3,3,3,3,3,3,3,3,3,3,3,3,3,3,3,4),(-0.744397949170611,-0.715830617420419,
-0.684607520785607,-0.66522578453741,-0.659137478993546,-0.653541760046644,
-0.621561531951959,-0.59067880805977,-0.576678114100325,-0.571091693875746,
-0.537836424408794,-0.504009574985985,-0.470157175969216,-0.446242817180524,
-0.439103398439934,-0.432971303885224,-0.398062506635795,-0.374499740814447,
-0.340715801391881,-0.306315566008677,-0.298239138263934,-0.292491696861189,
-0.258101090438267,-0.222604447663952,-0.186771987988499,-0.163425489489936,
-0.155579680387924,-0.150736029870234,-0.145686340478701,-0.108957693422131,
-0.0721605833636332,-0.0360477121925127,0.),.UNSPECIFIED.);
#6127=B_SPLINE_CURVE_WITH_KNOTS('',3,(#38007,#38008,#38009,#38010,#38011,
#38012,#38013,#38014,#38015),.UNSPECIFIED.,.F.,.F.,(4,1,1,1,1,1,4),(10.3759343473738,
11.2755500526137,12.2624891535323,13.2494282544508,14.2363673553694,15.223306456288,
15.7079632679489),.UNSPECIFIED.);
#6128=B_SPLINE_CURVE_WITH_KNOTS('',3,(#38019,#38020,#38021,#38022,#38023,
#38024,#38025,#38026),.UNSPECIFIED.,.F.,.F.,(4,1,1,1,1,4),(11.6152142277547,
12.6021533286733,13.5890924295918,14.5760315305104,15.562970631429,15.7079632679489),
 .UNSPECIFIED.);
#6129=B_SPLINE_CURVE_WITH_KNOTS('',3,(#38283,#38284,#38285,#38286,#38287,
#38288,#38289,#38290,#38291,#38292,#38293,#38294,#38295,#38296,#38297,#38298,
#38299,#38300,#38301,#38302,#38303,#38304,#38305,#38306,#38307,#38308,#38309,
#38310,#38311,#38312,#38313,#38314,#38315,#38316,#38317,#38318,#38319,#38320,
#38321,#38322,#38323,#38324,#38325,#38326,#38327,#38328,#38329,#38330,#38331,
#38332,#38333,#38334,#38335,#38336,#38337,#38338,#38339,#38340,#38341,#38342,
#38343,#38344,#38345,#38346,#38347,#38348,#38349,#38350,#38351,#38352,#38353,
#38354,#38355,#38356,#38357,#38358,#38359,#38360,#38361,#38362,#38363,#38364,
#38365,#38366,#38367,#38368,#38369,#38370,#38371,#38372,#38373,#38374,#38375,
#38376,#38377,#38378,#38379),.UNSPECIFIED.,.F.,.F.,(4,3,3,3,3,3,3,3,3,3,
3,3,3,3,3,3,3,3,3,3,3,3,3,3,3,3,3,3,3,3,3,3,4),(-0.741270768406357,-0.707014008746274,
-0.670388059544822,-0.649568879746411,-0.641049544639479,-0.635068332322656,
-0.597844938628606,-0.565274469146312,-0.551024888747808,-0.542258278765346,
-0.537238527650124,-0.501842393489449,-0.466685446597756,-0.432562017839177,
-0.408741809071946,-0.399271703402815,-0.394873316318385,-0.3612453002017,
-0.337281182770253,-0.302985287215554,-0.268599125561966,-0.261938743205762,
-0.25721588929756,-0.22380133845036,-0.190343187133,-0.157286094955077,
-0.137625333085692,-0.128382691599488,-0.123812193525018,-0.091602157735499,
-0.0598372732219336,-0.0290469650055772,0.),.UNSPECIFIED.);
#6130=B_SPLINE_CURVE_WITH_KNOTS('',3,(#38398,#38399,#38400,#38401,#38402,
#38403,#38404,#38405,#38406,#38407),.UNSPECIFIED.,.F.,.F.,(4,3,3,4),(-4.09274904019427,
-3.99053949058499,-2.99290461793874,-2.06120159751576),.UNSPECIFIED.);
#6131=B_SPLINE_CURVE_WITH_KNOTS('',3,(#38410,#38411,#38412,#38413,#38414,
#38415,#38416),.UNSPECIFIED.,.F.,.F.,(4,3,4),(0.,0.997634872646276,1.11004521091191),
 .UNSPECIFIED.);
#6132=B_SPLINE_CURVE_WITH_KNOTS('',3,(#38421,#38422,#38423,#38424,#38425,
#38426,#38427,#38428,#38429,#38430,#38431,#38432,#38433,#38434,#38435,#38436,
#38437,#38438,#38439,#38440,#38441,#38442),.UNSPECIFIED.,.F.,.F.,(4,3,3,
3,3,3,3,4),(-10.3759343473739,-9.97634872646248,-8.97871385381623,-7.98107898116998,
-6.98344410852373,-5.98580923587749,-4.98817436323124,-4.09274904019427),
 .UNSPECIFIED.);
#6133=B_SPLINE_CURVE_WITH_KNOTS('',3,(#38443,#38444,#38445,#38446,#38447,
#38448,#38449,#38450,#38451,#38452,#38453,#38454,#38455,#38456,#38457,#38458,
#38459,#38460,#38461,#38462,#38463,#38464),.UNSPECIFIED.,.F.,.F.,(4,3,3,
3,3,3,3,4),(1.11004521091191,1.99526974529252,2.99290461793875,3.99053949058499,
4.98817436323123,5.98580923587746,6.9834441085237,7.3932305180915),
 .UNSPECIFIED.);
#6134=B_SPLINE_CURVE_WITH_KNOTS('',3,(#38469,#38470,#38471,#38472,#38473,
#38474,#38475,#38476,#38477,#38478,#38479,#38480,#38481,#38482,#38483,#38484,
#38485,#38486,#38487,#38488,#38489,#38490),.UNSPECIFIED.,.F.,.F.,(4,3,3,
3,3,3,3,4),(-16.6591196545534,-15.96215796234,-14.9645230896937,-13.9668882170475,
-12.9692533444012,-11.971618471755,-10.9739835991087,-10.3759343473739),
 .UNSPECIFIED.);
#6135=B_SPLINE_CURVE_WITH_KNOTS('',3,(#38491,#38492,#38493,#38494,#38495,
#38496,#38497,#38498,#38499,#38500,#38501,#38502,#38503,#38504,#38505,#38506,
#38507,#38508,#38509,#38510,#38511,#38512),.UNSPECIFIED.,.F.,.F.,(4,3,3,
3,3,3,3,4),(7.3932305180915,7.98107898116995,8.97871385381621,9.97634872646246,
10.9739835991087,11.971618471755,12.9692533444012,13.6764158252711),
 .UNSPECIFIED.);
#6136=B_SPLINE_CURVE_WITH_KNOTS('',3,(#38517,#38518,#38519,#38520,#38521,
#38522,#38523,#38524,#38525,#38526,#38527,#38528,#38529,#38530,#38531,#38532,
#38533,#38534,#38535,#38536,#38537,#38538),.UNSPECIFIED.,.F.,.F.,(4,3,3,
3,3,3,3,4),(-22.942304961733,-21.9479671982174,-20.9503323255712,-19.952697452925,
-18.9550625802787,-17.9574277076325,-16.9597928349862,-16.6591196545534),
 .UNSPECIFIED.);
#6137=B_SPLINE_CURVE_WITH_KNOTS('',3,(#38539,#38540,#38541,#38542,#38543,
#38544,#38545,#38546,#38547,#38548,#38549,#38550,#38551,#38552,#38553,#38554,
#38555,#38556,#38557,#38558,#38559,#38560,#38561,#38562,#38563),
 .UNSPECIFIED.,.F.,.F.,(4,3,3,3,3,3,3,3,4),(13.6764158252711,13.9668882170475,
14.9645230896937,15.96215796234,16.9597928349862,17.9574277076325,18.9550625802787,
19.9526974529249,19.9596011324507),.UNSPECIFIED.);
#6138=B_SPLINE_CURVE_WITH_KNOTS('',3,(#38568,#38569,#38570,#38571,#38572,
#38573,#38574,#38575,#38576,#38577,#38578,#38579,#38580,#38581,#38582,#38583,
#38584,#38585,#38586,#38587,#38588,#38589,#38590,#38591,#38592),
 .UNSPECIFIED.,.F.,.F.,(4,3,3,3,3,3,3,3,4),(-29.2254902689126,-28.9314113067412,
-27.9337764340949,-26.9361415614487,-25.9385066888024,-24.9408718161562,
-23.9432369435099,-22.9456020708637,-22.942304961733),.UNSPECIFIED.);
#6139=B_SPLINE_CURVE_WITH_KNOTS('',3,(#38593,#38594,#38595,#38596,#38597,
#38598,#38599,#38600,#38601,#38602,#38603,#38604,#38605,#38606,#38607,#38608,
#38609,#38610,#38611,#38612,#38613,#38614),.UNSPECIFIED.,.F.,.F.,(4,3,3,
3,3,3,3,4),(19.9596011324507,20.9503323255712,21.9479671982174,22.9456020708637,
23.9432369435099,24.9408718161562,25.9385066888024,26.2427864396303),
 .UNSPECIFIED.);
#6140=B_SPLINE_CURVE_WITH_KNOTS('',3,(#38619,#38620,#38621,#38622,#38623,
#38624,#38625,#38626,#38627,#38628,#38629,#38630,#38631,#38632,#38633,#38634,
#38635,#38636,#38637,#38638,#38639,#38640),.UNSPECIFIED.,.F.,.F.,(4,3,3,
3,3,3,3,4),(-35.5086755760922,-34.9172205426187,-33.9195856699724,-32.9219507973262,
-31.9243159246799,-30.9266810520337,-29.9290461793874,-29.2254902689126),
 .UNSPECIFIED.);
#6141=B_SPLINE_CURVE_WITH_KNOTS('',3,(#38641,#38642,#38643,#38644,#38645,
#38646,#38647,#38648,#38649,#38650,#38651,#38652,#38653,#38654,#38655,#38656,
#38657,#38658,#38659,#38660,#38661,#38662),.UNSPECIFIED.,.F.,.F.,(4,3,3,
3,3,3,3,4),(26.2427864396303,26.9361415614487,27.9337764340949,28.9314113067412,
29.9290461793874,30.9266810520337,31.92431592468,32.5259717468098),
 .UNSPECIFIED.);
#6142=B_SPLINE_CURVE_WITH_KNOTS('',3,(#38667,#38668,#38669,#38670,#38671,
#38672,#38673,#38674,#38675,#38676,#38677,#38678,#38679,#38680,#38681,#38682,
#38683,#38684,#38685,#38686,#38687,#38688),.UNSPECIFIED.,.F.,.F.,(4,3,3,
3,3,3,3,4),(-41.7918608832718,-40.9030297784961,-39.9053949058499,-38.9077600332037,
-37.9101251605574,-36.9124902879112,-35.9148554152649,-35.5086755760922),
 .UNSPECIFIED.);
#6143=B_SPLINE_CURVE_WITH_KNOTS('',3,(#38689,#38690,#38691,#38692,#38693,
#38694,#38695,#38696,#38697,#38698,#38699,#38700,#38701,#38702,#38703,#38704,
#38705,#38706,#38707,#38708,#38709,#38710),.UNSPECIFIED.,.F.,.F.,(4,3,3,
3,3,3,3,4),(32.5259717468098,32.9219507973262,33.9195856699724,34.9172205426187,
35.9148554152649,36.9124902879112,37.9101251605574,38.8091570539894),
 .UNSPECIFIED.);
#6144=B_SPLINE_CURVE_WITH_KNOTS('',3,(#38715,#38716,#38717,#38718,#38719,
#38720,#38721,#38722,#38723,#38724,#38725,#38726,#38727,#38728,#38729,#38730,
#38731,#38732,#38733,#38734,#38735,#38736,#38737,#38738,#38739),
 .UNSPECIFIED.,.F.,.F.,(4,3,3,3,3,3,3,3,4),(-48.0750461904514,-47.8864738870199,
-46.8888390143736,-45.8912041417274,-44.8935692690811,-43.8959343964349,
-42.8982995237886,-41.9006646511424,-41.7918608832718),.UNSPECIFIED.);
#6145=B_SPLINE_CURVE_WITH_KNOTS('',3,(#38740,#38741,#38742,#38743,#38744,
#38745,#38746,#38747,#38748,#38749,#38750,#38751,#38752,#38753,#38754,#38755,
#38756,#38757,#38758,#38759,#38760,#38761,#38762,#38763,#38764),
 .UNSPECIFIED.,.F.,.F.,(4,3,3,3,3,3,3,3,4),(38.8091570539894,38.9077600332037,
39.9053949058499,40.9030297784962,41.9006646511424,42.8982995237887,43.8959343964349,
44.8935692690811,45.092342361169),.UNSPECIFIED.);
#6146=B_SPLINE_CURVE_WITH_KNOTS('',3,(#38769,#38770,#38771,#38772,#38773,
#38774,#38775,#38776,#38777,#38778,#38779,#38780,#38781,#38782,#38783,#38784,
#38785,#38786,#38787,#38788,#38789,#38790),.UNSPECIFIED.,.F.,.F.,(4,3,3,
3,3,3,3,4),(-54.358231497631,-53.8722831228974,-52.8746482502511,-51.8770133776049,
-50.8793785049586,-49.8817436323124,-48.8841087596661,-48.0750461904514),
 .UNSPECIFIED.);
#6147=B_SPLINE_CURVE_WITH_KNOTS('',3,(#38791,#38792,#38793,#38794,#38795,
#38796,#38797,#38798,#38799,#38800,#38801,#38802,#38803,#38804,#38805,#38806,
#38807,#38808,#38809,#38810,#38811,#38812),.UNSPECIFIED.,.F.,.F.,(4,3,3,
3,3,3,3,4),(45.092342361169,45.8912041417274,46.8888390143737,47.8864738870199,
48.8841087596661,49.8817436323124,50.8793785049587,51.3755276683486),
 .UNSPECIFIED.);
#6148=B_SPLINE_CURVE_WITH_KNOTS('',3,(#38817,#38818,#38819,#38820,#38821,
#38822,#38823,#38824,#38825,#38826,#38827,#38828,#38829,#38830,#38831,#38832,
#38833,#38834,#38835,#38836,#38837,#38838),.UNSPECIFIED.,.F.,.F.,(4,3,3,
3,3,3,3,4),(-60.6414168048106,-59.8580923587748,-58.8604574861286,-57.8628226134824,
-56.8651877408361,-55.8675528681899,-54.8699179955436,-54.358231497631),
 .UNSPECIFIED.);
#6149=B_SPLINE_CURVE_WITH_KNOTS('',3,(#38839,#38840,#38841,#38842,#38843,
#38844,#38845,#38846,#38847,#38848,#38849,#38850,#38851,#38852,#38853,#38854,
#38855,#38856,#38857,#38858,#38859,#38860),.UNSPECIFIED.,.F.,.F.,(4,3,3,
3,3,3,3,4),(51.3755276683486,51.8770133776049,52.8746482502512,53.8722831228974,
54.8699179955437,55.8675528681899,56.8651877408361,57.6587129755282),
 .UNSPECIFIED.);
#6150=B_SPLINE_CURVE_WITH_KNOTS('',3,(#38865,#38866,#38867,#38868,#38869,
#38870,#38871,#38872,#38873,#38874,#38875,#38876,#38877,#38878,#38879,#38880,
#38881,#38882,#38883,#38884,#38885,#38886,#38887,#38888,#38889),
 .UNSPECIFIED.,.F.,.F.,(4,3,3,3,3,3,3,3,4),(-66.9246021119902,-66.8415364672986,
-65.8439015946523,-64.8462667220061,-63.8486318493598,-62.8509969767136,
-61.8533621040674,-60.8557272314211,-60.6414168048106),.UNSPECIFIED.);
#6151=B_SPLINE_CURVE_WITH_KNOTS('',3,(#38890,#38891,#38892,#38893,#38894,
#38895,#38896,#38897,#38898,#38899,#38900,#38901,#38902,#38903,#38904,#38905,
#38906,#38907,#38908,#38909,#38910,#38911,#38912,#38913,#38914),
 .UNSPECIFIED.,.F.,.F.,(4,3,3,3,3,3,3,3,4),(57.6587129755282,57.8628226134824,
58.8604574861286,59.8580923587749,60.8557272314211,61.8533621040674,62.8509969767136,
63.8486318493599,63.9418982827078),.UNSPECIFIED.);
#6152=B_SPLINE_CURVE_WITH_KNOTS('',3,(#38919,#38920,#38921,#38922,#38923,
#38924,#38925,#38926,#38927,#38928,#38929,#38930,#38931,#38932,#38933,#38934,
#38935,#38936,#38937,#38938,#38939,#38940),.UNSPECIFIED.,.F.,.F.,(4,3,3,
3,3,3,3,4),(-73.2077874191698,-72.8273457031761,-71.8297108305298,-70.8320759578836,
-69.8344410852373,-68.8368062125911,-67.8391713399448,-66.9246021119902),
 .UNSPECIFIED.);
#6153=B_SPLINE_CURVE_WITH_KNOTS('',3,(#38941,#38942,#38943,#38944,#38945,
#38946,#38947,#38948,#38949,#38950,#38951,#38952,#38953,#38954,#38955,#38956,
#38957,#38958,#38959,#38960,#38961,#38962),.UNSPECIFIED.,.F.,.F.,(4,3,3,
3,3,3,3,4),(63.9418982827078,64.8462667220061,65.8439015946524,66.8415364672986,
67.8391713399448,68.8368062125911,69.8344410852373,70.2250835898874),
 .UNSPECIFIED.);
#6154=B_SPLINE_CURVE_WITH_KNOTS('',3,(#38967,#38968,#38969,#38970,#38971,
#38972,#38973,#38974,#38975,#38976,#38977,#38978,#38979,#38980,#38981,#38982,
#38983,#38984,#38985,#38986,#38987,#38988),.UNSPECIFIED.,.F.,.F.,(4,3,3,
3,3,3,3,4),(-79.4909727263494,-78.8131549390536,-77.8155200664073,-76.8178851937611,
-75.8202503211148,-74.8226154484686,-73.8249805758223,-73.2077874191698),
 .UNSPECIFIED.);
#6155=B_SPLINE_CURVE_WITH_KNOTS('',3,(#38989,#38990,#38991,#38992,#38993,
#38994,#38995,#38996,#38997,#38998,#38999,#39000,#39001,#39002,#39003,#39004,
#39005,#39006,#39007,#39008,#39009,#39010),.UNSPECIFIED.,.F.,.F.,(4,3,3,
3,3,3,3,4),(70.2250835898874,70.8320759578836,71.8297108305298,72.8273457031761,
73.8249805758223,74.8226154484686,75.8202503211148,76.508268897067),
 .UNSPECIFIED.);
#6156=B_SPLINE_CURVE_WITH_KNOTS('',3,(#39015,#39016,#39017,#39018,#39019,
#39020,#39021,#39022,#39023,#39024,#39025,#39026,#39027,#39028,#39029,#39030,
#39031,#39032,#39033,#39034,#39035,#39036),.UNSPECIFIED.,.F.,.F.,(4,3,3,
3,3,3,3,4),(-85.7741580335289,-84.798964174931,-83.8013293022848,-82.8036944296386,
-81.8060595569923,-80.8084246843461,-79.8107898116998,-79.4909727263494),
 .UNSPECIFIED.);
#6157=B_SPLINE_CURVE_WITH_KNOTS('',3,(#39037,#39038,#39039,#39040,#39041,
#39042,#39043,#39044,#39045,#39046,#39047,#39048,#39049,#39050,#39051,#39052,
#39053,#39054,#39055,#39056,#39057,#39058),.UNSPECIFIED.,.F.,.F.,(4,3,3,
3,3,3,3,4),(76.508268897067,76.8178851937611,77.8155200664073,78.8131549390536,
79.8107898116998,80.8084246843461,81.8060595569923,82.7914542042466),
 .UNSPECIFIED.);
#6158=B_SPLINE_CURVE_WITH_KNOTS('',3,(#39063,#39064,#39065,#39066,#39067,
#39068,#39069,#39070,#39071,#39072,#39073,#39074,#39075,#39076,#39077,#39078,
#39079,#39080,#39081,#39082,#39083,#39084,#39085,#39086,#39087),
 .UNSPECIFIED.,.F.,.F.,(4,3,3,3,3,3,3,3,4),(-92.0573433407085,-91.7824082834548,
-90.7847734108085,-89.7871385381623,-88.789503665516,-87.7918687928698,
-86.7942339202235,-85.7965990475773,-85.7741580335289),.UNSPECIFIED.);
#6159=B_SPLINE_CURVE_WITH_KNOTS('',3,(#39088,#39089,#39090,#39091,#39092,
#39093,#39094,#39095,#39096,#39097,#39098,#39099,#39100,#39101,#39102,#39103,
#39104,#39105,#39106,#39107,#39108,#39109,#39110,#39111,#39112),
 .UNSPECIFIED.,.F.,.F.,(4,3,3,3,3,3,3,3,4),(82.7914542042466,82.8036944296386,
83.8013293022848,84.7989641749311,85.7965990475773,86.7942339202236,87.7918687928698,
88.789503665516,89.0746395114262),.UNSPECIFIED.);
#6160=B_SPLINE_CURVE_WITH_KNOTS('',3,(#39117,#39118,#39119,#39120,#39121,
#39122,#39123,#39124,#39125,#39126,#39127,#39128,#39129,#39130,#39131,#39132,
#39133,#39134,#39135,#39136,#39137,#39138),.UNSPECIFIED.,.F.,.F.,(4,3,3,
3,3,3,3,4),(-98.3405286478881,-97.7682175193322,-96.770582646686,-95.7729477740397,
-94.7753129013935,-93.7776780287473,-92.780043156101,-92.0573433407085),
 .UNSPECIFIED.);
#6161=B_SPLINE_CURVE_WITH_KNOTS('',3,(#39139,#39140,#39141,#39142,#39143,
#39144,#39145,#39146,#39147,#39148,#39149,#39150,#39151,#39152,#39153,#39154,
#39155,#39156,#39157,#39158,#39159,#39160),.UNSPECIFIED.,.F.,.F.,(4,3,3,
3,3,3,3,4),(89.0746395114262,89.7871385381623,90.7847734108086,91.7824082834548,
92.780043156101,93.7776780287473,94.7753129013935,95.3578248186058),
 .UNSPECIFIED.);
#6162=B_SPLINE_CURVE_WITH_KNOTS('',3,(#39165,#39166,#39167,#39168,#39169,
#39170,#39171,#39172,#39173,#39174,#39175,#39176,#39177,#39178,#39179,#39180,
#39181,#39182,#39183,#39184,#39185,#39186),.UNSPECIFIED.,.F.,.F.,(4,3,3,
3,3,3,3,4),(-104.623713955068,-103.75402675521,-102.756391882563,-101.758757009917,
-100.761122137271,-99.7634872646247,-98.7658523919785,-98.3405286478881),
 .UNSPECIFIED.);
#6163=B_SPLINE_CURVE_WITH_KNOTS('',3,(#39187,#39188,#39189,#39190,#39191,
#39192,#39193,#39194,#39195,#39196,#39197,#39198,#39199,#39200,#39201,#39202,
#39203,#39204,#39205,#39206,#39207,#39208),.UNSPECIFIED.,.F.,.F.,(4,3,3,
3,3,3,3,4),(95.3578248186058,95.7729477740397,96.770582646686,97.7682175193323,
98.7658523919785,99.7634872646248,100.761122137271,101.641010125785),
 .UNSPECIFIED.);
#6164=B_SPLINE_CURVE_WITH_KNOTS('',3,(#39213,#39214,#39215,#39216,#39217,
#39218,#39219,#39220,#39221,#39222,#39223,#39224,#39225,#39226,#39227,#39228,
#39229,#39230,#39231,#39232,#39233,#39234,#39235,#39236,#39237),
 .UNSPECIFIED.,.F.,.F.,(4,3,3,3,3,3,3,3,4),(-110.906899262247,-110.737470863733,
-109.739835991087,-108.742201118441,-107.744566245795,-106.746931373148,
-105.749296500502,-104.751661627856,-104.623713955068),.UNSPECIFIED.);
#6165=B_SPLINE_CURVE_WITH_KNOTS('',3,(#39238,#39239,#39240,#39241,#39242,
#39243,#39244,#39245,#39246,#39247,#39248,#39249,#39250,#39251,#39252,#39253,
#39254,#39255,#39256,#39257,#39258,#39259,#39260,#39261,#39262),
 .UNSPECIFIED.,.F.,.F.,(4,3,3,3,3,3,3,3,4),(101.641010125785,101.758757009917,
102.756391882564,103.75402675521,104.751661627856,105.749296500502,106.746931373149,
107.744566245795,107.924195432965),.UNSPECIFIED.);
#6166=B_SPLINE_CURVE_WITH_KNOTS('',3,(#39267,#39268,#39269,#39270,#39271,
#39272,#39273,#39274,#39275,#39276,#39277,#39278,#39279,#39280,#39281,#39282,
#39283,#39284,#39285,#39286,#39287,#39288),.UNSPECIFIED.,.F.,.F.,(4,3,3,
3,3,3,3,4),(-117.190084569427,-116.723280099611,-115.725645226965,-114.728010354318,
-113.730375481672,-112.732740609026,-111.73510573638,-110.906899262247),
 .UNSPECIFIED.);
#6167=B_SPLINE_CURVE_WITH_KNOTS('',3,(#39289,#39290,#39291,#39292,#39293,
#39294,#39295,#39296,#39297,#39298,#39299,#39300,#39301,#39302,#39303,#39304,
#39305,#39306,#39307,#39308,#39309,#39310),.UNSPECIFIED.,.F.,.F.,(4,3,3,
3,3,3,3,4),(107.924195432965,108.742201118441,109.739835991087,110.737470863734,
111.73510573638,112.732740609026,113.730375481672,114.207380740145),
 .UNSPECIFIED.);
#6168=B_SPLINE_CURVE_WITH_KNOTS('',3,(#39315,#39316,#39317,#39318,#39319,
#39320,#39321,#39322,#39323,#39324,#39325,#39326,#39327,#39328,#39329,#39330,
#39331,#39332,#39333,#39334,#39335,#39336),.UNSPECIFIED.,.F.,.F.,(4,3,3,
3,3,3,3,4),(-123.473269876607,-122.709089335488,-121.711454462842,-120.713819590196,
-119.71618471755,-118.718549844903,-117.720914972257,-117.190084569427),
 .UNSPECIFIED.);
#6169=B_SPLINE_CURVE_WITH_KNOTS('',3,(#39337,#39338,#39339,#39340,#39341,
#39342,#39343,#39344,#39345,#39346,#39347,#39348,#39349,#39350,#39351,#39352,
#39353,#39354,#39355,#39356,#39357,#39358),.UNSPECIFIED.,.F.,.F.,(4,3,3,
3,3,3,3,4),(114.207380740145,114.728010354318,115.725645226965,116.723280099611,
117.720914972257,118.718549844904,119.71618471755,120.490566047324),
 .UNSPECIFIED.);
#6170=B_SPLINE_CURVE_WITH_KNOTS('',3,(#39363,#39364,#39365,#39366,#39367,
#39368,#39369,#39370,#39371,#39372,#39373,#39374,#39375,#39376,#39377,#39378,
#39379,#39380,#39381,#39382,#39383,#39384,#39385,#39386,#39387),
 .UNSPECIFIED.,.F.,.F.,(4,3,3,3,3,3,3,3,4),(-129.756455183786,-129.692533444012,
-128.694898571366,-127.69726369872,-126.699628826073,-125.701993953427,
-124.704359080781,-123.706724208135,-123.473269876607),.UNSPECIFIED.);
#6171=B_SPLINE_CURVE_WITH_KNOTS('',3,(#39388,#39389,#39390,#39391,#39392,
#39393,#39394,#39395,#39396,#39397,#39398,#39399,#39400,#39401,#39402,#39403,
#39404,#39405,#39406,#39407,#39408,#39409,#39410,#39411,#39412),
 .UNSPECIFIED.,.F.,.F.,(4,3,3,3,3,3,3,3,4),(120.490566047324,120.713819590196,
121.711454462842,122.709089335488,123.706724208135,124.704359080781,125.701993953427,
126.699628826073,126.773751354504),.UNSPECIFIED.);
#6172=B_SPLINE_CURVE_WITH_KNOTS('',3,(#39417,#39418,#39419,#39420,#39421,
#39422,#39423,#39424,#39425,#39426,#39427,#39428,#39429,#39430,#39431,#39432,
#39433,#39434,#39435,#39436,#39437,#39438),.UNSPECIFIED.,.F.,.F.,(4,3,3,
3,3,3,3,4),(-136.039640490966,-135.67834267989,-134.680707807243,-133.683072934597,
-132.685438061951,-131.687803189305,-130.690168316658,-129.756455183786),
 .UNSPECIFIED.);
#6173=B_SPLINE_CURVE_WITH_KNOTS('',3,(#39439,#39440,#39441,#39442,#39443,
#39444,#39445,#39446,#39447,#39448,#39449,#39450,#39451,#39452,#39453,#39454,
#39455,#39456,#39457,#39458,#39459,#39460),.UNSPECIFIED.,.F.,.F.,(4,3,3,
3,3,3,3,4),(126.773751354504,127.69726369872,128.694898571366,129.692533444012,
130.690168316658,131.687803189305,132.685438061951,133.056936661683),
 .UNSPECIFIED.);
#6174=B_SPLINE_CURVE_WITH_KNOTS('',3,(#39465,#39466,#39467,#39468,#39469,
#39470,#39471,#39472,#39473,#39474,#39475,#39476,#39477,#39478,#39479,#39480,
#39481,#39482,#39483,#39484,#39485,#39486),.UNSPECIFIED.,.F.,.F.,(4,3,3,
3,3,3,3,4),(-142.322825798145,-141.664151915767,-140.666517043121,-139.668882170475,
-138.671247297828,-137.673612425182,-136.675977552536,-136.039640490966),
 .UNSPECIFIED.);
#6175=B_SPLINE_CURVE_WITH_KNOTS('',3,(#39487,#39488,#39489,#39490,#39491,
#39492,#39493,#39494,#39495,#39496,#39497,#39498,#39499,#39500,#39501,#39502,
#39503,#39504,#39505,#39506,#39507,#39508),.UNSPECIFIED.,.F.,.F.,(4,3,3,
3,3,3,3,4),(133.056936661683,133.683072934597,134.680707807244,135.67834267989,
136.675977552536,137.673612425182,138.671247297829,139.340121968863),
 .UNSPECIFIED.);
#6176=B_SPLINE_CURVE_WITH_KNOTS('',3,(#39513,#39514,#39515,#39516,#39517,
#39518,#39519,#39520,#39521,#39522,#39523,#39524,#39525,#39526,#39527,#39528,
#39529,#39530,#39531,#39532,#39533,#39534),.UNSPECIFIED.,.F.,.F.,(4,3,3,
3,3,3,3,4),(-148.606011105325,-147.649961151645,-146.652326278998,-145.654691406352,
-144.657056533706,-143.65942166106,-142.661786788413,-142.322825798145),
 .UNSPECIFIED.);
#6177=B_SPLINE_CURVE_WITH_KNOTS('',3,(#39535,#39536,#39537,#39538,#39539,
#39540,#39541,#39542,#39543,#39544,#39545,#39546,#39547,#39548,#39549,#39550,
#39551,#39552,#39553,#39554,#39555,#39556),.UNSPECIFIED.,.F.,.F.,(4,3,3,
3,3,3,3,4),(139.340121968863,139.668882170475,140.666517043121,141.664151915767,
142.661786788413,143.65942166106,144.657056533706,145.623307276042),
 .UNSPECIFIED.);
#6178=B_SPLINE_CURVE_WITH_KNOTS('',3,(#39561,#39562,#39563,#39564,#39565,
#39566,#39567,#39568,#39569,#39570,#39571,#39572,#39573,#39574,#39575,#39576,
#39577,#39578,#39579,#39580,#39581,#39582,#39583,#39584,#39585),
 .UNSPECIFIED.,.F.,.F.,(4,3,3,3,3,3,3,3,4),(-154.889196412504,-154.633405260168,
-153.635770387522,-152.638135514876,-151.64050064223,-150.642865769583,
-149.645230896937,-148.647596024291,-148.606011105325),.UNSPECIFIED.);
#6179=B_SPLINE_CURVE_WITH_KNOTS('',3,(#39586,#39587,#39588,#39589,#39590,
#39591,#39592,#39593,#39594,#39595,#39596,#39597,#39598,#39599,#39600,#39601,
#39602,#39603,#39604,#39605,#39606,#39607,#39608,#39609,#39610),
 .UNSPECIFIED.,.F.,.F.,(4,3,3,3,3,3,3,3,4),(145.623307276042,145.654691406352,
146.652326278998,147.649961151645,148.647596024291,149.645230896937,150.642865769583,
151.64050064223,151.906492583222),.UNSPECIFIED.);
#6180=B_SPLINE_CURVE_WITH_KNOTS('',3,(#39615,#39616,#39617,#39618,#39619,
#39620,#39621,#39622,#39623,#39624,#39625,#39626,#39627,#39628,#39629,#39630,
#39631,#39632,#39633,#39634,#39635,#39636),.UNSPECIFIED.,.F.,.F.,(4,3,3,
3,3,3,3,4),(-161.172381719684,-160.619214496046,-159.6215796234,-158.623944750753,
-157.626309878107,-156.628675005461,-155.631040132815,-154.889196412504),
 .UNSPECIFIED.);
#6181=B_SPLINE_CURVE_WITH_KNOTS('',3,(#39637,#39638,#39639,#39640,#39641,
#39642,#39643,#39644,#39645,#39646,#39647,#39648,#39649,#39650,#39651,#39652,
#39653,#39654,#39655,#39656,#39657,#39658),.UNSPECIFIED.,.F.,.F.,(4,3,3,
3,3,3,3,4),(151.906492583222,152.638135514876,153.635770387522,154.633405260168,
155.631040132815,156.628675005461,157.626309878107,158.189677890402),
 .UNSPECIFIED.);
#6182=B_SPLINE_CURVE_WITH_KNOTS('',3,(#39663,#39664,#39665,#39666,#39667,
#39668,#39669,#39670,#39671,#39672,#39673,#39674,#39675,#39676,#39677,#39678,
#39679,#39680,#39681,#39682,#39683,#39684),.UNSPECIFIED.,.F.,.F.,(4,3,3,
3,3,3,3,4),(-167.455567026863,-166.605023731923,-165.607388859277,-164.609753986631,
-163.612119113985,-162.614484241338,-161.616849368692,-161.172381719684),
 .UNSPECIFIED.);
#6183=B_SPLINE_CURVE_WITH_KNOTS('',3,(#39685,#39686,#39687,#39688,#39689,
#39690,#39691,#39692,#39693,#39694,#39695,#39696,#39697,#39698,#39699,#39700,
#39701,#39702,#39703,#39704,#39705,#39706),.UNSPECIFIED.,.F.,.F.,(4,3,3,
3,3,3,3,4),(158.189677890402,158.623944750753,159.6215796234,160.619214496046,
161.616849368692,162.614484241338,163.612119113985,164.472863197581),
 .UNSPECIFIED.);
#6184=B_SPLINE_CURVE_WITH_KNOTS('',3,(#39711,#39712,#39713,#39714,#39715,
#39716,#39717,#39718,#39719,#39720,#39721,#39722,#39723,#39724,#39725,#39726,
#39727,#39728,#39729,#39730,#39731,#39732,#39733,#39734,#39735),
 .UNSPECIFIED.,.F.,.F.,(4,3,3,3,3,3,3,3,4),(-173.738752334043,-173.588467840447,
-172.590832967801,-171.593198095155,-170.595563222508,-169.597928349862,
-168.600293477216,-167.60265860457,-167.455567026863),.UNSPECIFIED.);
#6185=B_SPLINE_CURVE_WITH_KNOTS('',3,(#39736,#39737,#39738,#39739,#39740,
#39741,#39742,#39743,#39744,#39745,#39746,#39747,#39748,#39749,#39750,#39751,
#39752,#39753,#39754,#39755,#39756,#39757,#39758,#39759,#39760),
 .UNSPECIFIED.,.F.,.F.,(4,3,3,3,3,3,3,3,4),(164.472863197581,164.609753986631,
165.607388859277,166.605023731923,167.60265860457,168.600293477216,169.597928349862,
170.595563222508,170.756048504761),.UNSPECIFIED.);
#6186=B_SPLINE_CURVE_WITH_KNOTS('',3,(#39765,#39766,#39767,#39768,#39769,
#39770,#39771,#39772,#39773,#39774,#39775,#39776,#39777,#39778,#39779,#39780,
#39781,#39782,#39783,#39784,#39785,#39786),.UNSPECIFIED.,.F.,.F.,(4,3,3,
3,3,3,3,4),(-180.021937641223,-179.574277076325,-178.576642203678,-177.579007331032,
-176.581372458386,-175.58373758574,-174.586102713093,-173.738752334043),
 .UNSPECIFIED.);
#6187=B_SPLINE_CURVE_WITH_KNOTS('',3,(#39787,#39788,#39789,#39790,#39791,
#39792,#39793,#39794,#39795,#39796,#39797,#39798,#39799,#39800,#39801,#39802,
#39803,#39804,#39805,#39806,#39807,#39808),.UNSPECIFIED.,.F.,.F.,(4,3,3,
3,3,3,3,4),(170.756048504761,171.593198095155,172.590832967801,173.588467840447,
174.586102713093,175.58373758574,176.581372458386,177.03923381194),
 .UNSPECIFIED.);
#6188=B_SPLINE_CURVE_WITH_KNOTS('',3,(#39813,#39814,#39815,#39816,#39817,
#39818,#39819,#39820,#39821,#39822,#39823,#39824,#39825,#39826,#39827,#39828,
#39829,#39830,#39831,#39832,#39833,#39834),.UNSPECIFIED.,.F.,.F.,(4,3,3,
3,3,3,3,4),(-186.305122948402,-185.560086312202,-184.562451439556,-183.56481656691,
-182.567181694263,-181.569546821617,-180.571911948971,-180.021937641223),
 .UNSPECIFIED.);
#6189=B_SPLINE_CURVE_WITH_KNOTS('',3,(#39835,#39836,#39837,#39838,#39839,
#39840,#39841,#39842,#39843,#39844,#39845,#39846,#39847,#39848,#39849,#39850,
#39851,#39852,#39853,#39854,#39855,#39856),.UNSPECIFIED.,.F.,.F.,(4,3,3,
3,3,3,3,4),(177.03923381194,177.579007331032,178.576642203678,179.574277076325,
180.571911948971,181.569546821617,182.567181694263,183.32241911912),
 .UNSPECIFIED.);
#6190=B_SPLINE_CURVE_WITH_KNOTS('',3,(#39861,#39862,#39863,#39864,#39865,
#39866,#39867,#39868,#39869,#39870,#39871,#39872,#39873,#39874,#39875,#39876,
#39877,#39878,#39879,#39880,#39881,#39882,#39883,#39884,#39885),
 .UNSPECIFIED.,.F.,.F.,(4,3,3,3,3,3,3,3,4),(-192.588308255582,-192.543530420726,
-191.545895548079,-190.548260675433,-189.550625802787,-188.552990930141,
-187.555356057495,-186.557721184848,-186.305122948402),.UNSPECIFIED.);
#6191=B_SPLINE_CURVE_WITH_KNOTS('',3,(#39886,#39887,#39888,#39889,#39890,
#39891,#39892,#39893,#39894,#39895,#39896,#39897,#39898,#39899,#39900,#39901,
#39902,#39903,#39904,#39905,#39906,#39907,#39908,#39909,#39910),
 .UNSPECIFIED.,.F.,.F.,(4,3,3,3,3,3,3,3,4),(183.32241911912,183.56481656691,
184.562451439556,185.560086312202,186.557721184848,187.555356057495,188.552990930141,
189.550625802787,189.605604426299),.UNSPECIFIED.);
#6192=B_SPLINE_CURVE_WITH_KNOTS('',3,(#39915,#39916,#39917,#39918,#39919,
#39920,#39921,#39922,#39923,#39924,#39925,#39926,#39927,#39928,#39929,#39930,
#39931,#39932,#39933,#39934,#39935,#39936),.UNSPECIFIED.,.F.,.F.,(4,3,3,
3,3,3,3,4),(-198.871493562761,-198.529339656603,-197.531704783957,-196.534069911311,
-195.536435038664,-194.538800166018,-193.541165293372,-192.588308255582),
 .UNSPECIFIED.);
#6193=B_SPLINE_CURVE_WITH_KNOTS('',3,(#39937,#39938,#39939,#39940,#39941,
#39942,#39943,#39944,#39945,#39946,#39947,#39948,#39949,#39950,#39951,#39952,
#39953,#39954,#39955,#39956,#39957,#39958),.UNSPECIFIED.,.F.,.F.,(4,3,3,
3,3,3,3,4),(189.605604426299,190.548260675433,191.54589554808,192.543530420726,
193.541165293372,194.538800166018,195.536435038665,195.888789733479),
 .UNSPECIFIED.);
#6194=B_SPLINE_CURVE_WITH_KNOTS('',3,(#39963,#39964,#39965,#39966,#39967,
#39968,#39969,#39970,#39971,#39972,#39973,#39974,#39975,#39976,#39977,#39978,
#39979,#39980,#39981,#39982,#39983,#39984),.UNSPECIFIED.,.F.,.F.,(4,3,3,
3,3,3,3,4),(-205.154678869941,-204.515148892481,-203.517514019834,-202.519879147188,
-201.522244274542,-200.524609401896,-199.526974529249,-198.871493562761),
 .UNSPECIFIED.);
#6195=B_SPLINE_CURVE_WITH_KNOTS('',3,(#39985,#39986,#39987,#39988,#39989,
#39990,#39991,#39992,#39993,#39994,#39995,#39996,#39997,#39998,#39999,#40000,
#40001,#40002,#40003,#40004,#40005,#40006),.UNSPECIFIED.,.F.,.F.,(4,3,3,
3,3,3,3,4),(195.888789733479,196.534069911311,197.531704783957,198.529339656603,
199.52697452925,200.524609401896,201.522244274542,202.171975040659),
 .UNSPECIFIED.);
#6196=B_SPLINE_CURVE_WITH_KNOTS('',3,(#40011,#40012,#40013,#40014,#40015,
#40016,#40017,#40018,#40019,#40020,#40021,#40022,#40023,#40024,#40025,#40026,
#40027,#40028,#40029,#40030,#40031,#40032),.UNSPECIFIED.,.F.,.F.,(4,3,3,
3,3,3,3,4),(-211.43786417712,-210.500958128358,-209.503323255712,-208.505688383066,
-207.50805351042,-206.510418637773,-205.512783765127,-205.154678869941),
 .UNSPECIFIED.);
#6197=B_SPLINE_CURVE_WITH_KNOTS('',3,(#40033,#40034,#40035,#40036,#40037,
#40038,#40039,#40040,#40041,#40042,#40043,#40044,#40045,#40046,#40047,#40048,
#40049,#40050,#40051,#40052,#40053,#40054),.UNSPECIFIED.,.F.,.F.,(4,3,3,
3,3,3,3,4),(202.171975040659,202.519879147188,203.517514019835,204.515148892481,
205.512783765127,206.510418637773,207.50805351042,208.455160347838),
 .UNSPECIFIED.);
#6198=B_SPLINE_CURVE_WITH_KNOTS('',3,(#40059,#40060,#40061,#40062,#40063,
#40064,#40065,#40066,#40067,#40068,#40069,#40070,#40071,#40072,#40073,#40074,
#40075,#40076,#40077,#40078,#40079,#40080,#40081,#40082,#40083),
 .UNSPECIFIED.,.F.,.F.,(4,3,3,3,3,3,3,3,4),(-217.7210494843,-217.484402236882,
-216.486767364236,-215.489132491589,-214.491497618943,-213.493862746297,
-212.496227873651,-211.498593001004,-211.43786417712),.UNSPECIFIED.);
#6199=B_SPLINE_CURVE_WITH_KNOTS('',3,(#40084,#40085,#40086,#40087,#40088,
#40089,#40090,#40091,#40092,#40093,#40094,#40095,#40096,#40097,#40098,#40099,
#40100,#40101,#40102,#40103,#40104,#40105,#40106,#40107,#40108),
 .UNSPECIFIED.,.F.,.F.,(4,3,3,3,3,3,3,3,4),(208.455160347838,208.505688383066,
209.503323255712,210.500958128358,211.498593001005,212.496227873651,213.493862746297,
214.491497618943,214.738345655018),.UNSPECIFIED.);
#6200=B_SPLINE_CURVE_WITH_KNOTS('',3,(#40113,#40114,#40115,#40116,#40117,
#40118,#40119,#40120,#40121,#40122,#40123,#40124,#40125,#40126,#40127,#40128,
#40129,#40130,#40131,#40132,#40133,#40134),.UNSPECIFIED.,.F.,.F.,(4,3,3,
3,3,3,3,4),(-224.00423479148,-223.470211472759,-222.472576600113,-221.474941727467,
-220.477306854821,-219.479671982174,-218.482037109528,-217.7210494843),
 .UNSPECIFIED.);
#6201=B_SPLINE_CURVE_WITH_KNOTS('',3,(#40135,#40136,#40137,#40138,#40139,
#40140,#40141,#40142,#40143,#40144,#40145,#40146,#40147,#40148,#40149,#40150,
#40151,#40152,#40153,#40154,#40155,#40156),.UNSPECIFIED.,.F.,.F.,(4,3,3,
3,3,3,3,4),(214.738345655018,215.48913249159,216.486767364236,217.484402236882,
218.482037109528,219.479671982175,220.477306854821,221.021530962197),
 .UNSPECIFIED.);
#6202=B_SPLINE_CURVE_WITH_KNOTS('',3,(#40161,#40162,#40163,#40164,#40165,
#40166,#40167,#40168,#40169,#40170,#40171,#40172,#40173,#40174,#40175,#40176,
#40177,#40178,#40179,#40180,#40181,#40182),.UNSPECIFIED.,.F.,.F.,(4,3,3,
3,3,3,3,4),(-230.287420098659,-229.456020708637,-228.458385835991,-227.460750963344,
-226.463116090698,-225.465481218052,-224.467846345406,-224.00423479148),
 .UNSPECIFIED.);
#6203=B_SPLINE_CURVE_WITH_KNOTS('',3,(#40183,#40184,#40185,#40186,#40187,
#40188,#40189,#40190,#40191,#40192,#40193,#40194,#40195,#40196,#40197,#40198,
#40199,#40200,#40201,#40202,#40203,#40204),.UNSPECIFIED.,.F.,.F.,(4,3,3,
3,3,3,3,4),(221.021530962197,221.474941727467,222.472576600113,223.47021147276,
224.467846345406,225.465481218052,226.463116090698,227.304716269377),
 .UNSPECIFIED.);
#6204=B_SPLINE_CURVE_WITH_KNOTS('',3,(#40209,#40210,#40211,#40212,#40213,
#40214,#40215,#40216,#40217,#40218,#40219,#40220,#40221,#40222,#40223,#40224,
#40225,#40226,#40227,#40228,#40229,#40230,#40231,#40232,#40233),
 .UNSPECIFIED.,.F.,.F.,(4,3,3,3,3,3,3,3,4),(-236.570605405839,-236.439464817161,
-235.441829944514,-234.444195071868,-233.446560199222,-232.448925326576,
-231.451290453929,-230.453655581283,-230.287420098659),.UNSPECIFIED.);
#6205=B_SPLINE_CURVE_WITH_KNOTS('',3,(#40234,#40235,#40236,#40237,#40238,
#40239,#40240,#40241,#40242,#40243,#40244,#40245,#40246,#40247,#40248,#40249,
#40250,#40251,#40252,#40253,#40254,#40255,#40256,#40257,#40258),
 .UNSPECIFIED.,.F.,.F.,(4,3,3,3,3,3,3,3,4),(227.304716269377,227.460750963345,
228.458385835991,229.456020708637,230.453655581283,231.451290453929,232.448925326576,
233.446560199222,233.587901576556),.UNSPECIFIED.);
#6206=B_SPLINE_CURVE_WITH_KNOTS('',3,(#40263,#40264,#40265,#40266,#40267,
#40268,#40269,#40270,#40271,#40272,#40273,#40274,#40275,#40276,#40277,#40278,
#40279,#40280,#40281,#40282,#40283,#40284),.UNSPECIFIED.,.F.,.F.,(4,3,3,
3,3,3,3,4),(-242.853790713018,-242.425274053038,-241.427639180392,-240.430004307746,
-239.432369435099,-238.434734562453,-237.437099689807,-236.570605405839),
 .UNSPECIFIED.);
#6207=B_SPLINE_CURVE_WITH_KNOTS('',3,(#40285,#40286,#40287,#40288,#40289,
#40290,#40291,#40292,#40293,#40294,#40295,#40296,#40297,#40298,#40299,#40300,
#40301,#40302,#40303,#40304,#40305,#40306),.UNSPECIFIED.,.F.,.F.,(4,3,3,
3,3,3,3,4),(233.587901576556,234.444195071868,235.441829944515,236.439464817161,
237.437099689807,238.434734562453,239.432369435099,239.871086883736),
 .UNSPECIFIED.);
#6208=B_SPLINE_CURVE_WITH_KNOTS('',3,(#40311,#40312,#40313,#40314,#40315,
#40316,#40317,#40318,#40319,#40320,#40321,#40322,#40323,#40324,#40325,#40326,
#40327,#40328,#40329,#40330,#40331,#40332),.UNSPECIFIED.,.F.,.F.,(4,3,3,
3,3,3,3,4),(-249.136976020198,-248.411083288916,-247.413448416269,-246.415813543623,
-245.418178670977,-244.420543798331,-243.422908925684,-242.853790713018),
 .UNSPECIFIED.);
#6209=B_SPLINE_CURVE_WITH_KNOTS('',3,(#40333,#40334,#40335,#40336,#40337,
#40338,#40339,#40340,#40341,#40342,#40343,#40344,#40345,#40346,#40347,#40348,
#40349,#40350,#40351,#40352,#40353,#40354),.UNSPECIFIED.,.F.,.F.,(4,3,3,
3,3,3,3,4),(239.871086883736,240.430004307746,241.427639180392,242.425274053038,
243.422908925684,244.420543798331,245.418178670977,246.154272190915),
 .UNSPECIFIED.);
#6210=B_SPLINE_CURVE_WITH_KNOTS('',3,(#40359,#40360,#40361,#40362,#40363,
#40364,#40365,#40366,#40367,#40368,#40369,#40370,#40371,#40372,#40373,#40374,
#40375,#40376,#40377,#40378,#40379,#40380,#40381,#40382,#40383),
 .UNSPECIFIED.,.F.,.F.,(4,3,3,3,3,3,3,3,4),(-255.420161327377,-255.394527397439,
-254.396892524793,-253.399257652147,-252.401622779501,-251.403987906854,
-250.406353034208,-249.408718161562,-249.136976020198),.UNSPECIFIED.);
#6211=B_SPLINE_CURVE_WITH_KNOTS('',3,(#40384,#40385,#40386,#40387,#40388,
#40389,#40390,#40391,#40392,#40393,#40394,#40395,#40396,#40397,#40398,#40399,
#40400,#40401,#40402,#40403,#40404,#40405,#40406,#40407,#40408),
 .UNSPECIFIED.,.F.,.F.,(4,3,3,3,3,3,3,3,4),(246.154272190915,246.415813543623,
247.41344841627,248.411083288916,249.408718161562,250.406353034208,251.403987906854,
252.401622779501,252.437457498095),.UNSPECIFIED.);
#6212=B_SPLINE_CURVE_WITH_KNOTS('',3,(#40413,#40414,#40415,#40416,#40417,
#40418,#40419,#40420,#40421,#40422,#40423,#40424,#40425,#40426,#40427,#40428,
#40429,#40430,#40431,#40432,#40433,#40434),.UNSPECIFIED.,.F.,.F.,(4,3,3,
3,3,3,3,4),(-261.703346634557,-261.380336633317,-260.382701760671,-259.385066888024,
-258.387432015378,-257.389797142732,-256.392162270086,-255.420161327377),
 .UNSPECIFIED.);
#6213=B_SPLINE_CURVE_WITH_KNOTS('',3,(#40435,#40436,#40437,#40438,#40439,
#40440,#40441,#40442,#40443,#40444,#40445,#40446,#40447,#40448,#40449,#40450,
#40451,#40452,#40453,#40454,#40455,#40456),.UNSPECIFIED.,.F.,.F.,(4,3,3,
3,3,3,3,4),(252.437457498095,253.399257652147,254.396892524793,255.394527397439,
256.392162270086,257.389797142732,258.387432015378,258.720642805275),
 .UNSPECIFIED.);
#6214=B_SPLINE_CURVE_WITH_KNOTS('',3,(#40461,#40462,#40463,#40464,#40465,
#40466,#40467,#40468,#40469,#40470,#40471,#40472,#40473,#40474,#40475,#40476,
#40477,#40478,#40479,#40480,#40481,#40482),.UNSPECIFIED.,.F.,.F.,(4,3,3,
3,3,3,3,4),(-267.986531941737,-267.366145869194,-266.368510996548,-265.370876123902,
-264.373241251256,-263.375606378609,-262.377971505963,-261.703346634557),
 .UNSPECIFIED.);
#6215=B_SPLINE_CURVE_WITH_KNOTS('',3,(#40483,#40484,#40485,#40486,#40487,
#40488,#40489,#40490,#40491,#40492,#40493,#40494,#40495,#40496,#40497,#40498,
#40499,#40500,#40501,#40502,#40503,#40504),.UNSPECIFIED.,.F.,.F.,(4,3,3,
3,3,3,3,4),(258.720642805275,259.385066888024,260.382701760671,261.380336633317,
262.377971505963,263.375606378609,264.373241251256,265.003828112454),
 .UNSPECIFIED.);
#6216=B_SPLINE_CURVE_WITH_KNOTS('',3,(#40509,#40510,#40511,#40512,#40513,
#40514,#40515,#40516,#40517,#40518,#40519,#40520,#40521,#40522,#40523,#40524,
#40525,#40526,#40527,#40528,#40529,#40530),.UNSPECIFIED.,.F.,.F.,(4,3,3,
3,3,3,3,4),(-274.269717248916,-273.351955105072,-272.354320232426,-271.356685359779,
-270.359050487133,-269.361415614487,-268.363780741841,-267.986531941737),
 .UNSPECIFIED.);
#6217=B_SPLINE_CURVE_WITH_KNOTS('',3,(#40531,#40532,#40533,#40534,#40535,
#40536,#40537,#40538,#40539,#40540,#40541,#40542,#40543,#40544,#40545,#40546,
#40547,#40548,#40549,#40550,#40551,#40552),.UNSPECIFIED.,.F.,.F.,(4,3,3,
3,3,3,3,4),(265.003828112454,265.370876123902,266.368510996548,267.366145869194,
268.363780741841,269.361415614487,270.359050487133,271.287013419634),
 .UNSPECIFIED.);
#6218=B_SPLINE_CURVE_WITH_KNOTS('',3,(#40558,#40559,#40560,#40561),
 .UNSPECIFIED.,.F.,.F.,(4,4),(285.884931476671,285.89887235325),
 .UNSPECIFIED.);
#6219=B_SPLINE_CURVE_WITH_KNOTS('',3,(#40567,#40568,#40569,#40570,#40571,
#40572,#40573,#40574,#40575,#40576),.UNSPECIFIED.,.F.,.F.,(4,1,1,1,1,1,
1,4),(279.601746169491,279.978994969596,280.976629842242,281.974264714888,
282.971899587534,283.969534460181,284.967169332827,285.884931476671),
 .UNSPECIFIED.);
#6220=B_SPLINE_CURVE_WITH_KNOTS('',3,(#40579,#40580,#40581,#40582,#40583,
#40584,#40585,#40586,#40587),.UNSPECIFIED.,.F.,.F.,(4,1,1,1,1,1,4),(279.601746169492,
279.671418109638,280.669052982284,281.66668785493,282.664322727577,283.661957600223,
284.659592472869),.UNSPECIFIED.);
#6221=B_SPLINE_CURVE_WITH_KNOTS('',3,(#40592,#40593,#40594,#40595,#40596,
#40597,#40598,#40599,#40600,#40601),.UNSPECIFIED.,.F.,.F.,(4,1,1,1,1,1,
1,4),(273.318560862312,273.993185733718,274.990820606364,275.988455479011,
276.986090351657,277.983725224303,278.981360096949,279.601746169491),
 .UNSPECIFIED.);
#6222=B_SPLINE_CURVE_WITH_KNOTS('',3,(#40602,#40603,#40604,#40605,#40606,
#40607,#40608,#40609,#40610,#40611),.UNSPECIFIED.,.F.,.F.,(4,1,1,1,1,1,
1,4),(273.318560862312,273.68560887376,274.683243746407,275.680878619053,
276.678513491699,277.676148364345,278.673783236992,279.601746169492),
 .UNSPECIFIED.);
#6223=B_SPLINE_CURVE_WITH_KNOTS('',3,(#40616,#40617,#40618,#40619,#40620,
#40621,#40622,#40623,#40624,#40625),.UNSPECIFIED.,.F.,.F.,(4,1,1,1,1,1,
1,4),(267.035375555132,268.007376497841,269.005011370487,270.002646243133,
271.000281115779,271.997915988426,272.995550861072,273.318560862312),
 .UNSPECIFIED.);
#6224=B_SPLINE_CURVE_WITH_KNOTS('',3,(#40626,#40627,#40628,#40629,#40630,
#40631,#40632,#40633,#40634,#40635),.UNSPECIFIED.,.F.,.F.,(4,1,1,1,1,1,
1,4),(267.035375555132,267.699799637883,268.697434510529,269.695069383175,
270.692704255822,271.690339128468,272.687974001114,273.318560862312),
 .UNSPECIFIED.);
#6225=B_SPLINE_CURVE_WITH_KNOTS('',3,(#40640,#40641,#40642,#40643,#40644,
#40645,#40646,#40647,#40648,#40649,#40650),.UNSPECIFIED.,.F.,.F.,(4,1,1,
1,1,1,1,1,4),(260.752190247953,261.023932389317,262.021567261963,263.019202134609,
264.016837007256,265.014471879902,266.012106752548,267.009741625194,267.035375555132),
 .UNSPECIFIED.);
#6226=B_SPLINE_CURVE_WITH_KNOTS('',3,(#40651,#40652,#40653,#40654,#40655,
#40656,#40657,#40658,#40659,#40660),.UNSPECIFIED.,.F.,.F.,(4,1,1,1,1,1,
1,4),(260.752190247953,261.713990402005,262.711625274652,263.709260147298,
264.706895019944,265.70452989259,266.702164765237,267.035375555132),
 .UNSPECIFIED.);
#6227=B_SPLINE_CURVE_WITH_KNOTS('',3,(#40665,#40666,#40667,#40668,#40669,
#40670,#40671,#40672,#40673,#40674),.UNSPECIFIED.,.F.,.F.,(4,1,1,1,1,1,
1,4),(254.469004940773,255.038123153439,256.035758026086,257.033392898732,
258.031027771378,259.028662644024,260.026297516671,260.752190247953),
 .UNSPECIFIED.);
#6228=B_SPLINE_CURVE_WITH_KNOTS('',3,(#40675,#40676,#40677,#40678,#40679,
#40680,#40681,#40682,#40683,#40684,#40685),.UNSPECIFIED.,.F.,.F.,(4,1,1,
1,1,1,1,1,4),(254.469004940773,254.730546293482,255.728181166128,256.725816038774,
257.72345091142,258.721085784067,259.718720656713,260.716355529359,260.752190247953),
 .UNSPECIFIED.);
#6229=B_SPLINE_CURVE_WITH_KNOTS('',3,(#40690,#40691,#40692,#40693,#40694,
#40695,#40696,#40697,#40698,#40699),.UNSPECIFIED.,.F.,.F.,(4,1,1,1,1,1,
1,4),(248.185819633594,249.052313917562,250.049948790208,251.047583662854,
252.045218535501,253.042853408147,254.040488280793,254.469004940773),
 .UNSPECIFIED.);
#6230=B_SPLINE_CURVE_WITH_KNOTS('',3,(#40700,#40701,#40702,#40703,#40704,
#40705,#40706,#40707,#40708,#40709),.UNSPECIFIED.,.F.,.F.,(4,1,1,1,1,1,
1,4),(248.185819633594,248.744737057604,249.74237193025,250.740006802897,
251.737641675543,252.735276548189,253.732911420835,254.469004940773),
 .UNSPECIFIED.);
#6231=B_SPLINE_CURVE_WITH_KNOTS('',3,(#40714,#40715,#40716,#40717,#40718,
#40719,#40720,#40721,#40722,#40723,#40724),.UNSPECIFIED.,.F.,.F.,(4,1,1,
1,1,1,1,1,4),(241.902634326414,242.068869809038,243.066504681685,244.064139554331,
245.061774426977,246.059409299623,247.05704417227,248.054679044916,248.185819633594),
 .UNSPECIFIED.);
#6232=B_SPLINE_CURVE_WITH_KNOTS('',3,(#40725,#40726,#40727,#40728,#40729,
#40730,#40731,#40732,#40733,#40734),.UNSPECIFIED.,.F.,.F.,(4,1,1,1,1,1,
1,4),(241.902634326414,242.758927821727,243.756562694373,244.754197567019,
245.751832439665,246.749467312312,247.747102184958,248.185819633594),
 .UNSPECIFIED.);
#6233=B_SPLINE_CURVE_WITH_KNOTS('',3,(#40739,#40740,#40741,#40742,#40743,
#40744,#40745,#40746,#40747,#40748),.UNSPECIFIED.,.F.,.F.,(4,1,1,1,1,1,
1,4),(235.619449019234,236.083060573161,237.080695445807,238.078330318453,
239.0759651911,240.073600063746,241.071234936392,241.902634326414),
 .UNSPECIFIED.);
#6234=B_SPLINE_CURVE_WITH_KNOTS('',3,(#40749,#40750,#40751,#40752,#40753,
#40754,#40755,#40756,#40757,#40758,#40759),.UNSPECIFIED.,.F.,.F.,(4,1,1,
1,1,1,1,1,4),(235.619449019235,235.775483713203,236.773118585849,237.770753458495,
238.768388331142,239.766023203788,240.763658076434,241.76129294908,241.902634326414),
 .UNSPECIFIED.);
#6235=B_SPLINE_CURVE_WITH_KNOTS('',3,(#40764,#40765,#40766,#40767,#40768,
#40769,#40770,#40771,#40772,#40773),.UNSPECIFIED.,.F.,.F.,(4,1,1,1,1,1,
1,4),(229.336263712055,230.097251337283,231.09488620993,232.092521082576,
233.090155955222,234.087790827868,235.085425700515,235.619449019234),
 .UNSPECIFIED.);
#6236=B_SPLINE_CURVE_WITH_KNOTS('',3,(#40774,#40775,#40776,#40777,#40778,
#40779,#40780,#40781,#40782,#40783),.UNSPECIFIED.,.F.,.F.,(4,1,1,1,1,1,
1,4),(229.336263712055,229.789674477325,230.787309349972,231.784944222618,
232.782579095264,233.78021396791,234.777848840557,235.619449019235),
 .UNSPECIFIED.);
#6237=B_SPLINE_CURVE_WITH_KNOTS('',3,(#40788,#40789,#40790,#40791,#40792,
#40793,#40794,#40795,#40796,#40797,#40798),.UNSPECIFIED.,.F.,.F.,(4,1,1,
1,1,1,1,1,4),(223.053078404875,223.11380722876,224.111442101406,225.109076974052,
226.106711846698,227.104346719345,228.101981591991,229.099616464637,229.336263712055),
 .UNSPECIFIED.);
#6238=B_SPLINE_CURVE_WITH_KNOTS('',3,(#40799,#40800,#40801,#40802,#40803,
#40804,#40805,#40806,#40807,#40808),.UNSPECIFIED.,.F.,.F.,(4,1,1,1,1,1,
1,4),(223.053078404876,223.803865241448,224.801500114094,225.79913498674,
226.796769859387,227.794404732033,228.792039604679,229.336263712055),
 .UNSPECIFIED.);
#6239=B_SPLINE_CURVE_WITH_KNOTS('',3,(#40813,#40814,#40815,#40816,#40817,
#40818,#40819,#40820,#40821,#40822),.UNSPECIFIED.,.F.,.F.,(4,1,1,1,1,1,
1,4),(216.769893097696,217.127997992882,218.125632865528,219.123267738175,
220.120902610821,221.118537483467,222.116172356113,223.053078404875),
 .UNSPECIFIED.);
#6240=B_SPLINE_CURVE_WITH_KNOTS('',3,(#40823,#40824,#40825,#40826,#40827,
#40828,#40829,#40830,#40831,#40832,#40833),.UNSPECIFIED.,.F.,.F.,(4,1,1,
1,1,1,1,1,4),(216.769893097696,216.820421132924,217.81805600557,218.815690878217,
219.813325750863,220.810960623509,221.808595496155,222.806230368802,223.053078404876),
 .UNSPECIFIED.);
#6241=B_SPLINE_CURVE_WITH_KNOTS('',3,(#40838,#40839,#40840,#40841,#40842,
#40843,#40844,#40845,#40846,#40847),.UNSPECIFIED.,.F.,.F.,(4,1,1,1,1,1,
1,4),(210.486707790516,211.142188757005,212.139823629651,213.137458502297,
214.135093374943,215.13272824759,216.130363120236,216.769893097696),
 .UNSPECIFIED.);
#6242=B_SPLINE_CURVE_WITH_KNOTS('',3,(#40848,#40849,#40850,#40851,#40852,
#40853,#40854,#40855,#40856,#40857),.UNSPECIFIED.,.F.,.F.,(4,1,1,1,1,1,
1,4),(210.486707790516,210.834611897047,211.832246769693,212.829881642339,
213.827516514985,214.825151387632,215.822786260278,216.769893097696),
 .UNSPECIFIED.);
#6243=B_SPLINE_CURVE_WITH_KNOTS('',3,(#40862,#40863,#40864,#40865,#40866,
#40867,#40868,#40869,#40870,#40871),.UNSPECIFIED.,.F.,.F.,(4,1,1,1,1,1,
1,4),(204.203522483337,205.156379521127,206.154014393773,207.15164926642,
208.149284139066,209.146919011712,210.144553884358,210.486707790516),
 .UNSPECIFIED.);
#6244=B_SPLINE_CURVE_WITH_KNOTS('',3,(#40872,#40873,#40874,#40875,#40876,
#40877,#40878,#40879,#40880,#40881),.UNSPECIFIED.,.F.,.F.,(4,1,1,1,1,1,
1,4),(204.203522483337,204.848802661169,205.846437533815,206.844072406462,
207.841707279108,208.839342151754,209.8369770244,210.486707790516),
 .UNSPECIFIED.);
#6245=B_SPLINE_CURVE_WITH_KNOTS('',3,(#40886,#40887,#40888,#40889,#40890,
#40891,#40892,#40893,#40894,#40895,#40896),.UNSPECIFIED.,.F.,.F.,(4,1,1,
1,1,1,1,1,4),(197.920337176157,198.172935412603,199.17057028525,200.168205157896,
201.165840030542,202.163474903188,203.161109775835,204.158744648481,204.203522483337),
 .UNSPECIFIED.);
#6246=B_SPLINE_CURVE_WITH_KNOTS('',3,(#40897,#40898,#40899,#40900,#40901,
#40902,#40903,#40904,#40905,#40906),.UNSPECIFIED.,.F.,.F.,(4,1,1,1,1,1,
1,4),(197.920337176157,198.862993425292,199.860628297938,200.858263170584,
201.85589804323,202.853532915877,203.851167788523,204.203522483337),
 .UNSPECIFIED.);
#6247=B_SPLINE_CURVE_WITH_KNOTS('',3,(#40911,#40912,#40913,#40914,#40915,
#40916,#40917,#40918,#40919,#40920),.UNSPECIFIED.,.F.,.F.,(4,1,1,1,1,1,
1,4),(191.637151868978,192.187126176726,193.184761049372,194.182395922018,
195.180030794665,196.177665667311,197.175300539957,197.920337176157),
 .UNSPECIFIED.);
#6248=B_SPLINE_CURVE_WITH_KNOTS('',3,(#40921,#40922,#40923,#40924,#40925,
#40926,#40927,#40928,#40929,#40930,#40931),.UNSPECIFIED.,.F.,.F.,(4,1,1,
1,1,1,1,1,4),(191.637151868978,191.879549316768,192.877184189414,193.87481906206,
194.872453934707,195.870088807353,196.867723679999,197.865358552645,197.920337176157),
 .UNSPECIFIED.);
#6249=B_SPLINE_CURVE_WITH_KNOTS('',3,(#40936,#40937,#40938,#40939,#40940,
#40941,#40942,#40943,#40944,#40945),.UNSPECIFIED.,.F.,.F.,(4,1,1,1,1,1,
1,4),(185.353966561798,186.201316940848,187.198951813495,188.196586686141,
189.194221558787,190.191856431433,191.18949130408,191.637151868978),
 .UNSPECIFIED.);
#6250=B_SPLINE_CURVE_WITH_KNOTS('',3,(#40946,#40947,#40948,#40949,#40950,
#40951,#40952,#40953,#40954,#40955),.UNSPECIFIED.,.F.,.F.,(4,1,1,1,1,1,
1,4),(185.353966561798,185.89374008089,186.891374953537,187.889009826183,
188.886644698829,189.884279571475,190.881914444122,191.637151868978),
 .UNSPECIFIED.);
#6251=B_SPLINE_CURVE_WITH_KNOTS('',3,(#40960,#40961,#40962,#40963,#40964,
#40965,#40966,#40967,#40968,#40969,#40970),.UNSPECIFIED.,.F.,.F.,(4,1,1,
1,1,1,1,1,4),(179.070781254618,179.217872832325,180.215507704971,181.213142577617,
182.210777450263,183.20841232291,184.206047195556,185.203682068202,185.353966561798),
 .UNSPECIFIED.);
#6252=B_SPLINE_CURVE_WITH_KNOTS('',3,(#40971,#40972,#40973,#40974,#40975,
#40976,#40977,#40978,#40979,#40980),.UNSPECIFIED.,.F.,.F.,(4,1,1,1,1,1,
1,4),(179.070781254619,179.907930845013,180.905565717659,181.903200590305,
182.900835462952,183.898470335598,184.896105208244,185.353966561798),
 .UNSPECIFIED.);
#6253=B_SPLINE_CURVE_WITH_KNOTS('',3,(#40985,#40986,#40987,#40988,#40989,
#40990,#40991,#40992,#40993,#40994),.UNSPECIFIED.,.F.,.F.,(4,1,1,1,1,1,
1,4),(172.787595947439,173.232063596447,174.229698469093,175.22733334174,
176.224968214386,177.222603087032,178.220237959678,179.070781254618),
 .UNSPECIFIED.);
#6254=B_SPLINE_CURVE_WITH_KNOTS('',3,(#40995,#40996,#40997,#40998,#40999,
#41000,#41001,#41002,#41003,#41004,#41005),.UNSPECIFIED.,.F.,.F.,(4,1,1,
1,1,1,1,1,4),(172.787595947439,172.924486736489,173.922121609136,174.919756481782,
175.917391354428,176.915026227074,177.912661099721,178.910295972367,179.070781254619),
 .UNSPECIFIED.);
#6255=B_SPLINE_CURVE_WITH_KNOTS('',3,(#41010,#41011,#41012,#41013,#41014,
#41015,#41016,#41017,#41018,#41019),.UNSPECIFIED.,.F.,.F.,(4,1,1,1,1,1,
1,4),(166.504410640259,167.24625436057,168.243889233216,169.241524105862,
170.239158978508,171.236793851155,172.234428723801,172.787595947439),
 .UNSPECIFIED.);
#6256=B_SPLINE_CURVE_WITH_KNOTS('',3,(#41020,#41021,#41022,#41023,#41024,
#41025,#41026,#41027,#41028,#41029),.UNSPECIFIED.,.F.,.F.,(4,1,1,1,1,1,
1,4),(166.504410640259,166.938677500612,167.936312373258,168.933947245904,
169.931582118551,170.929216991197,171.926851863843,172.787595947439),
 .UNSPECIFIED.);
#6257=B_SPLINE_CURVE_WITH_KNOTS('',3,(#41034,#41035,#41036,#41037,#41038,
#41039,#41040,#41041,#41042,#41043,#41044),.UNSPECIFIED.,.F.,.F.,(4,1,1,
1,1,1,1,1,4),(160.22122533308,160.262810252046,161.260445124692,162.258079997338,
163.255714869985,164.253349742631,165.250984615277,166.248619487923,166.504410640259),
 .UNSPECIFIED.);
#6258=B_SPLINE_CURVE_WITH_KNOTS('',3,(#41045,#41046,#41047,#41048,#41049,
#41050,#41051,#41052,#41053,#41054),.UNSPECIFIED.,.F.,.F.,(4,1,1,1,1,1,
1,4),(160.22122533308,160.952868264734,161.950503137381,162.948138010027,
163.945772882673,164.943407755319,165.941042627966,166.504410640259),
 .UNSPECIFIED.);
#6259=B_SPLINE_CURVE_WITH_KNOTS('',3,(#41059,#41060,#41061,#41062,#41063,
#41064,#41065,#41066,#41067,#41068),.UNSPECIFIED.,.F.,.F.,(4,1,1,1,1,1,
1,4),(153.9380400259,154.277001016168,155.274635888815,156.272270761461,
157.269905634107,158.267540506754,159.2651753794,160.22122533308),
 .UNSPECIFIED.);
#6260=B_SPLINE_CURVE_WITH_KNOTS('',3,(#41069,#41070,#41071,#41072,#41073,
#41074,#41075,#41076,#41077,#41078,#41079),.UNSPECIFIED.,.F.,.F.,(4,1,1,
1,1,1,1,1,4),(153.9380400259,153.969424156211,154.967059028857,155.964693901503,
156.962328774149,157.959963646796,158.957598519442,159.955233392088,160.22122533308),
 .UNSPECIFIED.);
#6261=B_SPLINE_CURVE_WITH_KNOTS('',3,(#41084,#41085,#41086,#41087,#41088,
#41089,#41090,#41091,#41092,#41093),.UNSPECIFIED.,.F.,.F.,(4,1,1,1,1,1,
1,4),(147.654854718721,148.291191780291,149.288826652937,150.286461525584,
151.28409639823,152.281731270876,153.279366143522,153.9380400259),
 .UNSPECIFIED.);
#6262=B_SPLINE_CURVE_WITH_KNOTS('',3,(#41094,#41095,#41096,#41097,#41098,
#41099,#41100,#41101,#41102,#41103),.UNSPECIFIED.,.F.,.F.,(4,1,1,1,1,1,
1,4),(147.654854718721,147.983614920333,148.981249792979,149.978884665626,
150.976519538272,151.974154410918,152.971789283564,153.9380400259),
 .UNSPECIFIED.);
#6263=B_SPLINE_CURVE_WITH_KNOTS('',3,(#41108,#41109,#41110,#41111,#41112,
#41113,#41114,#41115,#41116,#41117),.UNSPECIFIED.,.F.,.F.,(4,1,1,1,1,1,
1,4),(141.371669411541,142.305382544414,143.30301741706,144.300652289706,
145.298287162352,146.295922034999,147.293556907645,147.654854718721),
 .UNSPECIFIED.);
#6264=B_SPLINE_CURVE_WITH_KNOTS('',3,(#41118,#41119,#41120,#41121,#41122,
#41123,#41124,#41125,#41126,#41127),.UNSPECIFIED.,.F.,.F.,(4,1,1,1,1,1,
1,4),(141.371669411541,141.997805684456,142.995440557102,143.993075429748,
144.990710302394,145.988345175041,146.985980047687,147.654854718721),
 .UNSPECIFIED.);
#6265=B_SPLINE_CURVE_WITH_KNOTS('',3,(#41132,#41133,#41134,#41135,#41136,
#41137,#41138,#41139,#41140,#41141,#41142),.UNSPECIFIED.,.F.,.F.,(4,1,1,
1,1,1,1,1,4),(135.088484104361,135.32193843589,136.319573308536,137.317208181182,
138.314843053829,139.312477926475,140.310112799121,141.307747671767,141.371669411541),
 .UNSPECIFIED.);
#6266=B_SPLINE_CURVE_WITH_KNOTS('',3,(#41143,#41144,#41145,#41146,#41147,
#41148,#41149,#41150,#41151,#41152),.UNSPECIFIED.,.F.,.F.,(4,1,1,1,1,1,
1,4),(135.088484104362,136.011996448578,137.009631321224,138.007266193871,
139.004901066517,140.002535939163,141.000170811809,141.371669411541),
 .UNSPECIFIED.);
#6267=B_SPLINE_CURVE_WITH_KNOTS('',3,(#41157,#41158,#41159,#41160,#41161,
#41162,#41163,#41164,#41165,#41166),.UNSPECIFIED.,.F.,.F.,(4,1,1,1,1,1,
1,4),(128.805298797182,129.336129200012,130.333764072659,131.331398945305,
132.329033817951,133.326668690597,134.324303563244,135.088484104361),
 .UNSPECIFIED.);
#6268=B_SPLINE_CURVE_WITH_KNOTS('',3,(#41167,#41168,#41169,#41170,#41171,
#41172,#41173,#41174,#41175,#41176,#41177),.UNSPECIFIED.,.F.,.F.,(4,1,1,
1,1,1,1,1,4),(128.805298797182,129.028552340054,130.026187212701,131.023822085347,
132.021456957993,133.019091830639,134.016726703286,135.014361575932,135.088484104362),
 .UNSPECIFIED.);
#6269=B_SPLINE_CURVE_WITH_KNOTS('',3,(#41182,#41183,#41184,#41185,#41186,
#41187,#41188,#41189,#41190,#41191),.UNSPECIFIED.,.F.,.F.,(4,1,1,1,1,1,
1,4),(122.522113490002,123.350319964135,124.347954836781,125.345589709427,
126.343224582074,127.34085945472,128.338494327366,128.805298797182),
 .UNSPECIFIED.);
#6270=B_SPLINE_CURVE_WITH_KNOTS('',3,(#41192,#41193,#41194,#41195,#41196,
#41197,#41198,#41199,#41200,#41201),.UNSPECIFIED.,.F.,.F.,(4,1,1,1,1,1,
1,4),(122.522113490002,123.042743104177,124.040377976823,125.038012849469,
126.035647722116,127.033282594762,128.030917467408,128.805298797182),
 .UNSPECIFIED.);
#6271=B_SPLINE_CURVE_WITH_KNOTS('',3,(#41206,#41207,#41208,#41209,#41210,
#41211,#41212,#41213,#41214,#41215,#41216),.UNSPECIFIED.,.F.,.F.,(4,1,1,
1,1,1,1,1,4),(116.238928182823,116.366875855611,117.364510728257,118.362145600904,
119.35978047355,120.357415346196,121.355050218842,122.352685091489,122.522113490002),
 .UNSPECIFIED.);
#6272=B_SPLINE_CURVE_WITH_KNOTS('',3,(#41217,#41218,#41219,#41220,#41221,
#41222,#41223,#41224,#41225,#41226),.UNSPECIFIED.,.F.,.F.,(4,1,1,1,1,1,
1,4),(116.238928182823,117.056933868299,118.054568740946,119.052203613592,
120.049838486238,121.047473358884,122.045108231531,122.522113490002),
 .UNSPECIFIED.);
#6273=B_SPLINE_CURVE_WITH_KNOTS('',3,(#41231,#41232,#41233,#41234,#41235,
#41236,#41237,#41238,#41239,#41240),.UNSPECIFIED.,.F.,.F.,(4,1,1,1,1,1,
1,4),(109.955742875643,110.381066619734,111.37870149238,112.376336365026,
113.373971237672,114.371606110319,115.369240982965,116.238928182823),
 .UNSPECIFIED.);
#6274=B_SPLINE_CURVE_WITH_KNOTS('',3,(#41241,#41242,#41243,#41244,#41245,
#41246,#41247,#41248,#41249,#41250,#41251),.UNSPECIFIED.,.F.,.F.,(4,1,1,
1,1,1,1,1,4),(109.955742875643,110.073489759776,111.071124632422,112.068759505068,
113.066394377714,114.064029250361,115.061664123007,116.059298995653,116.238928182823),
 .UNSPECIFIED.);
#6275=B_SPLINE_CURVE_WITH_KNOTS('',3,(#41256,#41257,#41258,#41259,#41260,
#41261,#41262,#41263,#41264,#41265),.UNSPECIFIED.,.F.,.F.,(4,1,1,1,1,1,
1,4),(103.672557568464,104.395257383856,105.392892256502,106.390527129149,
107.388162001795,108.385796874441,109.383431747087,109.955742875643),
 .UNSPECIFIED.);
#6276=B_SPLINE_CURVE_WITH_KNOTS('',3,(#41266,#41267,#41268,#41269,#41270,
#41271,#41272,#41273,#41274,#41275),.UNSPECIFIED.,.F.,.F.,(4,1,1,1,1,1,
1,4),(103.672557568464,104.087680523898,105.085315396544,106.082950269191,
107.080585141837,108.078220014483,109.075854887129,109.955742875643),
 .UNSPECIFIED.);
#6277=B_SPLINE_CURVE_WITH_KNOTS('',3,(#41280,#41281,#41282,#41283,#41284,
#41285,#41286,#41287,#41288,#41289,#41290),.UNSPECIFIED.,.F.,.F.,(4,1,1,
1,1,1,1,1,4),(97.389372261284,97.4118132753324,98.4094481479786,99.4070830206249,
100.404717893271,101.402352765917,102.399987638564,103.39762251121,103.672557568464),
 .UNSPECIFIED.);
#6278=B_SPLINE_CURVE_WITH_KNOTS('',3,(#41291,#41292,#41293,#41294,#41295,
#41296,#41297,#41298,#41299,#41300),.UNSPECIFIED.,.F.,.F.,(4,1,1,1,1,1,
1,4),(97.3893722612841,98.1018712880207,99.0995061606669,100.097141033313,
101.094775905959,102.092410778606,103.090045651252,103.672557568464),
 .UNSPECIFIED.);
#6279=B_SPLINE_CURVE_WITH_KNOTS('',3,(#41305,#41306,#41307,#41308,#41309,
#41310,#41311,#41312,#41313,#41314),.UNSPECIFIED.,.F.,.F.,(4,1,1,1,1,1,
1,4),(91.1061869541044,91.4260040394549,92.4236389121012,93.4212737847474,
94.4189086573937,95.4165435300399,96.4141784026861,97.389372261284),
 .UNSPECIFIED.);
#6280=B_SPLINE_CURVE_WITH_KNOTS('',3,(#41315,#41316,#41317,#41318,#41319,
#41320,#41321,#41322,#41323,#41324,#41325),.UNSPECIFIED.,.F.,.F.,(4,1,1,
1,1,1,1,1,4),(91.1061869541045,91.1184271794969,92.1160620521432,93.1136969247894,
94.1113317974357,95.1089666700819,96.1066015427282,97.1042364153744,97.3893722612841),
 .UNSPECIFIED.);
#6281=B_SPLINE_CURVE_WITH_KNOTS('',3,(#41330,#41331,#41332,#41333,#41334,
#41335,#41336,#41337,#41338,#41339),.UNSPECIFIED.,.F.,.F.,(4,1,1,1,1,1,
1,4),(84.8230016469248,85.4401948035774,86.4378296762237,87.4354645488699,
88.4330994215162,89.4307342941624,90.4283691668087,91.1061869541044),
 .UNSPECIFIED.);
#6282=B_SPLINE_CURVE_WITH_KNOTS('',3,(#41340,#41341,#41342,#41343,#41344,
#41345,#41346,#41347,#41348,#41349),.UNSPECIFIED.,.F.,.F.,(4,1,1,1,1,1,
1,4),(84.8230016469249,85.1326179436194,86.1302528162657,87.1278876889119,
88.1255225615582,89.1231574342044,90.1207923068507,91.1061869541045),
 .UNSPECIFIED.);
#6283=B_SPLINE_CURVE_WITH_KNOTS('',3,(#41354,#41355,#41356,#41357,#41358,
#41359,#41360,#41361,#41362,#41363),.UNSPECIFIED.,.F.,.F.,(4,1,1,1,1,1,
1,4),(78.5398163397452,79.4543855676999,80.4520204403462,81.4496553129924,
82.4472901856387,83.4449250582849,84.4425599309312,84.8230016469248),
 .UNSPECIFIED.);
#6284=B_SPLINE_CURVE_WITH_KNOTS('',3,(#41364,#41365,#41366,#41367,#41368,
#41369,#41370,#41371,#41372,#41373),.UNSPECIFIED.,.F.,.F.,(4,1,1,1,1,1,
1,4),(78.5398163397453,79.146808707742,80.1444435803882,81.1420784530345,
82.1397133256807,83.1373481983269,84.1349830709732,84.8230016469249),
 .UNSPECIFIED.);
#6285=B_SPLINE_CURVE_WITH_KNOTS('',3,(#41378,#41379,#41380,#41381,#41382,
#41383,#41384,#41385,#41386,#41387,#41388),.UNSPECIFIED.,.F.,.F.,(4,1,1,
1,1,1,1,1,4),(72.2566310325656,72.4709414591762,73.4685763318225,74.4662112044687,
75.463846077115,76.4614809497612,77.4591158224074,78.4567506950537,78.5398163397452),
 .UNSPECIFIED.);
#6286=B_SPLINE_CURVE_WITH_KNOTS('',3,(#41389,#41390,#41391,#41392,#41393,
#41394,#41395,#41396,#41397,#41398),.UNSPECIFIED.,.F.,.F.,(4,1,1,1,1,1,
1,4),(72.2566310325657,73.1609994718645,74.1586343445107,75.156269217157,
76.1539040898032,77.1515389624495,78.1491738350957,78.5398163397453),
 .UNSPECIFIED.);
#6287=B_SPLINE_CURVE_WITH_KNOTS('',3,(#41403,#41404,#41405,#41406,#41407,
#41408,#41409,#41410,#41411,#41412),.UNSPECIFIED.,.F.,.F.,(4,1,1,1,1,1,
1,4),(65.973445725386,66.4851322232987,67.482767095945,68.4804019685912,
69.4780368412375,70.4756717138837,71.47330658653,72.2566310325656),
 .UNSPECIFIED.);
#6288=B_SPLINE_CURVE_WITH_KNOTS('',3,(#41413,#41414,#41415,#41416,#41417,
#41418,#41419,#41420,#41421,#41422,#41423),.UNSPECIFIED.,.F.,.F.,(4,1,1,
1,1,1,1,1,4),(65.9734457253861,66.1775553633407,67.175190235987,68.1728251086332,
69.1704599812795,70.1680948539257,71.165729726572,72.1633645992182,72.2566310325657),
 .UNSPECIFIED.);
#6289=B_SPLINE_CURVE_WITH_KNOTS('',3,(#41428,#41429,#41430,#41431,#41432,
#41433,#41434,#41435,#41436,#41437),.UNSPECIFIED.,.F.,.F.,(4,1,1,1,1,1,
1,4),(59.6902604182064,60.4993229874212,61.4969578600675,62.4945927327137,
63.49222760536,64.4898624780062,65.4874973506525,65.973445725386),
 .UNSPECIFIED.);
#6290=B_SPLINE_CURVE_WITH_KNOTS('',3,(#41438,#41439,#41440,#41441,#41442,
#41443,#41444,#41445,#41446,#41447),.UNSPECIFIED.,.F.,.F.,(4,1,1,1,1,1,
1,4),(59.6902604182065,60.1917461274632,61.1893810001095,62.1870158727557,
63.184650745402,64.1822856180482,65.1799204906945,65.9734457253861),
 .UNSPECIFIED.);
#6291=B_SPLINE_CURVE_WITH_KNOTS('',3,(#41452,#41453,#41454,#41455,#41456,
#41457,#41458,#41459,#41460,#41461,#41462),.UNSPECIFIED.,.F.,.F.,(4,1,1,
1,1,1,1,1,4),(53.4070751110268,53.5158788788975,54.5135137515438,55.51114862419,
56.5087834968363,57.5064183694825,58.5040532421287,59.501688114775,59.6902604182064),
 .UNSPECIFIED.);
#6292=B_SPLINE_CURVE_WITH_KNOTS('',3,(#41463,#41464,#41465,#41466,#41467,
#41468,#41469,#41470,#41471,#41472),.UNSPECIFIED.,.F.,.F.,(4,1,1,1,1,1,
1,4),(53.4070751110269,54.2059368915858,55.203571764232,56.2012066368783,
57.1988415095245,58.1964763821708,59.194111254817,59.6902604182065),
 .UNSPECIFIED.);
#6293=B_SPLINE_CURVE_WITH_KNOTS('',3,(#41477,#41478,#41479,#41480,#41481,
#41482,#41483,#41484,#41485,#41486),.UNSPECIFIED.,.F.,.F.,(4,1,1,1,1,1,
1,4),(47.1238898038472,47.53006964302,48.5277045156663,49.5253393883125,
50.5229742609588,51.520609133605,52.5182440062513,53.4070751110268),
 .UNSPECIFIED.);
#6294=B_SPLINE_CURVE_WITH_KNOTS('',3,(#41487,#41488,#41489,#41490,#41491,
#41492,#41493,#41494,#41495,#41496,#41497),.UNSPECIFIED.,.F.,.F.,(4,1,1,
1,1,1,1,1,4),(47.1238898038473,47.222492783062,48.2201276557083,49.2177625283545,
50.2153974010008,51.213032273647,52.2106671462933,53.2083020189395,53.4070751110269),
 .UNSPECIFIED.);
#6295=B_SPLINE_CURVE_WITH_KNOTS('',3,(#41502,#41503,#41504,#41505,#41506,
#41507,#41508,#41509,#41510,#41511),.UNSPECIFIED.,.F.,.F.,(4,1,1,1,1,1,
1,4),(40.8407044966676,41.5442604071425,42.5418952797888,43.539530152435,
44.5371650250813,45.5347998977275,46.5324347703738,47.1238898038472),
 .UNSPECIFIED.);
#6296=B_SPLINE_CURVE_WITH_KNOTS('',3,(#41512,#41513,#41514,#41515,#41516,
#41517,#41518,#41519,#41520,#41521),.UNSPECIFIED.,.F.,.F.,(4,1,1,1,1,1,
1,4),(40.8407044966677,41.2366835471845,42.2343184198308,43.231953292477,
44.2295881651233,45.2272230377695,46.2248579104158,47.1238898038473),
 .UNSPECIFIED.);
#6297=B_SPLINE_CURVE_WITH_KNOTS('',3,(#41526,#41527,#41528,#41529,#41530,
#41531,#41532,#41533,#41534,#41535,#41536),.UNSPECIFIED.,.F.,.F.,(4,1,1,
1,1,1,1,1,4),(34.557519189488,34.5608162986188,35.5584511712651,36.5560860439113,
37.5537209165576,38.5513557892038,39.54899066185,40.5466255344963,40.8407044966676),
 .UNSPECIFIED.);
#6298=B_SPLINE_CURVE_WITH_KNOTS('',3,(#41537,#41538,#41539,#41540,#41541,
#41542,#41543,#41544,#41545,#41546),.UNSPECIFIED.,.F.,.F.,(4,1,1,1,1,1,
1,4),(34.5575191894882,35.2508743113071,36.2485091839533,37.2461440565995,
38.2437789292458,39.241413801892,40.2390486745383,40.8407044966677),
 .UNSPECIFIED.);
#6299=B_SPLINE_CURVE_WITH_KNOTS('',3,(#41551,#41552,#41553,#41554,#41555,
#41556,#41557,#41558,#41559,#41560),.UNSPECIFIED.,.F.,.F.,(4,1,1,1,1,1,
1,4),(28.2743338823084,28.5750070627413,29.5726419353876,30.5702768080338,
31.5679116806801,32.5655465533263,33.5631814259726,34.557519189488),
 .UNSPECIFIED.);
#6300=B_SPLINE_CURVE_WITH_KNOTS('',3,(#41561,#41562,#41563,#41564,#41565,
#41566,#41567,#41568,#41569,#41570),.UNSPECIFIED.,.F.,.F.,(4,1,1,1,1,1,
1,4),(28.2743338823086,29.2650650754296,30.2626999480758,31.2603348207221,
32.2579696933683,33.2556045660146,34.2532394386608,34.5575191894882),
 .UNSPECIFIED.);
#6301=B_SPLINE_CURVE_WITH_KNOTS('',3,(#41575,#41576,#41577,#41578,#41579,
#41580,#41581,#41582,#41583,#41584),.UNSPECIFIED.,.F.,.F.,(4,1,1,1,1,1,
1,4),(21.9911485751289,22.5891978268638,23.5868326995101,24.5844675721563,
25.5821024448026,26.5797373174488,27.5773721900951,28.2743338823084),
 .UNSPECIFIED.);
#6302=B_SPLINE_CURVE_WITH_KNOTS('',3,(#41585,#41586,#41587,#41588,#41589,
#41590,#41591,#41592,#41593,#41594,#41595),.UNSPECIFIED.,.F.,.F.,(4,1,1,
1,1,1,1,1,4),(21.991148575129,22.2816209669058,23.2792558395521,24.2768907121983,
25.2745255848446,26.2721604574908,27.2697953301371,28.2674302027833,28.2743338823086),
 .UNSPECIFIED.);
#6303=B_SPLINE_CURVE_WITH_KNOTS('',3,(#41600,#41601,#41602,#41603,#41604,
#41605,#41606,#41607,#41608,#41609),.UNSPECIFIED.,.F.,.F.,(4,1,1,1,1,1,
1,4),(15.7079632679493,16.6033885909864,17.6010234636326,18.5986583362789,
19.5962932089251,20.5939280815713,21.5915629542176,21.9911485751289),
 .UNSPECIFIED.);
#6304=B_SPLINE_CURVE_WITH_KNOTS('',3,(#41610,#41611,#41612,#41613,#41614,
#41615,#41616,#41617,#41618,#41619),.UNSPECIFIED.,.F.,.F.,(4,1,1,1,1,1,
1,4),(15.7079632679494,16.2958117310283,17.2934466036746,18.2910814763208,
19.2887163489671,20.2863512216133,21.2839860942596,21.991148575129),
 .UNSPECIFIED.);
#6305=B_SPLINE_CURVE_WITH_KNOTS('',3,(#42741,#42742,#42743,#42744,#42745,
#42746,#42747,#42748,#42749,#42750,#42751,#42752,#42753,#42754,#42755,#42756,
#42757,#42758,#42759,#42760,#42761,#42762,#42763,#42764,#42765,#42766,#42767,
#42768,#42769,#42770,#42771,#42772,#42773,#42774,#42775,#42776,#42777,#42778,
#42779,#42780,#42781,#42782,#42783,#42784,#42785,#42786,#42787,#42788,#42789,
#42790,#42791,#42792,#42793,#42794,#42795,#42796,#42797,#42798,#42799,#42800,
#42801,#42802,#42803,#42804,#42805,#42806,#42807,#42808,#42809,#42810,#42811,
#42812,#42813,#42814,#42815,#42816,#42817,#42818,#42819,#42820,#42821,#42822,
#42823,#42824,#42825,#42826,#42827,#42828,#42829,#42830,#42831,#42832,#42833,
#42834,#42835,#42836,#42837),.UNSPECIFIED.,.F.,.F.,(4,3,3,3,3,3,3,3,3,3,
3,3,3,3,3,3,3,3,3,3,3,3,3,3,3,3,3,3,3,3,3,3,4),(-0.741270768406308,-0.715387510784636,
-0.678846032931345,-0.657738243517773,-0.643316797175534,-0.635862900512505,
-0.599020213237717,-0.566782861872277,-0.552679020649897,-0.544234280993646,
-0.537662343230828,-0.502261333851186,-0.467119578216044,-0.433015993298668,
-0.41004234555255,-0.398746749984718,-0.393744789683524,-0.360135524847538,
-0.341121402314197,-0.306853456049999,-0.272440609283236,-0.261693001887453,
-0.257007819058798,-0.223577420294793,-0.190116876212526,-0.157068650315129,
-0.137435069025738,-0.130957629949228,-0.124458872839733,-0.0922450955809254,
-0.0604778109814689,-0.0296903572576096,0.),.UNSPECIFIED.);
#6306=B_SPLINE_CURVE_WITH_KNOTS('',3,(#42838,#42839,#42840,#42841,#42842,
#42843,#42844,#42845,#42846,#42847,#42848,#42849,#42850),.UNSPECIFIED.,
 .F.,.F.,(4,3,3,3,4),(271.287013419634,271.356685359779,272.354320232426,
273.351955105072,274.283658125495),.UNSPECIFIED.);
#6307=B_SPLINE_CURVE_WITH_KNOTS('',3,(#42852,#42853,#42854,#42855,#42856,
#42857,#42858,#42859,#42860,#42861,#42862,#42863,#42864,#42865,#42866,#42867,
#42868,#42869,#42870,#42871,#42872,#42873,#42874,#42875,#42876,#42877,#42878,
#42879,#42880,#42881,#42882,#42883,#42884,#42885,#42886,#42887,#42888,#42889,
#42890,#42891,#42892,#42893,#42894,#42895,#42896,#42897,#42898,#42899,#42900,
#42901,#42902,#42903,#42904,#42905,#42906,#42907,#42908,#42909,#42910,#42911,
#42912,#42913,#42914,#42915,#42916,#42917,#42918,#42919,#42920,#42921,#42922,
#42923,#42924,#42925,#42926,#42927,#42928,#42929,#42930,#42931,#42932,#42933,
#42934,#42935,#42936,#42937,#42938,#42939,#42940,#42941,#42942,#42943,#42944,
#42945,#42946,#42947,#42948,#42949,#42950,#42951),.UNSPECIFIED.,.F.,.F.,
(4,3,3,3,3,3,3,3,3,3,3,3,3,3,3,3,3,3,3,3,3,3,3,3,3,3,3,3,3,3,3,3,3,4),(-0.744397949170561,
-0.722857348546835,-0.691759636347062,-0.672173659622073,-0.659729697581051,
-0.653647223896304,-0.621623974301131,-0.591218978606893,-0.57779191421541,
-0.572099067158539,-0.566376890083838,-0.532985059609366,-0.499081457463265,
-0.465285106585306,-0.443559832125787,-0.437180479628824,-0.432790863135699,
-0.397876458807638,-0.378384008747229,-0.344662910041584,-0.31030331663291,
-0.299192426024121,-0.292592230277462,-0.2581831131989,-0.222669619455726,
-0.186825819848632,-0.163472592367553,-0.155670996352624,-0.150810522246808,
-0.145703618645708,-0.108961989561893,-0.0721598384238253,-0.0360557370617284,
0.),.UNSPECIFIED.);
#6308=B_SPLINE_CURVE_WITH_KNOTS('',3,(#42952,#42953,#42954,#42955,#42956,
#42957,#42958,#42959,#42960),.UNSPECIFIED.,.F.,.F.,(4,1,1,1,1,1,4),(10.3759343473742,
11.3076373677971,12.3052722404433,13.3029071130896,14.3005419857358,15.2981768583821,
15.7079632679494),.UNSPECIFIED.);
#6309=B_SPLINE_CURVE_WITH_KNOTS('',3,(#42966,#42967,#42968,#42969,#42970,
#42971,#42972,#42973,#42974,#42975,#42976,#42977,#42978,#42979,#42980,#42981,
#42982,#42983,#42984,#42985,#42986,#42987,#42988,#42989,#42990,#42991,#42992,
#42993,#42994,#42995,#42996,#42997,#42998,#42999,#43000,#43001,#43002,#43003,
#43004,#43005,#43006,#43007,#43008,#43009,#43010,#43011,#43012,#43013,#43014,
#43015,#43016,#43017,#43018,#43019,#43020,#43021,#43022,#43023,#43024,#43025,
#43026,#43027,#43028,#43029,#43030,#43031,#43032,#43033,#43034,#43035,#43036,
#43037,#43038,#43039,#43040,#43041,#43042,#43043,#43044,#43045,#43046,#43047,
#43048,#43049,#43050,#43051,#43052,#43053,#43054,#43055,#43056,#43057,#43058,
#43059,#43060,#43061,#43062),.UNSPECIFIED.,.F.,.F.,(4,3,3,3,3,3,3,3,3,3,
3,3,3,3,3,3,3,3,3,3,3,3,3,3,3,3,3,3,3,3,3,3,4),(-0.741270768406415,-0.715387510784742,
-0.678846032311912,-0.657738242937057,-0.643316795555802,-0.635862898961111,
-0.599020211880251,-0.566782860684498,-0.552679019536357,-0.544234276107367,
-0.537662341481398,-0.502261331512692,-0.46711957209537,-0.433015977083203,
-0.41004233339096,-0.398746728953922,-0.39374478606441,-0.360135513608645,
-0.341121402314231,-0.306853450668917,-0.272440605048863,-0.261692995236242,
-0.257007812571432,-0.223577410634224,-0.190116869812972,-0.157068653419064,
-0.137435071741681,-0.13095764083796,-0.124458872072335,-0.0922451026976537,
-0.0604778299681871,-0.029690391740758,0.),.UNSPECIFIED.);
#6310=B_SPLINE_CURVE_WITH_KNOTS('',3,(#43065,#43066,#43067,#43068,#43069,
#43070,#43071,#43072),.UNSPECIFIED.,.F.,.F.,(4,1,1,1,1,4),(11.6152142277551,
12.6128491004014,13.6104839730476,14.6081188456939,15.6057537183401,15.7079632679493),
 .UNSPECIFIED.);
#6311=B_SPLINE_CURVE_WITH_KNOTS('',3,(#44194,#44195,#44196,#44197,#44198,
#44199,#44200,#44201,#44202,#44203,#44204,#44205,#44206,#44207,#44208,#44209,
#44210,#44211,#44212,#44213,#44214,#44215,#44216,#44217,#44218,#44219,#44220,
#44221,#44222,#44223,#44224,#44225,#44226,#44227,#44228,#44229,#44230,#44231,
#44232,#44233,#44234,#44235,#44236,#44237,#44238,#44239,#44240,#44241,#44242,
#44243,#44244,#44245,#44246,#44247,#44248,#44249,#44250,#44251,#44252,#44253,
#44254,#44255,#44256,#44257,#44258,#44259,#44260,#44261,#44262,#44263,#44264,
#44265,#44266,#44267,#44268,#44269,#44270,#44271,#44272,#44273,#44274,#44275,
#44276,#44277,#44278,#44279,#44280,#44281,#44282,#44283,#44284,#44285,#44286,
#44287,#44288,#44289,#44290,#44291,#44292,#44293),.UNSPECIFIED.,.F.,.F.,
(4,3,3,3,3,3,3,3,3,3,3,3,3,3,3,3,3,3,3,3,3,3,3,3,3,3,3,3,3,3,3,3,3,4),(-0.744397949170713,
-0.722857348547031,-0.691759626910421,-0.672173650775227,-0.659729685964857,
-0.653647221772012,-0.621623964078995,-0.591218969662536,-0.577791899653599,
-0.57209901896209,-0.566376879451804,-0.532985044276137,-0.499081441064884,
-0.465285090294045,-0.443559819907365,-0.437180447783716,-0.432790799375827,
-0.39787639550394,-0.378384008747325,-0.344662906100098,-0.310303308027255,
-0.299192413474635,-0.29259223086673,-0.25818311008637,-0.222669611795312,
-0.186825810288309,-0.163472584002271,-0.155670981000362,-0.150810518391116,
-0.145703618285079,-0.108961986661821,-0.072159837380098,-0.0360557472806876,
0.),.UNSPECIFIED.);
#6312=B_SPLINE_CURVE_WITH_KNOTS('',3,(#44294,#44295,#44296,#44297,#44298,
#44299,#44300,#44301,#44302,#44303),.UNSPECIFIED.,.F.,.F.,(4,3,3,4),(-276.344859723011,
-275.347224850364,-274.349589977718,-274.269717248916),.UNSPECIFIED.);
#6313=B_SPLINE_CURVE_WITH_KNOTS('',3,(#44375,#44376,#44377,#44378,#44379,
#44380,#44381,#44382,#44383,#44384),.UNSPECIFIED.,.F.,.F.,(4,3,3,4),(-4.09274904019427,
-3.99858960751474,-2.99894220563605,-2.06120159751581),.UNSPECIFIED.);
#6314=B_SPLINE_CURVE_WITH_KNOTS('',3,(#44387,#44388,#44389,#44390,#44391,
#44392,#44393),.UNSPECIFIED.,.F.,.F.,(4,3,4),(0.,0.999647401878707,1.1100452109132),
 .UNSPECIFIED.);
#6315=B_SPLINE_CURVE_WITH_KNOTS('',3,(#44398,#44399,#44400,#44401,#44402,
#44403,#44404,#44405,#44406,#44407,#44408,#44409,#44410,#44411,#44412,#44413,
#44414,#44415,#44416,#44417,#44418,#44419),.UNSPECIFIED.,.F.,.F.,(4,3,3,
3,3,3,3,4),(-10.3759343473739,-9.99647401878684,-8.99682661690816,-7.99717921502947,
-6.99753181315079,-5.9978844112721,-4.99823700939342,-4.09274904019427),
 .UNSPECIFIED.);
#6316=B_SPLINE_CURVE_WITH_KNOTS('',3,(#44420,#44421,#44422,#44423,#44424,
#44425,#44426,#44427,#44428,#44429,#44430,#44431,#44432,#44433,#44434,#44435,
#44436,#44437,#44438,#44439,#44440,#44441),.UNSPECIFIED.,.F.,.F.,(4,3,3,
3,3,3,3,4),(1.1100452109132,1.9992948037574,2.99894220563608,3.99858960751477,
4.99823700939346,5.99788441127215,6.99753181315084,7.39323051809279),
 .UNSPECIFIED.);
#6317=B_SPLINE_CURVE_WITH_KNOTS('',3,(#44446,#44447,#44448,#44449,#44450,
#44451,#44452,#44453,#44454,#44455,#44456,#44457,#44458,#44459,#44460,#44461,
#44462,#44463,#44464,#44465,#44466,#44467),.UNSPECIFIED.,.F.,.F.,(4,3,3,
3,3,3,3,4),(-16.6591196545534,-15.9943584300589,-14.9947110281803,-13.9950636263016,
-12.9954162244229,-11.9957688225442,-10.9961214206655,-10.3759343473739),
 .UNSPECIFIED.);
#6318=B_SPLINE_CURVE_WITH_KNOTS('',3,(#44468,#44469,#44470,#44471,#44472,
#44473,#44474,#44475,#44476,#44477,#44478,#44479,#44480,#44481,#44482,#44483,
#44484,#44485,#44486,#44487,#44488,#44489),.UNSPECIFIED.,.F.,.F.,(4,3,3,
3,3,3,3,4),(7.39323051809279,7.99717921502952,8.99682661690821,9.99647401878689,
10.9961214206656,11.9957688225443,12.9954162244229,13.6764158252724),
 .UNSPECIFIED.);
#6319=B_SPLINE_CURVE_WITH_KNOTS('',3,(#44494,#44495,#44496,#44497,#44498,
#44499,#44500,#44501,#44502,#44503,#44504,#44505,#44506,#44507,#44508,#44509,
#44510,#44511,#44512,#44513,#44514,#44515),.UNSPECIFIED.,.F.,.F.,(4,3,3,
3,3,3,3,4),(-22.942304961733,-21.992242841331,-20.9925954394524,-19.9929480375737,
-18.993300635695,-17.9936532338163,-16.9940058319376,-16.6591196545534),
 .UNSPECIFIED.);
#6320=B_SPLINE_CURVE_WITH_KNOTS('',3,(#44516,#44517,#44518,#44519,#44520,
#44521,#44522,#44523,#44524,#44525,#44526,#44527,#44528,#44529,#44530,#44531,
#44532,#44533,#44534,#44535,#44536,#44537),.UNSPECIFIED.,.F.,.F.,(4,3,3,
3,3,3,3,4),(13.6764158252724,13.9950636263016,14.9947110281803,15.9943584300589,
16.9940058319376,17.9936532338163,18.9933006356949,19.959601132452),
 .UNSPECIFIED.);
#6321=B_SPLINE_CURVE_WITH_KNOTS('',3,(#44542,#44543,#44544,#44545,#44546,
#44547,#44548,#44549,#44550,#44551,#44552,#44553,#44554,#44555,#44556,#44557,
#44558,#44559,#44560,#44561,#44562,#44563,#44564,#44565,#44566),
 .UNSPECIFIED.,.F.,.F.,(4,3,3,3,3,3,3,3,4),(-29.2254902689126,-28.9897746544818,
-27.9901272526032,-26.9904798507245,-25.9908324488458,-24.9911850469671,
-23.9915376450884,-22.9918902432097,-22.942304961733),.UNSPECIFIED.);
#6322=B_SPLINE_CURVE_WITH_KNOTS('',3,(#44567,#44568,#44569,#44570,#44571,
#44572,#44573,#44574,#44575,#44576,#44577,#44578,#44579,#44580,#44581,#44582,
#44583,#44584,#44585,#44586,#44587,#44588,#44589,#44590,#44591),
 .UNSPECIFIED.,.F.,.F.,(4,3,3,3,3,3,3,3,4),(19.959601132452,19.9929480375736,
20.9925954394523,21.992242841331,22.9918902432097,23.9915376450884,24.9911850469671,
25.9908324488458,26.2427864396316),.UNSPECIFIED.);
#6323=B_SPLINE_CURVE_WITH_KNOTS('',3,(#44596,#44597,#44598,#44599,#44600,
#44601,#44602,#44603,#44604,#44605,#44606,#44607,#44608,#44609,#44610,#44611,
#44612,#44613,#44614,#44615,#44616,#44617),.UNSPECIFIED.,.F.,.F.,(4,3,3,
3,3,3,3,4),(-35.5086755760922,-34.9876590657539,-33.9880116638753,-32.9883642619966,
-31.9887168601179,-30.9890694582392,-29.9894220563605,-29.2254902689126),
 .UNSPECIFIED.);
#6324=B_SPLINE_CURVE_WITH_KNOTS('',3,(#44618,#44619,#44620,#44621,#44622,
#44623,#44624,#44625,#44626,#44627,#44628,#44629,#44630,#44631,#44632,#44633,
#44634,#44635,#44636,#44637,#44638,#44639),.UNSPECIFIED.,.F.,.F.,(4,3,3,
3,3,3,3,4),(26.2427864396316,26.9904798507245,27.9901272526032,28.9897746544819,
29.9894220563605,30.9890694582392,31.9887168601179,32.5259717468111),
 .UNSPECIFIED.);
#6325=B_SPLINE_CURVE_WITH_KNOTS('',3,(#44644,#44645,#44646,#44647,#44648,
#44649,#44650,#44651,#44652,#44653,#44654,#44655,#44656,#44657,#44658,#44659,
#44660,#44661,#44662,#44663,#44664,#44665),.UNSPECIFIED.,.F.,.F.,(4,3,3,
3,3,3,3,4),(-41.7918608832718,-40.985543477026,-39.9858960751474,-38.9862486732687,
-37.98660127139,-36.9869538695113,-35.9873064676326,-35.5086755760922),
 .UNSPECIFIED.);
#6326=B_SPLINE_CURVE_WITH_KNOTS('',3,(#44666,#44667,#44668,#44669,#44670,
#44671,#44672,#44673,#44674,#44675,#44676,#44677,#44678,#44679,#44680,#44681,
#44682,#44683,#44684,#44685,#44686,#44687),.UNSPECIFIED.,.F.,.F.,(4,3,3,
3,3,3,3,4),(32.5259717468111,32.9883642619966,33.9880116638753,34.987659065754,
35.9873064676326,36.9869538695113,37.98660127139,38.8091570539907),
 .UNSPECIFIED.);
#6327=B_SPLINE_CURVE_WITH_KNOTS('',3,(#44692,#44693,#44694,#44695,#44696,
#44697,#44698,#44699,#44700,#44701,#44702,#44703,#44704,#44705,#44706,#44707,
#44708,#44709,#44710,#44711,#44712,#44713,#44714,#44715,#44716),
 .UNSPECIFIED.,.F.,.F.,(4,3,3,3,3,3,3,3,4),(-48.0750461904514,-47.9830752901768,
-46.9834278882981,-45.9837804864195,-44.9841330845408,-43.9844856826621,
-42.9848382807834,-41.9851908789047,-41.7918608832718),.UNSPECIFIED.);
#6328=B_SPLINE_CURVE_WITH_KNOTS('',3,(#44717,#44718,#44719,#44720,#44721,
#44722,#44723,#44724,#44725,#44726,#44727,#44728,#44729,#44730,#44731,#44732,
#44733,#44734,#44735,#44736,#44737,#44738,#44739,#44740,#44741),
 .UNSPECIFIED.,.F.,.F.,(4,3,3,3,3,3,3,3,4),(38.8091570539907,38.9862486732687,
39.9858960751474,40.9855434770261,41.9851908789047,42.9848382807834,43.9844856826621,
44.9841330845408,45.0923423611703),.UNSPECIFIED.);
#6329=B_SPLINE_CURVE_WITH_KNOTS('',3,(#44746,#44747,#44748,#44749,#44750,
#44751,#44752,#44753,#44754,#44755,#44756,#44757,#44758,#44759,#44760,#44761,
#44762,#44763,#44764,#44765,#44766,#44767),.UNSPECIFIED.,.F.,.F.,(4,3,3,
3,3,3,3,4),(-54.358231497631,-53.9809597014489,-52.9813122995703,-51.9816648976916,
-50.9820174958129,-49.9823700939342,-48.9827226920555,-48.0750461904514),
 .UNSPECIFIED.);
#6330=B_SPLINE_CURVE_WITH_KNOTS('',3,(#44768,#44769,#44770,#44771,#44772,
#44773,#44774,#44775,#44776,#44777,#44778,#44779,#44780,#44781,#44782,#44783,
#44784,#44785,#44786,#44787,#44788,#44789),.UNSPECIFIED.,.F.,.F.,(4,3,3,
3,3,3,3,4),(45.0923423611703,45.9837804864195,46.9834278882981,47.9830752901768,
48.9827226920555,49.9823700939342,50.9820174958129,51.3755276683499),
 .UNSPECIFIED.);
#6331=B_SPLINE_CURVE_WITH_KNOTS('',3,(#44794,#44795,#44796,#44797,#44798,
#44799,#44800,#44801,#44802,#44803,#44804,#44805,#44806,#44807,#44808,#44809,
#44810,#44811,#44812,#44813,#44814,#44815),.UNSPECIFIED.,.F.,.F.,(4,3,3,
3,3,3,3,4),(-60.6414168048105,-59.978844112721,-58.9791967108424,-57.9795493089637,
-56.979901907085,-55.9802545052063,-54.9806071033276,-54.358231497631),
 .UNSPECIFIED.);
#6332=B_SPLINE_CURVE_WITH_KNOTS('',3,(#44816,#44817,#44818,#44819,#44820,
#44821,#44822,#44823,#44824,#44825,#44826,#44827,#44828,#44829,#44830,#44831,
#44832,#44833,#44834,#44835,#44836,#44837),.UNSPECIFIED.,.F.,.F.,(4,3,3,
3,3,3,3,4),(51.3755276683499,51.9816648976916,52.9813122995703,53.980959701449,
54.9806071033277,55.9802545052063,56.979901907085,57.6587129755296),
 .UNSPECIFIED.);
#6333=B_SPLINE_CURVE_WITH_KNOTS('',3,(#44842,#44843,#44844,#44845,#44846,
#44847,#44848,#44849,#44850,#44851,#44852,#44853,#44854,#44855,#44856,#44857,
#44858,#44859,#44860,#44861,#44862,#44863),.UNSPECIFIED.,.F.,.F.,(4,3,3,
3,3,3,3,4),(-66.9246021119901,-65.9767285239931,-64.9770811221145,-63.9774337202358,
-62.9777863183571,-61.9781389164784,-60.9784915145997,-60.6414168048105),
 .UNSPECIFIED.);
#6334=B_SPLINE_CURVE_WITH_KNOTS('',3,(#44864,#44865,#44866,#44867,#44868,
#44869,#44870,#44871,#44872,#44873,#44874,#44875,#44876,#44877,#44878,#44879,
#44880,#44881,#44882,#44883,#44884,#44885),.UNSPECIFIED.,.F.,.F.,(4,3,3,
3,3,3,3,4),(57.6587129755296,57.9795493089637,58.9791967108424,59.9788441127211,
60.9784915145998,61.9781389164785,62.9777863183572,63.9418982827091),
 .UNSPECIFIED.);
#6335=B_SPLINE_CURVE_WITH_KNOTS('',3,(#44890,#44891,#44892,#44893,#44894,
#44895,#44896,#44897,#44898,#44899,#44900,#44901,#44902,#44903,#44904,#44905,
#44906,#44907,#44908,#44909,#44910,#44911,#44912,#44913,#44914),
 .UNSPECIFIED.,.F.,.F.,(4,3,3,3,3,3,3,3,4),(-73.2077874191697,-72.9742603371439,
-71.9746129352653,-70.9749655333866,-69.9753181315079,-68.9756707296292,
-67.9760233277505,-66.9763759258718,-66.9246021119901),.UNSPECIFIED.);
#6336=B_SPLINE_CURVE_WITH_KNOTS('',3,(#44915,#44916,#44917,#44918,#44919,
#44920,#44921,#44922,#44923,#44924,#44925,#44926,#44927,#44928,#44929,#44930,
#44931,#44932,#44933,#44934,#44935,#44936,#44937,#44938,#44939),
 .UNSPECIFIED.,.F.,.F.,(4,3,3,3,3,3,3,3,4),(63.9418982827091,63.9774337202358,
64.9770811221145,65.9767285239932,66.9763759258719,67.9760233277506,68.9756707296293,
69.9753181315079,70.2250835898887),.UNSPECIFIED.);
#6337=B_SPLINE_CURVE_WITH_KNOTS('',3,(#44944,#44945,#44946,#44947,#44948,
#44949,#44950,#44951,#44952,#44953,#44954,#44955,#44956,#44957,#44958,#44959,
#44960,#44961,#44962,#44963,#44964,#44965),.UNSPECIFIED.,.F.,.F.,(4,3,3,
3,3,3,3,4),(-79.4909727263493,-78.972144748416,-77.9724973465374,-76.9728499446587,
-75.97320254278,-74.9735551409013,-73.9739077390226,-73.2077874191697),
 .UNSPECIFIED.);
#6338=B_SPLINE_CURVE_WITH_KNOTS('',3,(#44966,#44967,#44968,#44969,#44970,
#44971,#44972,#44973,#44974,#44975,#44976,#44977,#44978,#44979,#44980,#44981,
#44982,#44983,#44984,#44985,#44986,#44987),.UNSPECIFIED.,.F.,.F.,(4,3,3,
3,3,3,3,4),(70.2250835898887,70.9749655333866,71.9746129352653,72.974260337144,
73.9739077390227,74.9735551409013,75.97320254278,76.5082688970683),
 .UNSPECIFIED.);
#6339=B_SPLINE_CURVE_WITH_KNOTS('',3,(#44992,#44993,#44994,#44995,#44996,
#44997,#44998,#44999,#45000,#45001,#45002,#45003,#45004,#45005,#45006,#45007,
#45008,#45009,#45010,#45011,#45012,#45013),.UNSPECIFIED.,.F.,.F.,(4,3,3,
3,3,3,3,4),(-85.7741580335289,-84.9700291596882,-83.9703817578095,-82.9707343559308,
-81.9710869540521,-80.9714395521734,-79.9717921502947,-79.4909727263493),
 .UNSPECIFIED.);
#6340=B_SPLINE_CURVE_WITH_KNOTS('',3,(#45014,#45015,#45016,#45017,#45018,
#45019,#45020,#45021,#45022,#45023,#45024,#45025,#45026,#45027,#45028,#45029,
#45030,#45031,#45032,#45033,#45034,#45035),.UNSPECIFIED.,.F.,.F.,(4,3,3,
3,3,3,3,4),(76.5082688970683,76.9728499446587,77.9724973465374,78.9721447484161,
79.9717921502948,80.9714395521735,81.9710869540522,82.7914542042479),
 .UNSPECIFIED.);
#6341=B_SPLINE_CURVE_WITH_KNOTS('',3,(#45040,#45041,#45042,#45043,#45044,
#45045,#45046,#45047,#45048,#45049,#45050,#45051,#45052,#45053,#45054,#45055,
#45056,#45057,#45058,#45059,#45060,#45061,#45062,#45063,#45064),
 .UNSPECIFIED.,.F.,.F.,(4,3,3,3,3,3,3,3,4),(-92.0573433407085,-91.9675609728389,
-90.9679135709602,-89.9682661690816,-88.9686187672029,-87.9689713653242,
-86.9693239634455,-85.9696765615668,-85.7741580335289),.UNSPECIFIED.);
#6342=B_SPLINE_CURVE_WITH_KNOTS('',3,(#45065,#45066,#45067,#45068,#45069,
#45070,#45071,#45072,#45073,#45074,#45075,#45076,#45077,#45078,#45079,#45080,
#45081,#45082,#45083,#45084,#45085,#45086,#45087,#45088,#45089),
 .UNSPECIFIED.,.F.,.F.,(4,3,3,3,3,3,3,3,4),(82.7914542042479,82.9707343559309,
83.9703817578095,84.9700291596882,85.9696765615669,86.9693239634455,87.9689713653242,
88.9686187672029,89.0746395114275),.UNSPECIFIED.);
#6343=B_SPLINE_CURVE_WITH_KNOTS('',3,(#45094,#45095,#45096,#45097,#45098,
#45099,#45100,#45101,#45102,#45103,#45104,#45105,#45106,#45107,#45108,#45109,
#45110,#45111,#45112,#45113,#45114,#45115),.UNSPECIFIED.,.F.,.F.,(4,3,3,
3,3,3,3,4),(-98.3405286478881,-97.965445384111,-96.9657979822324,-95.9661505803537,
-94.966503178475,-93.9668557765963,-92.9672083747176,-92.0573433407085),
 .UNSPECIFIED.);
#6344=B_SPLINE_CURVE_WITH_KNOTS('',3,(#45116,#45117,#45118,#45119,#45120,
#45121,#45122,#45123,#45124,#45125,#45126,#45127,#45128,#45129,#45130,#45131,
#45132,#45133,#45134,#45135,#45136,#45137),.UNSPECIFIED.,.F.,.F.,(4,3,3,
3,3,3,3,4),(89.0746395114275,89.9682661690816,90.9679135709603,91.967560972839,
92.9672083747177,93.9668557765964,94.9665031784751,95.3578248186071),
 .UNSPECIFIED.);
#6345=B_SPLINE_CURVE_WITH_KNOTS('',3,(#45142,#45143,#45144,#45145,#45146,
#45147,#45148,#45149,#45150,#45151,#45152,#45153,#45154,#45155,#45156,#45157,
#45158,#45159,#45160,#45161,#45162,#45163),.UNSPECIFIED.,.F.,.F.,(4,3,3,
3,3,3,3,4),(-104.623713955068,-103.963329795383,-102.963682393504,-101.964034991626,
-100.964387589747,-99.9647401878684,-98.9650927859897,-98.3405286478881),
 .UNSPECIFIED.);
#6346=B_SPLINE_CURVE_WITH_KNOTS('',3,(#45164,#45165,#45166,#45167,#45168,
#45169,#45170,#45171,#45172,#45173,#45174,#45175,#45176,#45177,#45178,#45179,
#45180,#45181,#45182,#45183,#45184,#45185),.UNSPECIFIED.,.F.,.F.,(4,3,3,
3,3,3,3,4),(95.3578248186071,95.9661505803537,96.9657979822324,97.9654453841111,
98.9650927859898,99.9647401878685,100.964387589747,101.641010125787),
 .UNSPECIFIED.);
#6347=B_SPLINE_CURVE_WITH_KNOTS('',3,(#45190,#45191,#45192,#45193,#45194,
#45195,#45196,#45197,#45198,#45199,#45200,#45201,#45202,#45203,#45204,#45205,
#45206,#45207,#45208,#45209,#45210,#45211),.UNSPECIFIED.,.F.,.F.,(4,3,3,
3,3,3,3,4),(-110.906899262247,-109.961214206655,-108.961566804777,-107.961919402898,
-106.962272001019,-105.962624599141,-104.962977197262,-104.623713955068),
 .UNSPECIFIED.);
#6348=B_SPLINE_CURVE_WITH_KNOTS('',3,(#45212,#45213,#45214,#45215,#45216,
#45217,#45218,#45219,#45220,#45221,#45222,#45223,#45224,#45225,#45226,#45227,
#45228,#45229,#45230,#45231,#45232,#45233),.UNSPECIFIED.,.F.,.F.,(4,3,3,
3,3,3,3,4),(101.641010125787,101.964034991626,102.963682393505,103.963329795383,
104.962977197262,105.962624599141,106.962272001019,107.924195432966),
 .UNSPECIFIED.);
#6349=B_SPLINE_CURVE_WITH_KNOTS('',3,(#45238,#45239,#45240,#45241,#45242,
#45243,#45244,#45245,#45246,#45247,#45248,#45249,#45250,#45251,#45252,#45253,
#45254,#45255,#45256,#45257,#45258,#45259,#45260,#45261,#45262),
 .UNSPECIFIED.,.F.,.F.,(4,3,3,3,3,3,3,3,4),(-117.190084569427,-116.958746019806,
-115.959098617927,-114.959451216049,-113.95980381417,-112.960156412291,
-111.960509010413,-110.960861608534,-110.906899262247),.UNSPECIFIED.);
#6350=B_SPLINE_CURVE_WITH_KNOTS('',3,(#45263,#45264,#45265,#45266,#45267,
#45268,#45269,#45270,#45271,#45272,#45273,#45274,#45275,#45276,#45277,#45278,
#45279,#45280,#45281,#45282,#45283,#45284,#45285,#45286,#45287),
 .UNSPECIFIED.,.F.,.F.,(4,3,3,3,3,3,3,3,4),(107.924195432966,107.961919402898,
108.961566804777,109.961214206655,110.960861608534,111.960509010413,112.960156412291,
113.95980381417,114.207380740146),.UNSPECIFIED.);
#6351=B_SPLINE_CURVE_WITH_KNOTS('',3,(#45292,#45293,#45294,#45295,#45296,
#45297,#45298,#45299,#45300,#45301,#45302,#45303,#45304,#45305,#45306,#45307,
#45308,#45309,#45310,#45311,#45312,#45313),.UNSPECIFIED.,.F.,.F.,(4,3,3,
3,3,3,3,4),(-123.473269876606,-122.956630431078,-121.956983029199,-120.957335627321,
-119.957688225442,-118.958040823563,-117.958393421685,-117.190084569427),
 .UNSPECIFIED.);
#6352=B_SPLINE_CURVE_WITH_KNOTS('',3,(#45314,#45315,#45316,#45317,#45318,
#45319,#45320,#45321,#45322,#45323,#45324,#45325,#45326,#45327,#45328,#45329,
#45330,#45331,#45332,#45333,#45334,#45335),.UNSPECIFIED.,.F.,.F.,(4,3,3,
3,3,3,3,4),(114.207380740146,114.959451216049,115.959098617927,116.958746019806,
117.958393421685,118.958040823563,119.957688225442,120.490566047325),
 .UNSPECIFIED.);
#6353=B_SPLINE_CURVE_WITH_KNOTS('',3,(#45340,#45341,#45342,#45343,#45344,
#45345,#45346,#45347,#45348,#45349,#45350,#45351,#45352,#45353,#45354,#45355,
#45356,#45357,#45358,#45359,#45360,#45361),.UNSPECIFIED.,.F.,.F.,(4,3,3,
3,3,3,3,4),(-129.756455183786,-128.95451484235,-127.954867440472,-126.955220038593,
-125.955572636714,-124.955925234836,-123.956277832957,-123.473269876606),
 .UNSPECIFIED.);
#6354=B_SPLINE_CURVE_WITH_KNOTS('',3,(#45362,#45363,#45364,#45365,#45366,
#45367,#45368,#45369,#45370,#45371,#45372,#45373,#45374,#45375,#45376,#45377,
#45378,#45379,#45380,#45381,#45382,#45383),.UNSPECIFIED.,.F.,.F.,(4,3,3,
3,3,3,3,4),(120.490566047325,120.957335627321,121.9569830292,122.956630431078,
123.956277832957,124.955925234836,125.955572636714,126.773751354505),
 .UNSPECIFIED.);
#6355=B_SPLINE_CURVE_WITH_KNOTS('',3,(#45388,#45389,#45390,#45391,#45392,
#45393,#45394,#45395,#45396,#45397,#45398,#45399,#45400,#45401,#45402,#45403,
#45404,#45405,#45406,#45407,#45408,#45409,#45410,#45411,#45412),
 .UNSPECIFIED.,.F.,.F.,(4,3,3,3,3,3,3,3,4),(-136.039640490966,-135.952046655501,
-134.952399253622,-133.952751851744,-132.953104449865,-131.953457047986,
-130.953809646108,-129.954162244229,-129.756455183786),.UNSPECIFIED.);
#6356=B_SPLINE_CURVE_WITH_KNOTS('',3,(#45413,#45414,#45415,#45416,#45417,
#45418,#45419,#45420,#45421,#45422,#45423,#45424,#45425,#45426,#45427,#45428,
#45429,#45430,#45431,#45432,#45433,#45434,#45435,#45436,#45437),
 .UNSPECIFIED.,.F.,.F.,(4,3,3,3,3,3,3,3,4),(126.773751354505,126.955220038593,
127.954867440472,128.95451484235,129.954162244229,130.953809646108,131.953457047986,
132.953104449865,133.056936661685),.UNSPECIFIED.);
#6357=B_SPLINE_CURVE_WITH_KNOTS('',3,(#45442,#45443,#45444,#45445,#45446,
#45447,#45448,#45449,#45450,#45451,#45452,#45453,#45454,#45455,#45456,#45457,
#45458,#45459,#45460,#45461,#45462,#45463),.UNSPECIFIED.,.F.,.F.,(4,3,3,
3,3,3,3,4),(-142.322825798145,-141.949931066773,-140.950283664894,-139.950636263016,
-138.950988861137,-137.951341459258,-136.95169405738,-136.039640490966),
 .UNSPECIFIED.);
#6358=B_SPLINE_CURVE_WITH_KNOTS('',3,(#45464,#45465,#45466,#45467,#45468,
#45469,#45470,#45471,#45472,#45473,#45474,#45475,#45476,#45477,#45478,#45479,
#45480,#45481,#45482,#45483,#45484,#45485),.UNSPECIFIED.,.F.,.F.,(4,3,3,
3,3,3,3,4),(133.056936661685,133.952751851744,134.952399253622,135.952046655501,
136.95169405738,137.951341459259,138.950988861137,139.340121968864),
 .UNSPECIFIED.);
#6359=B_SPLINE_CURVE_WITH_KNOTS('',3,(#45490,#45491,#45492,#45493,#45494,
#45495,#45496,#45497,#45498,#45499,#45500,#45501,#45502,#45503,#45504,#45505,
#45506,#45507,#45508,#45509,#45510,#45511),.UNSPECIFIED.,.F.,.F.,(4,3,3,
3,3,3,3,4),(-148.606011105325,-147.947815478045,-146.948168076167,-145.948520674288,
-144.948873272409,-143.94922587053,-142.949578468652,-142.322825798145),
 .UNSPECIFIED.);
#6360=B_SPLINE_CURVE_WITH_KNOTS('',3,(#45512,#45513,#45514,#45515,#45516,
#45517,#45518,#45519,#45520,#45521,#45522,#45523,#45524,#45525,#45526,#45527,
#45528,#45529,#45530,#45531,#45532,#45533),.UNSPECIFIED.,.F.,.F.,(4,3,3,
3,3,3,3,4),(139.340121968864,139.950636263016,140.950283664895,141.949931066773,
142.949578468652,143.949225870531,144.948873272409,145.623307276044),
 .UNSPECIFIED.);
#6361=B_SPLINE_CURVE_WITH_KNOTS('',3,(#45538,#45539,#45540,#45541,#45542,
#45543,#45544,#45545,#45546,#45547,#45548,#45549,#45550,#45551,#45552,#45553,
#45554,#45555,#45556,#45557,#45558,#45559),.UNSPECIFIED.,.F.,.F.,(4,3,3,
3,3,3,3,4),(-154.889196412504,-153.945699889317,-152.946052487439,-151.94640508556,
-150.946757683681,-149.947110281803,-148.947462879924,-148.606011105325),
 .UNSPECIFIED.);
#6362=B_SPLINE_CURVE_WITH_KNOTS('',3,(#45560,#45561,#45562,#45563,#45564,
#45565,#45566,#45567,#45568,#45569,#45570,#45571,#45572,#45573,#45574,#45575,
#45576,#45577,#45578,#45579,#45580,#45581),.UNSPECIFIED.,.F.,.F.,(4,3,3,
3,3,3,3,4),(145.623307276044,145.948520674288,146.948168076167,147.947815478045,
148.947462879924,149.947110281803,150.946757683681,151.906492583223),
 .UNSPECIFIED.);
#6363=B_SPLINE_CURVE_WITH_KNOTS('',3,(#45586,#45587,#45588,#45589,#45590,
#45591,#45592,#45593,#45594,#45595,#45596,#45597,#45598,#45599,#45600,#45601,
#45602,#45603,#45604,#45605,#45606,#45607,#45608,#45609,#45610),
 .UNSPECIFIED.,.F.,.F.,(4,3,3,3,3,3,3,3,4),(-161.172381719684,-160.943231702468,
-159.943584300589,-158.943936898711,-157.944289496832,-156.944642094953,
-155.944994693075,-154.945347291196,-154.889196412504),.UNSPECIFIED.);
#6364=B_SPLINE_CURVE_WITH_KNOTS('',3,(#45611,#45612,#45613,#45614,#45615,
#45616,#45617,#45618,#45619,#45620,#45621,#45622,#45623,#45624,#45625,#45626,
#45627,#45628,#45629,#45630,#45631,#45632,#45633,#45634,#45635),
 .UNSPECIFIED.,.F.,.F.,(4,3,3,3,3,3,3,3,4),(151.906492583223,151.94640508556,
152.946052487439,153.945699889317,154.945347291196,155.944994693075,156.944642094953,
157.944289496832,158.189677890403),.UNSPECIFIED.);
#6365=B_SPLINE_CURVE_WITH_KNOTS('',3,(#45640,#45641,#45642,#45643,#45644,
#45645,#45646,#45647,#45648,#45649,#45650,#45651,#45652,#45653,#45654,#45655,
#45656,#45657,#45658,#45659,#45660,#45661),.UNSPECIFIED.,.F.,.F.,(4,3,3,
3,3,3,3,4),(-167.455567026863,-166.94111611374,-165.941468711862,-164.941821309983,
-163.942173908104,-162.942526506225,-161.942879104347,-161.172381719684),
 .UNSPECIFIED.);
#6366=B_SPLINE_CURVE_WITH_KNOTS('',3,(#45662,#45663,#45664,#45665,#45666,
#45667,#45668,#45669,#45670,#45671,#45672,#45673,#45674,#45675,#45676,#45677,
#45678,#45679,#45680,#45681,#45682,#45683),.UNSPECIFIED.,.F.,.F.,(4,3,3,
3,3,3,3,4),(158.189677890403,158.943936898711,159.94358430059,160.943231702468,
161.942879104347,162.942526506226,163.942173908104,164.472863197582),
 .UNSPECIFIED.);
#6367=B_SPLINE_CURVE_WITH_KNOTS('',3,(#45688,#45689,#45690,#45691,#45692,
#45693,#45694,#45695,#45696,#45697,#45698,#45699,#45700,#45701,#45702,#45703,
#45704,#45705,#45706,#45707,#45708,#45709),.UNSPECIFIED.,.F.,.F.,(4,3,3,
3,3,3,3,4),(-173.738752334043,-172.939000525012,-171.939353123134,-170.939705721255,
-169.940058319376,-168.940410917498,-167.940763515619,-167.455567026863),
 .UNSPECIFIED.);
#6368=B_SPLINE_CURVE_WITH_KNOTS('',3,(#45710,#45711,#45712,#45713,#45714,
#45715,#45716,#45717,#45718,#45719,#45720,#45721,#45722,#45723,#45724,#45725,
#45726,#45727,#45728,#45729,#45730,#45731),.UNSPECIFIED.,.F.,.F.,(4,3,3,
3,3,3,3,4),(164.472863197582,164.941821309983,165.941468711862,166.94111611374,
167.940763515619,168.940410917498,169.940058319376,170.756048504762),
 .UNSPECIFIED.);
#6369=B_SPLINE_CURVE_WITH_KNOTS('',3,(#45736,#45737,#45738,#45739,#45740,
#45741,#45742,#45743,#45744,#45745,#45746,#45747,#45748,#45749,#45750,#45751,
#45752,#45753,#45754,#45755,#45756,#45757,#45758,#45759,#45760),
 .UNSPECIFIED.,.F.,.F.,(4,3,3,3,3,3,3,3,4),(-180.021937641223,-179.936532338163,
-178.936884936284,-177.937237534406,-176.937590132527,-175.937942730648,
-174.93829532877,-173.938647926891,-173.738752334043),.UNSPECIFIED.);
#6370=B_SPLINE_CURVE_WITH_KNOTS('',3,(#45761,#45762,#45763,#45764,#45765,
#45766,#45767,#45768,#45769,#45770,#45771,#45772,#45773,#45774,#45775,#45776,
#45777,#45778,#45779,#45780,#45781,#45782,#45783,#45784,#45785),
 .UNSPECIFIED.,.F.,.F.,(4,3,3,3,3,3,3,3,4),(170.756048504762,170.939705721255,
171.939353123134,172.939000525012,173.938647926891,174.93829532877,175.937942730649,
176.937590132527,177.039233811942),.UNSPECIFIED.);
#6371=B_SPLINE_CURVE_WITH_KNOTS('',3,(#45790,#45791,#45792,#45793,#45794,
#45795,#45796,#45797,#45798,#45799,#45800,#45801,#45802,#45803,#45804,#45805,
#45806,#45807,#45808,#45809,#45810,#45811),.UNSPECIFIED.,.F.,.F.,(4,3,3,
3,3,3,3,4),(-186.305122948402,-185.934416749435,-184.934769347557,-183.935121945678,
-182.935474543799,-181.93582714192,-180.936179740042,-180.021937641223),
 .UNSPECIFIED.);
#6372=B_SPLINE_CURVE_WITH_KNOTS('',3,(#45812,#45813,#45814,#45815,#45816,
#45817,#45818,#45819,#45820,#45821,#45822,#45823,#45824,#45825,#45826,#45827,
#45828,#45829,#45830,#45831,#45832,#45833),.UNSPECIFIED.,.F.,.F.,(4,3,3,
3,3,3,3,4),(177.039233811942,177.937237534406,178.936884936285,179.936532338163,
180.936179740042,181.935827141921,182.935474543799,183.322419119121),
 .UNSPECIFIED.);
#6373=B_SPLINE_CURVE_WITH_KNOTS('',3,(#45838,#45839,#45840,#45841,#45842,
#45843,#45844,#45845,#45846,#45847,#45848,#45849,#45850,#45851,#45852,#45853,
#45854,#45855,#45856,#45857,#45858,#45859),.UNSPECIFIED.,.F.,.F.,(4,3,3,
3,3,3,3,4),(-192.588308255582,-191.932301160707,-190.932653758829,-189.93300635695,
-188.933358955071,-187.933711553193,-186.934064151314,-186.305122948402),
 .UNSPECIFIED.);
#6374=B_SPLINE_CURVE_WITH_KNOTS('',3,(#45860,#45861,#45862,#45863,#45864,
#45865,#45866,#45867,#45868,#45869,#45870,#45871,#45872,#45873,#45874,#45875,
#45876,#45877,#45878,#45879,#45880,#45881),.UNSPECIFIED.,.F.,.F.,(4,3,3,
3,3,3,3,4),(183.322419119121,183.935121945678,184.934769347557,185.934416749435,
186.934064151314,187.933711553193,188.933358955071,189.605604426301),
 .UNSPECIFIED.);
#6375=B_SPLINE_CURVE_WITH_KNOTS('',3,(#45886,#45887,#45888,#45889,#45890,
#45891,#45892,#45893,#45894,#45895,#45896,#45897,#45898,#45899,#45900,#45901,
#45902,#45903,#45904,#45905,#45906,#45907),.UNSPECIFIED.,.F.,.F.,(4,3,3,
3,3,3,3,4),(-198.871493562761,-197.930185571979,-196.930538170101,-195.930890768222,
-194.931243366343,-193.931595964465,-192.931948562586,-192.588308255582),
 .UNSPECIFIED.);
#6376=B_SPLINE_CURVE_WITH_KNOTS('',3,(#45908,#45909,#45910,#45911,#45912,
#45913,#45914,#45915,#45916,#45917,#45918,#45919,#45920,#45921,#45922,#45923,
#45924,#45925,#45926,#45927,#45928,#45929),.UNSPECIFIED.,.F.,.F.,(4,3,3,
3,3,3,3,4),(189.605604426301,189.93300635695,190.932653758829,191.932301160707,
192.931948562586,193.931595964465,194.931243366344,195.88878973348),
 .UNSPECIFIED.);
#6377=B_SPLINE_CURVE_WITH_KNOTS('',3,(#45934,#45935,#45936,#45937,#45938,
#45939,#45940,#45941,#45942,#45943,#45944,#45945,#45946,#45947,#45948,#45949,
#45950,#45951,#45952,#45953,#45954,#45955,#45956,#45957,#45958),
 .UNSPECIFIED.,.F.,.F.,(4,3,3,3,3,3,3,3,4),(-205.154678869941,-204.92771738513,
-203.928069983252,-202.928422581373,-201.928775179494,-200.929127777615,
-199.929480375737,-198.929832973858,-198.871493562761),.UNSPECIFIED.);
#6378=B_SPLINE_CURVE_WITH_KNOTS('',3,(#45959,#45960,#45961,#45962,#45963,
#45964,#45965,#45966,#45967,#45968,#45969,#45970,#45971,#45972,#45973,#45974,
#45975,#45976,#45977,#45978,#45979,#45980,#45981,#45982,#45983),
 .UNSPECIFIED.,.F.,.F.,(4,3,3,3,3,3,3,3,4),(195.88878973348,195.930890768222,
196.930538170101,197.93018557198,198.929832973858,199.929480375737,200.929127777616,
201.928775179494,202.17197504066),.UNSPECIFIED.);
#6379=B_SPLINE_CURVE_WITH_KNOTS('',3,(#45988,#45989,#45990,#45991,#45992,
#45993,#45994,#45995,#45996,#45997,#45998,#45999,#46000,#46001,#46002,#46003,
#46004,#46005,#46006,#46007,#46008,#46009),.UNSPECIFIED.,.F.,.F.,(4,3,3,
3,3,3,3,4),(-211.43786417712,-210.925601796402,-209.925954394524,-208.926306992645,
-207.926659590766,-206.927012188888,-205.927364787009,-205.154678869941),
 .UNSPECIFIED.);
#6380=B_SPLINE_CURVE_WITH_KNOTS('',3,(#46010,#46011,#46012,#46013,#46014,
#46015,#46016,#46017,#46018,#46019,#46020,#46021,#46022,#46023,#46024,#46025,
#46026,#46027,#46028,#46029,#46030,#46031),.UNSPECIFIED.,.F.,.F.,(4,3,3,
3,3,3,3,4),(202.17197504066,202.928422581373,203.928069983252,204.92771738513,
205.927364787009,206.927012188888,207.926659590766,208.455160347839),
 .UNSPECIFIED.);
#6381=B_SPLINE_CURVE_WITH_KNOTS('',3,(#46036,#46037,#46038,#46039,#46040,
#46041,#46042,#46043,#46044,#46045,#46046,#46047,#46048,#46049,#46050,#46051,
#46052,#46053,#46054,#46055,#46056,#46057),.UNSPECIFIED.,.F.,.F.,(4,3,3,
3,3,3,3,4),(-217.7210494843,-216.923486207674,-215.923838805796,-214.924191403917,
-213.924544002038,-212.92489660016,-211.925249198281,-211.43786417712),
 .UNSPECIFIED.);
#6382=B_SPLINE_CURVE_WITH_KNOTS('',3,(#46058,#46059,#46060,#46061,#46062,
#46063,#46064,#46065,#46066,#46067,#46068,#46069,#46070,#46071,#46072,#46073,
#46074,#46075,#46076,#46077,#46078,#46079),.UNSPECIFIED.,.F.,.F.,(4,3,3,
3,3,3,3,4),(208.455160347839,208.926306992645,209.925954394524,210.925601796402,
211.925249198281,212.92489660016,213.924544002039,214.738345655019),
 .UNSPECIFIED.);
#6383=B_SPLINE_CURVE_WITH_KNOTS('',3,(#46084,#46085,#46086,#46087,#46088,
#46089,#46090,#46091,#46092,#46093,#46094,#46095,#46096,#46097,#46098,#46099,
#46100,#46101,#46102,#46103,#46104,#46105,#46106,#46107,#46108),
 .UNSPECIFIED.,.F.,.F.,(4,3,3,3,3,3,3,3,4),(-224.00423479148,-223.921018020825,
-222.921370618947,-221.921723217068,-220.922075815189,-219.92242841331,
-218.922781011432,-217.923133609553,-217.7210494843),.UNSPECIFIED.);
#6384=B_SPLINE_CURVE_WITH_KNOTS('',3,(#46109,#46110,#46111,#46112,#46113,
#46114,#46115,#46116,#46117,#46118,#46119,#46120,#46121,#46122,#46123,#46124,
#46125,#46126,#46127,#46128,#46129,#46130,#46131,#46132,#46133),
 .UNSPECIFIED.,.F.,.F.,(4,3,3,3,3,3,3,3,4),(214.738345655019,214.924191403917,
215.923838805796,216.923486207675,217.923133609553,218.922781011432,219.922428413311,
220.922075815189,221.021530962199),.UNSPECIFIED.);
#6385=B_SPLINE_CURVE_WITH_KNOTS('',3,(#46138,#46139,#46140,#46141,#46142,
#46143,#46144,#46145,#46146,#46147,#46148,#46149,#46150,#46151,#46152,#46153,
#46154,#46155,#46156,#46157,#46158,#46159),.UNSPECIFIED.,.F.,.F.,(4,3,3,
3,3,3,3,4),(-230.287420098659,-229.918902432097,-228.919255030219,-227.91960762834,
-226.919960226461,-225.920312824583,-224.920665422704,-224.00423479148),
 .UNSPECIFIED.);
#6386=B_SPLINE_CURVE_WITH_KNOTS('',3,(#46160,#46161,#46162,#46163,#46164,
#46165,#46166,#46167,#46168,#46169,#46170,#46171,#46172,#46173,#46174,#46175,
#46176,#46177,#46178,#46179,#46180,#46181),.UNSPECIFIED.,.F.,.F.,(4,3,3,
3,3,3,3,4),(221.021530962199,221.921723217068,222.921370618947,223.921018020825,
224.920665422704,225.920312824583,226.919960226461,227.304716269378),
 .UNSPECIFIED.);
#6387=B_SPLINE_CURVE_WITH_KNOTS('',3,(#46186,#46187,#46188,#46189,#46190,
#46191,#46192,#46193,#46194,#46195,#46196,#46197,#46198,#46199,#46200,#46201,
#46202,#46203,#46204,#46205,#46206,#46207),.UNSPECIFIED.,.F.,.F.,(4,3,3,
3,3,3,3,4),(-236.570605405839,-235.916786843369,-234.917139441491,-233.917492039612,
-232.917844637733,-231.918197235855,-230.918549833976,-230.287420098659),
 .UNSPECIFIED.);
#6388=B_SPLINE_CURVE_WITH_KNOTS('',3,(#46208,#46209,#46210,#46211,#46212,
#46213,#46214,#46215,#46216,#46217,#46218,#46219,#46220,#46221,#46222,#46223,
#46224,#46225,#46226,#46227,#46228,#46229),.UNSPECIFIED.,.F.,.F.,(4,3,3,
3,3,3,3,4),(227.304716269378,227.91960762834,228.919255030219,229.918902432097,
230.918549833976,231.918197235855,232.917844637733,233.587901576558),
 .UNSPECIFIED.);
#6389=B_SPLINE_CURVE_WITH_KNOTS('',3,(#46234,#46235,#46236,#46237,#46238,
#46239,#46240,#46241,#46242,#46243,#46244,#46245,#46246,#46247,#46248,#46249,
#46250,#46251,#46252,#46253,#46254,#46255),.UNSPECIFIED.,.F.,.F.,(4,3,3,
3,3,3,3,4),(-242.853790713018,-241.914671254642,-240.915023852763,-239.915376450884,
-238.915729049006,-237.916081647127,-236.916434245248,-236.570605405839),
 .UNSPECIFIED.);
#6390=B_SPLINE_CURVE_WITH_KNOTS('',3,(#46256,#46257,#46258,#46259,#46260,
#46261,#46262,#46263,#46264,#46265,#46266,#46267,#46268,#46269,#46270,#46271,
#46272,#46273,#46274,#46275,#46276,#46277),.UNSPECIFIED.,.F.,.F.,(4,3,3,
3,3,3,3,4),(233.587901576558,233.917492039612,234.917139441491,235.91678684337,
236.916434245248,237.916081647127,238.915729049006,239.871086883737),
 .UNSPECIFIED.);
#6391=B_SPLINE_CURVE_WITH_KNOTS('',3,(#46282,#46283,#46284,#46285,#46286,
#46287,#46288,#46289,#46290,#46291,#46292,#46293,#46294,#46295,#46296,#46297,
#46298,#46299,#46300,#46301,#46302,#46303,#46304,#46305,#46306),
 .UNSPECIFIED.,.F.,.F.,(4,3,3,3,3,3,3,3,4),(-249.136976020198,-248.912203067792,
-247.912555665914,-246.912908264035,-245.913260862156,-244.913613460278,
-243.913966058399,-242.91431865652,-242.853790713018),.UNSPECIFIED.);
#6392=B_SPLINE_CURVE_WITH_KNOTS('',3,(#46307,#46308,#46309,#46310,#46311,
#46312,#46313,#46314,#46315,#46316,#46317,#46318,#46319,#46320,#46321,#46322,
#46323,#46324,#46325,#46326,#46327,#46328,#46329,#46330,#46331),
 .UNSPECIFIED.,.F.,.F.,(4,3,3,3,3,3,3,3,4),(239.871086883737,239.915376450884,
240.915023852763,241.914671254642,242.91431865652,243.913966058399,244.913613460278,
245.913260862156,246.154272190917),.UNSPECIFIED.);
#6393=B_SPLINE_CURVE_WITH_KNOTS('',3,(#46336,#46337,#46338,#46339,#46340,
#46341,#46342,#46343,#46344,#46345,#46346,#46347,#46348,#46349,#46350,#46351,
#46352,#46353,#46354,#46355,#46356,#46357),.UNSPECIFIED.,.F.,.F.,(4,3,3,
3,3,3,3,4),(-255.420161327377,-254.910087479064,-253.910440077186,-252.910792675307,
-251.911145273428,-250.91149787155,-249.911850469671,-249.136976020198),
 .UNSPECIFIED.);
#6394=B_SPLINE_CURVE_WITH_KNOTS('',3,(#46358,#46359,#46360,#46361,#46362,
#46363,#46364,#46365,#46366,#46367,#46368,#46369,#46370,#46371,#46372,#46373,
#46374,#46375,#46376,#46377,#46378,#46379),.UNSPECIFIED.,.F.,.F.,(4,3,3,
3,3,3,3,4),(246.154272190917,246.912908264035,247.912555665914,248.912203067792,
249.911850469671,250.91149787155,251.911145273429,252.437457498096),
 .UNSPECIFIED.);
#6395=B_SPLINE_CURVE_WITH_KNOTS('',3,(#46384,#46385,#46386,#46387,#46388,
#46389,#46390,#46391,#46392,#46393,#46394,#46395,#46396,#46397,#46398,#46399,
#46400,#46401,#46402,#46403,#46404,#46405),.UNSPECIFIED.,.F.,.F.,(4,3,3,
3,3,3,3,4),(-261.703346634557,-260.907971890337,-259.908324488458,-258.908677086579,
-257.9090296847,-256.909382282822,-255.909734880943,-255.420161327377),
 .UNSPECIFIED.);
#6396=B_SPLINE_CURVE_WITH_KNOTS('',3,(#46406,#46407,#46408,#46409,#46410,
#46411,#46412,#46413,#46414,#46415,#46416,#46417,#46418,#46419,#46420,#46421,
#46422,#46423,#46424,#46425,#46426,#46427),.UNSPECIFIED.,.F.,.F.,(4,3,3,
3,3,3,3,4),(252.437457498096,252.910792675307,253.910440077186,254.910087479065,
255.909734880943,256.909382282822,257.909029684701,258.720642805276),
 .UNSPECIFIED.);
#6397=B_SPLINE_CURVE_WITH_KNOTS('',3,(#46432,#46433,#46434,#46435,#46436,
#46437,#46438,#46439,#46440,#46441,#46442,#46443,#46444,#46445,#46446,#46447,
#46448,#46449,#46450,#46451,#46452,#46453,#46454,#46455,#46456),
 .UNSPECIFIED.,.F.,.F.,(4,3,3,3,3,3,3,3,4),(-267.986531941737,-267.905503703487,
-266.905856301609,-265.90620889973,-264.906561497851,-263.906914095973,
-262.907266694094,-261.907619292215,-261.703346634557),.UNSPECIFIED.);
#6398=B_SPLINE_CURVE_WITH_KNOTS('',3,(#46457,#46458,#46459,#46460,#46461,
#46462,#46463,#46464,#46465,#46466,#46467,#46468,#46469,#46470,#46471,#46472,
#46473,#46474,#46475,#46476,#46477,#46478,#46479,#46480,#46481),
 .UNSPECIFIED.,.F.,.F.,(4,3,3,3,3,3,3,3,4),(258.720642805276,258.908677086579,
259.908324488458,260.907971890337,261.907619292215,262.907266694094,263.906914095973,
264.906561497851,265.003828112455),.UNSPECIFIED.);
#6399=B_SPLINE_CURVE_WITH_KNOTS('',3,(#46486,#46487,#46488,#46489,#46490,
#46491,#46492,#46493,#46494,#46495,#46496,#46497,#46498,#46499,#46500,#46501,
#46502,#46503,#46504,#46505,#46506,#46507),.UNSPECIFIED.,.F.,.F.,(4,3,3,
3,3,3,3,4),(-274.269717248916,-273.903388114759,-272.903740712881,-271.904093311002,
-270.904445909123,-269.904798507245,-268.905151105366,-267.986531941737),
 .UNSPECIFIED.);
#6400=B_SPLINE_CURVE_WITH_KNOTS('',3,(#46508,#46509,#46510,#46511,#46512,
#46513,#46514,#46515,#46516,#46517,#46518,#46519,#46520,#46521,#46522,#46523,
#46524,#46525,#46526,#46527,#46528,#46529),.UNSPECIFIED.,.F.,.F.,(4,3,3,
3,3,3,3,4),(265.003828112455,265.90620889973,266.905856301609,267.905503703488,
268.905151105366,269.904798507245,270.904445909124,271.287013419635),
 .UNSPECIFIED.);
#6401=B_SPLINE_CURVE_WITH_KNOTS('',3,(#46534,#46535,#46536,#46537,#46538,
#46539,#46540,#46541,#46542,#46543,#46544,#46545,#46546,#46547,#46548,#46549,
#46550,#46551,#46552,#46553,#46554,#46555),.UNSPECIFIED.,.F.,.F.,(4,3,3,
3,3,3,3,4),(-280.552902556096,-279.901272526031,-278.901625124153,-277.901977722274,
-276.902330320395,-275.902682918517,-274.903035516638,-274.269717248916),
 .UNSPECIFIED.);
#6402=B_SPLINE_CURVE_WITH_KNOTS('',3,(#46556,#46557,#46558,#46559,#46560,
#46561,#46562,#46563,#46564,#46565,#46566,#46567,#46568,#46569,#46570,#46571,
#46572,#46573,#46574,#46575,#46576,#46577),.UNSPECIFIED.,.F.,.F.,(4,3,3,
3,3,3,3,4),(271.287013419635,271.904093311002,272.903740712881,273.90338811476,
274.903035516638,275.902682918517,276.902330320396,277.570198726815),
 .UNSPECIFIED.);
#6403=B_SPLINE_CURVE_WITH_KNOTS('',3,(#46582,#46583,#46584,#46585,#46586,
#46587,#46588,#46589,#46590,#46591,#46592,#46593,#46594,#46595,#46596,#46597,
#46598,#46599,#46600,#46601,#46602,#46603),.UNSPECIFIED.,.F.,.F.,(4,3,3,
3,3,3,3,4),(-286.836087863275,-285.899156937304,-284.899509535425,-283.899862133546,
-282.900214731668,-281.900567329789,-280.90091992791,-280.552902556096),
 .UNSPECIFIED.);
#6404=B_SPLINE_CURVE_WITH_KNOTS('',3,(#46604,#46605,#46606,#46607,#46608,
#46609,#46610,#46611,#46612,#46613,#46614,#46615,#46616,#46617,#46618,#46619,
#46620,#46621,#46622,#46623,#46624,#46625),.UNSPECIFIED.,.F.,.F.,(4,3,3,
3,3,3,3,4),(277.570198726815,277.901977722274,278.901625124153,279.901272526032,
280.90091992791,281.900567329789,282.900214731668,283.853384033994),
 .UNSPECIFIED.);
#6405=B_SPLINE_CURVE_WITH_KNOTS('',3,(#46630,#46631,#46632,#46633,#46634,
#46635,#46636,#46637,#46638,#46639,#46640,#46641,#46642,#46643,#46644,#46645,
#46646,#46647,#46648,#46649,#46650,#46651,#46652,#46653,#46654),
 .UNSPECIFIED.,.F.,.F.,(4,3,3,3,3,3,3,3,4),(-293.119273170455,-292.896688750454,
-291.897041348576,-290.897393946697,-289.897746544818,-288.89809914294,
-287.898451741061,-286.898804339182,-286.836087863275),.UNSPECIFIED.);
#6406=B_SPLINE_CURVE_WITH_KNOTS('',3,(#46655,#46656,#46657,#46658,#46659,
#46660,#46661,#46662,#46663,#46664,#46665,#46666,#46667,#46668,#46669,#46670,
#46671,#46672,#46673,#46674,#46675,#46676,#46677,#46678,#46679),
 .UNSPECIFIED.,.F.,.F.,(4,3,3,3,3,3,3,3,4),(283.853384033994,283.899862133546,
284.899509535425,285.899156937304,286.898804339183,287.898451741061,288.89809914294,
289.897746544819,290.136569341174),.UNSPECIFIED.);
#6407=B_SPLINE_CURVE_WITH_KNOTS('',3,(#46684,#46685,#46686,#46687,#46688,
#46689,#46690,#46691,#46692,#46693,#46694,#46695,#46696,#46697,#46698,#46699,
#46700,#46701,#46702,#46703,#46704,#46705),.UNSPECIFIED.,.F.,.F.,(4,3,3,
3,3,3,3,4),(-299.402458477634,-298.894573161726,-297.894925759848,-296.895278357969,
-295.89563095609,-294.895983554212,-293.896336152333,-293.119273170455),
 .UNSPECIFIED.);
#6408=B_SPLINE_CURVE_WITH_KNOTS('',3,(#46706,#46707,#46708,#46709,#46710,
#46711,#46712,#46713,#46714,#46715,#46716,#46717,#46718,#46719,#46720,#46721,
#46722,#46723,#46724,#46725,#46726,#46727),.UNSPECIFIED.,.F.,.F.,(4,3,3,
3,3,3,3,4),(290.136569341174,290.897393946697,291.897041348576,292.896688750455,
293.896336152333,294.895983554212,295.895630956091,296.419754648353),
 .UNSPECIFIED.);
#6409=B_SPLINE_CURVE_WITH_KNOTS('',3,(#46732,#46733,#46734,#46735,#46736,
#46737,#46738,#46739,#46740,#46741,#46742,#46743,#46744,#46745,#46746,#46747,
#46748,#46749,#46750,#46751,#46752,#46753),.UNSPECIFIED.,.F.,.F.,(4,3,3,
3,3,3,3,4),(-305.685643784814,-304.892457572999,-303.89281017112,-302.893162769241,
-301.893515367363,-300.893867965484,-299.894220563605,-299.402458477634),
 .UNSPECIFIED.);
#6410=B_SPLINE_CURVE_WITH_KNOTS('',3,(#46754,#46755,#46756,#46757,#46758,
#46759,#46760,#46761,#46762,#46763,#46764,#46765,#46766,#46767,#46768,#46769,
#46770,#46771,#46772,#46773,#46774,#46775),.UNSPECIFIED.,.F.,.F.,(4,3,3,
3,3,3,3,4),(296.419754648353,296.895278357969,297.894925759848,298.894573161727,
299.894220563605,300.893867965484,301.893515367363,302.702939955533),
 .UNSPECIFIED.);
#6411=B_SPLINE_CURVE_WITH_KNOTS('',3,(#46780,#46781,#46782,#46783,#46784,
#46785,#46786,#46787,#46788,#46789,#46790,#46791,#46792,#46793,#46794,#46795,
#46796,#46797,#46798,#46799,#46800,#46801,#46802,#46803,#46804),
 .UNSPECIFIED.,.F.,.F.,(4,3,3,3,3,3,3,3,4),(-311.968829091993,-311.889989386149,
-310.890341984271,-309.890694582392,-308.891047180513,-307.891399778635,
-306.891752376756,-305.892104974877,-305.685643784814),.UNSPECIFIED.);
#6412=B_SPLINE_CURVE_WITH_KNOTS('',3,(#46805,#46806,#46807,#46808,#46809,
#46810,#46811,#46812,#46813,#46814,#46815,#46816,#46817,#46818,#46819,#46820,
#46821,#46822,#46823,#46824,#46825,#46826,#46827,#46828,#46829),
 .UNSPECIFIED.,.F.,.F.,(4,3,3,3,3,3,3,3,4),(302.702939955533,302.893162769242,
303.89281017112,304.892457572999,305.892104974878,306.891752376756,307.891399778635,
308.891047180514,308.986125262712),.UNSPECIFIED.);
#6413=B_SPLINE_CURVE_WITH_KNOTS('',3,(#46834,#46835,#46836,#46837,#46838,
#46839,#46840,#46841,#46842,#46843,#46844,#46845,#46846,#46847,#46848,#46849,
#46850,#46851,#46852,#46853,#46854,#46855),.UNSPECIFIED.,.F.,.F.,(4,3,3,
3,3,3,3,4),(-318.252014399173,-317.887873797421,-316.888226395543,-315.888578993664,
-314.888931591785,-313.889284189907,-312.889636788028,-311.968829091993),
 .UNSPECIFIED.);
#6414=B_SPLINE_CURVE_WITH_KNOTS('',3,(#46856,#46857,#46858,#46859,#46860,
#46861,#46862,#46863,#46864,#46865,#46866,#46867,#46868,#46869,#46870,#46871,
#46872,#46873,#46874,#46875,#46876,#46877),.UNSPECIFIED.,.F.,.F.,(4,3,3,
3,3,3,3,4),(308.986125262712,309.890694582392,310.890341984271,311.88998938615,
312.889636788028,313.889284189907,314.888931591786,315.269310569892),
 .UNSPECIFIED.);
#6415=B_SPLINE_CURVE_WITH_KNOTS('',3,(#46882,#46883,#46884,#46885,#46886,
#46887,#46888,#46889,#46890,#46891,#46892,#46893,#46894,#46895,#46896,#46897,
#46898,#46899,#46900,#46901,#46902,#46903),.UNSPECIFIED.,.F.,.F.,(4,3,3,
3,3,3,3,4),(-324.535199706353,-323.885758208694,-322.886110806815,-321.886463404936,
-320.886816003058,-319.887168601179,-318.8875211993,-318.252014399173),
 .UNSPECIFIED.);
#6416=B_SPLINE_CURVE_WITH_KNOTS('',3,(#46904,#46905,#46906,#46907,#46908,
#46909,#46910,#46911,#46912,#46913,#46914,#46915,#46916,#46917,#46918,#46919,
#46920,#46921,#46922,#46923,#46924,#46925),.UNSPECIFIED.,.F.,.F.,(4,3,3,
3,3,3,3,4),(315.269310569892,315.888578993664,316.888226395543,317.887873797422,
318.8875211993,319.887168601179,320.886816003058,321.552495877072),
 .UNSPECIFIED.);
#6417=B_SPLINE_CURVE_WITH_KNOTS('',3,(#46930,#46931,#46932,#46933,#46934,
#46935,#46936,#46937,#46938,#46939,#46940,#46941,#46942,#46943,#46944,#46945,
#46946,#46947,#46948,#46949,#46950,#46951),.UNSPECIFIED.,.F.,.F.,(4,3,3,
3,3,3,3,4),(-330.818385013532,-329.883642619966,-328.883995218087,-327.884347816208,
-326.88470041433,-325.885053012451,-324.885405610572,-324.535199706353),
 .UNSPECIFIED.);
#6418=B_SPLINE_CURVE_WITH_KNOTS('',3,(#46952,#46953,#46954,#46955,#46956,
#46957,#46958,#46959,#46960,#46961,#46962,#46963,#46964,#46965,#46966,#46967,
#46968,#46969,#46970,#46971,#46972,#46973),.UNSPECIFIED.,.F.,.F.,(4,3,3,
3,3,3,3,4),(321.552495877072,321.886463404936,322.886110806815,323.885758208694,
324.885405610572,325.885053012451,326.88470041433,327.835681184251),
 .UNSPECIFIED.);
#6419=B_SPLINE_CURVE_WITH_KNOTS('',3,(#46978,#46979,#46980,#46981,#46982,
#46983,#46984,#46985,#46986,#46987,#46988,#46989,#46990,#46991,#46992,#46993,
#46994,#46995,#46996,#46997,#46998,#46999,#47000,#47001,#47002),
 .UNSPECIFIED.,.F.,.F.,(4,3,3,3,3,3,3,3,4),(-337.101570320712,-336.881174433116,
-335.881527031238,-334.881879629359,-333.88223222748,-332.882584825602,
-331.882937423723,-330.883290021844,-330.818385013532),.UNSPECIFIED.);
#6420=B_SPLINE_CURVE_WITH_KNOTS('',3,(#47003,#47004,#47005,#47006,#47007,
#47008,#47009,#47010,#47011,#47012,#47013,#47014,#47015,#47016,#47017,#47018,
#47019,#47020,#47021,#47022,#47023,#47024,#47025,#47026,#47027),
 .UNSPECIFIED.,.F.,.F.,(4,3,3,3,3,3,3,3,4),(327.835681184251,327.884347816209,
328.883995218087,329.883642619966,330.883290021845,331.882937423723,332.882584825602,
333.882232227481,334.118866491431),.UNSPECIFIED.);
#6421=B_SPLINE_CURVE_WITH_KNOTS('',3,(#47032,#47033,#47034,#47035,#47036,
#47037,#47038,#47039,#47040,#47041,#47042,#47043,#47044,#47045,#47046,#47047,
#47048,#47049,#47050,#47051,#47052,#47053),.UNSPECIFIED.,.F.,.F.,(4,3,3,
3,3,3,3,4),(-343.384755627891,-342.879058844389,-341.87941144251,-340.879764040631,
-339.880116638753,-338.880469236874,-337.880821834995,-337.101570320712),
 .UNSPECIFIED.);
#6422=B_SPLINE_CURVE_WITH_KNOTS('',3,(#47054,#47055,#47056,#47057,#47058,
#47059,#47060,#47061,#47062,#47063,#47064,#47065,#47066,#47067,#47068,#47069,
#47070,#47071,#47072,#47073,#47074,#47075),.UNSPECIFIED.,.F.,.F.,(4,3,3,
3,3,3,3,4),(334.118866491431,334.881879629359,335.881527031238,336.881174433117,
337.880821834995,338.880469236874,339.880116638753,340.40205179861),
 .UNSPECIFIED.);
#6423=B_SPLINE_CURVE_WITH_KNOTS('',3,(#47080,#47081,#47082,#47083,#47084,
#47085,#47086,#47087,#47088,#47089,#47090,#47091,#47092,#47093,#47094,#47095,
#47096,#47097,#47098,#47099,#47100,#47101),.UNSPECIFIED.,.F.,.F.,(4,3,3,
3,3,3,3,4),(-349.667940935071,-348.876943255661,-347.877295853782,-346.877648451903,
-345.878001050025,-344.878353648146,-343.878706246267,-343.384755627891),
 .UNSPECIFIED.);
#6424=B_SPLINE_CURVE_WITH_KNOTS('',3,(#47102,#47103,#47104,#47105,#47106,
#47107,#47108,#47109,#47110,#47111,#47112,#47113,#47114,#47115,#47116,#47117,
#47118,#47119,#47120,#47121,#47122,#47123),.UNSPECIFIED.,.F.,.F.,(4,3,3,
3,3,3,3,4),(340.40205179861,340.879764040631,341.87941144251,342.879058844389,
343.878706246268,344.878353648146,345.878001050025,346.68523710579),
 .UNSPECIFIED.);
#6425=B_SPLINE_CURVE_WITH_KNOTS('',3,(#47128,#47129,#47130,#47131,#47132,
#47133,#47134,#47135,#47136,#47137,#47138,#47139,#47140,#47141,#47142,#47143,
#47144,#47145,#47146,#47147,#47148,#47149,#47150,#47151,#47152),
 .UNSPECIFIED.,.F.,.F.,(4,3,3,3,3,3,3,3,4),(-355.95112624225,-355.874475068811,
-354.874827666933,-353.875180265054,-352.875532863175,-351.875885461297,
-350.876238059418,-349.876590657539,-349.667940935071),.UNSPECIFIED.);
#6426=B_SPLINE_CURVE_WITH_KNOTS('',3,(#47153,#47154,#47155,#47156,#47157,
#47158,#47159,#47160,#47161,#47162,#47163,#47164,#47165,#47166,#47167,#47168,
#47169,#47170,#47171,#47172,#47173,#47174,#47175,#47176,#47177),
 .UNSPECIFIED.,.F.,.F.,(4,3,3,3,3,3,3,3,4),(346.68523710579,346.877648451904,
347.877295853782,348.876943255661,349.87659065754,350.876238059418,351.875885461297,
352.875532863176,352.968422412969),.UNSPECIFIED.);
#6427=B_SPLINE_CURVE_WITH_KNOTS('',3,(#47182,#47183,#47184,#47185,#47186,
#47187,#47188,#47189,#47190,#47191,#47192,#47193,#47194,#47195,#47196,#47197,
#47198,#47199,#47200,#47201,#47202,#47203),.UNSPECIFIED.,.F.,.F.,(4,3,3,
3,3,3,3,4),(-362.23431154943,-361.872359480084,-360.872712078205,-359.873064676326,
-358.873417274448,-357.873769872569,-356.87412247069,-355.95112624225),
 .UNSPECIFIED.);
#6428=B_SPLINE_CURVE_WITH_KNOTS('',3,(#47204,#47205,#47206,#47207,#47208,
#47209,#47210,#47211,#47212,#47213,#47214,#47215,#47216,#47217,#47218,#47219,
#47220,#47221,#47222,#47223,#47224,#47225),.UNSPECIFIED.,.F.,.F.,(4,3,3,
3,3,3,3,4),(352.968422412969,353.875180265054,354.874827666933,355.874475068812,
356.87412247069,357.873769872569,358.873417274448,359.251607720149),
 .UNSPECIFIED.);
#6429=B_SPLINE_CURVE_WITH_KNOTS('',3,(#47230,#47231,#47232,#47233,#47234,
#47235,#47236,#47237,#47238,#47239,#47240,#47241,#47242,#47243,#47244,#47245,
#47246,#47247,#47248,#47249,#47250,#47251),.UNSPECIFIED.,.F.,.F.,(4,3,3,
3,3,3,3,4),(-368.51749685661,-367.870243891356,-366.870596489477,-365.870949087598,
-364.87130168572,-363.871654283841,-362.872006881962,-362.23431154943),
 .UNSPECIFIED.);
#6430=B_SPLINE_CURVE_WITH_KNOTS('',3,(#47252,#47253,#47254,#47255,#47256,
#47257,#47258,#47259,#47260,#47261,#47262,#47263,#47264,#47265,#47266,#47267,
#47268,#47269,#47270,#47271,#47272,#47273),.UNSPECIFIED.,.F.,.F.,(4,3,3,
3,3,3,3,4),(359.251607720149,359.873064676327,360.872712078205,361.872359480084,
362.872006881963,363.871654283841,364.87130168572,365.534793027328),
 .UNSPECIFIED.);
#6431=B_SPLINE_CURVE_WITH_KNOTS('',3,(#47278,#47279,#47280,#47281,#47282,
#47283,#47284,#47285,#47286,#47287,#47288,#47289,#47290,#47291,#47292,#47293,
#47294,#47295,#47296,#47297,#47298,#47299),.UNSPECIFIED.,.F.,.F.,(4,3,3,
3,3,3,3,4),(-374.800682163789,-373.868128302628,-372.868480900749,-371.86883349887,
-370.869186096992,-369.869538695113,-368.869891293234,-368.51749685661),
 .UNSPECIFIED.);
#6432=B_SPLINE_CURVE_WITH_KNOTS('',3,(#47300,#47301,#47302,#47303,#47304,
#47305,#47306,#47307,#47308,#47309,#47310,#47311,#47312,#47313,#47314,#47315,
#47316,#47317,#47318,#47319,#47320,#47321),.UNSPECIFIED.,.F.,.F.,(4,3,3,
3,3,3,3,4),(365.534793027328,365.870949087599,366.870596489477,367.870243891356,
368.869891293235,369.869538695113,370.869186096992,371.817978334508),
 .UNSPECIFIED.);
#6433=B_SPLINE_CURVE_WITH_KNOTS('',3,(#47326,#47327,#47328,#47329,#47330,
#47331,#47332,#47333,#47334,#47335,#47336,#47337,#47338,#47339,#47340,#47341,
#47342,#47343,#47344,#47345,#47346,#47347,#47348,#47349,#47350),
 .UNSPECIFIED.,.F.,.F.,(4,3,3,3,3,3,3,3,4),(-381.083867470969,-380.865660115779,
-379.8660127139,-378.866365312021,-377.866717910143,-376.867070508264,-375.867423106385,
-374.867775704506,-374.800682163789),.UNSPECIFIED.);
#6434=B_SPLINE_CURVE_WITH_KNOTS('',3,(#47351,#47352,#47353,#47354,#47355,
#47356,#47357,#47358,#47359,#47360,#47361,#47362,#47363,#47364,#47365,#47366,
#47367,#47368,#47369,#47370,#47371,#47372,#47373,#47374,#47375),
 .UNSPECIFIED.,.F.,.F.,(4,3,3,3,3,3,3,3,4),(371.817978334508,371.868833498871,
372.868480900749,373.868128302628,374.867775704507,375.867423106385,376.867070508264,
377.866717910143,378.101163641688),.UNSPECIFIED.);
#6435=B_SPLINE_CURVE_WITH_KNOTS('',3,(#47380,#47381,#47382,#47383,#47384,
#47385,#47386,#47387,#47388,#47389,#47390,#47391,#47392,#47393,#47394,#47395,
#47396,#47397,#47398,#47399,#47400,#47401),.UNSPECIFIED.,.F.,.F.,(4,3,3,
3,3,3,3,4),(-387.367052778148,-386.863544527051,-385.863897125172,-384.864249723293,
-383.864602321415,-382.864954919536,-381.865307517657,-381.083867470969),
 .UNSPECIFIED.);
#6436=B_SPLINE_CURVE_WITH_KNOTS('',3,(#47402,#47403,#47404,#47405,#47406,
#47407,#47408,#47409,#47410,#47411,#47412,#47413,#47414,#47415,#47416,#47417,
#47418,#47419,#47420,#47421,#47422,#47423),.UNSPECIFIED.,.F.,.F.,(4,3,3,
3,3,3,3,4),(378.101163641688,378.866365312022,379.8660127139,380.865660115779,
381.865307517658,382.864954919536,383.864602321415,384.384348948867),
 .UNSPECIFIED.);
#6437=B_SPLINE_CURVE_WITH_KNOTS('',3,(#47428,#47429,#47430,#47431,#47432,
#47433,#47434,#47435,#47436,#47437,#47438,#47439,#47440,#47441,#47442,#47443,
#47444,#47445,#47446,#47447,#47448,#47449),.UNSPECIFIED.,.F.,.F.,(4,3,3,
3,3,3,3,4),(-393.650238085328,-392.861428938323,-391.861781536444,-390.862134134565,
-389.862486732687,-388.862839330808,-387.863191928929,-387.367052778148),
 .UNSPECIFIED.);
#6438=B_SPLINE_CURVE_WITH_KNOTS('',3,(#47450,#47451,#47452,#47453,#47454,
#47455,#47456,#47457,#47458,#47459,#47460,#47461,#47462,#47463,#47464,#47465,
#47466,#47467,#47468,#47469,#47470,#47471),.UNSPECIFIED.,.F.,.F.,(4,3,3,
3,3,3,3,4),(384.384348948867,384.864249723294,385.863897125172,386.863544527051,
387.86319192893,388.862839330808,389.862486732687,390.667534256047),
 .UNSPECIFIED.);
#6439=B_SPLINE_CURVE_WITH_KNOTS('',3,(#47476,#47477,#47478,#47479,#47480,
#47481,#47482,#47483,#47484,#47485,#47486,#47487,#47488,#47489,#47490,#47491,
#47492,#47493,#47494,#47495,#47496,#47497,#47498,#47499,#47500),
 .UNSPECIFIED.,.F.,.F.,(4,3,3,3,3,3,3,3,4),(-399.933423392507,-399.858960751474,
-398.859313349595,-397.859665947716,-396.860018545838,-395.860371143959,
-394.86072374208,-393.861076340201,-393.650238085328),.UNSPECIFIED.);
#6440=B_SPLINE_CURVE_WITH_KNOTS('',3,(#47501,#47502,#47503,#47504,#47505,
#47506,#47507,#47508,#47509,#47510,#47511,#47512,#47513,#47514,#47515,#47516,
#47517,#47518,#47519,#47520,#47521,#47522,#47523,#47524,#47525),
 .UNSPECIFIED.,.F.,.F.,(4,3,3,3,3,3,3,3,4),(390.667534256047,390.862134134566,
391.861781536444,392.861428938323,393.861076340202,394.86072374208,395.860371143959,
396.860018545838,396.950719563226),.UNSPECIFIED.);
#6441=B_SPLINE_CURVE_WITH_KNOTS('',3,(#47530,#47531,#47532,#47533,#47534,
#47535,#47536,#47537,#47538,#47539,#47540,#47541,#47542,#47543,#47544,#47545,
#47546,#47547,#47548,#47549,#47550,#47551),.UNSPECIFIED.,.F.,.F.,(4,3,3,
3,3,3,3,4),(-406.216608699687,-405.856845162746,-404.857197760867,-403.857550358988,
-402.85790295711,-401.858255555231,-400.858608153352,-399.933423392507),
 .UNSPECIFIED.);
#6442=B_SPLINE_CURVE_WITH_KNOTS('',3,(#47552,#47553,#47554,#47555,#47556,
#47557,#47558,#47559,#47560,#47561,#47562,#47563,#47564,#47565,#47566,#47567,
#47568,#47569,#47570,#47571,#47572,#47573),.UNSPECIFIED.,.F.,.F.,(4,3,3,
3,3,3,3,4),(396.950719563226,397.859665947717,398.859313349595,399.858960751474,
400.858608153353,401.858255555231,402.85790295711,403.233904870406),
 .UNSPECIFIED.);
#6443=B_SPLINE_CURVE_WITH_KNOTS('',3,(#47578,#47579,#47580,#47581,#47582,
#47583,#47584,#47585,#47586,#47587,#47588,#47589,#47590,#47591,#47592,#47593,
#47594,#47595,#47596,#47597,#47598,#47599),.UNSPECIFIED.,.F.,.F.,(4,3,3,
3,3,3,3,4),(-412.499794006867,-411.854729574018,-410.855082172139,-409.85543477026,
-408.855787368382,-407.856139966503,-406.856492564624,-406.216608699687),
 .UNSPECIFIED.);
#6444=B_SPLINE_CURVE_WITH_KNOTS('',3,(#47600,#47601,#47602,#47603,#47604,
#47605,#47606,#47607,#47608,#47609,#47610,#47611,#47612,#47613,#47614,#47615,
#47616,#47617,#47618,#47619,#47620,#47621),.UNSPECIFIED.,.F.,.F.,(4,3,3,
3,3,3,3,4),(403.233904870406,403.857550358989,404.857197760867,405.856845162746,
406.856492564625,407.856139966503,408.855787368382,409.517090177585),
 .UNSPECIFIED.);
#6445=B_SPLINE_CURVE_WITH_KNOTS('',3,(#47626,#47627,#47628,#47629,#47630,
#47631,#47632,#47633,#47634,#47635,#47636,#47637,#47638,#47639,#47640,#47641,
#47642,#47643,#47644,#47645,#47646,#47647),.UNSPECIFIED.,.F.,.F.,(4,3,3,
3,3,3,3,4),(-418.782979314046,-417.85261398529,-416.852966583411,-415.853319181532,
-414.853671779654,-413.854024377775,-412.854376975896,-412.499794006867),
 .UNSPECIFIED.);
#6446=B_SPLINE_CURVE_WITH_KNOTS('',3,(#47648,#47649,#47650,#47651,#47652,
#47653,#47654,#47655,#47656,#47657,#47658,#47659,#47660,#47661,#47662,#47663,
#47664,#47665,#47666,#47667,#47668,#47669),.UNSPECIFIED.,.F.,.F.,(4,3,3,
3,3,3,3,4),(409.517090177585,409.855434770261,410.855082172139,411.854729574018,
412.854376975897,413.854024377775,414.853671779654,415.800275484765),
 .UNSPECIFIED.);
#6447=B_SPLINE_CURVE_WITH_KNOTS('',3,(#47674,#47675,#47676,#47677,#47678,
#47679,#47680,#47681,#47682,#47683,#47684,#47685,#47686,#47687,#47688,#47689,
#47690,#47691,#47692,#47693,#47694,#47695,#47696,#47697,#47698),
 .UNSPECIFIED.,.F.,.F.,(4,3,3,3,3,3,3,3,4),(-425.066164621226,-424.850145798441,
-423.850498396562,-422.850850994683,-421.851203592805,-420.851556190926,
-419.851908789047,-418.852261387169,-418.782979314046),.UNSPECIFIED.);
#6448=B_SPLINE_CURVE_WITH_KNOTS('',3,(#47699,#47700,#47701,#47702,#47703,
#47704,#47705,#47706,#47707,#47708,#47709,#47710,#47711,#47712,#47713,#47714,
#47715,#47716,#47717,#47718,#47719,#47720,#47721,#47722,#47723),
 .UNSPECIFIED.,.F.,.F.,(4,3,3,3,3,3,3,3,4),(415.800275484765,415.853319181533,
416.852966583412,417.85261398529,418.852261387169,419.851908789048,420.851556190926,
421.851203592805,422.083460791945),.UNSPECIFIED.);
#6449=B_SPLINE_CURVE_WITH_KNOTS('',3,(#47728,#47729,#47730,#47731,#47732,
#47733,#47734,#47735,#47736,#47737,#47738,#47739,#47740,#47741,#47742,#47743,
#47744,#47745,#47746,#47747,#47748,#47749),.UNSPECIFIED.,.F.,.F.,(4,3,3,
3,3,3,3,4),(-431.349349928405,-430.848030209713,-429.848382807834,-428.848735405955,
-427.849088004077,-426.849440602198,-425.849793200319,-425.066164621226),
 .UNSPECIFIED.);
#6450=B_SPLINE_CURVE_WITH_KNOTS('',3,(#47750,#47751,#47752,#47753,#47754,
#47755,#47756,#47757,#47758,#47759,#47760,#47761,#47762,#47763,#47764,#47765,
#47766,#47767,#47768,#47769,#47770,#47771),.UNSPECIFIED.,.F.,.F.,(4,3,3,
3,3,3,3,4),(422.083460791945,422.850850994684,423.850498396562,424.850145798441,
425.84979320032,426.849440602198,427.849088004077,428.366646099124),
 .UNSPECIFIED.);
#6451=B_SPLINE_CURVE_WITH_KNOTS('',3,(#47776,#47777,#47778,#47779,#47780,
#47781,#47782,#47783,#47784,#47785,#47786,#47787,#47788,#47789,#47790,#47791,
#47792,#47793,#47794,#47795,#47796,#47797),.UNSPECIFIED.,.F.,.F.,(4,3,3,
3,3,3,3,4),(-437.632535235585,-436.845914620985,-435.846267219106,-434.846619817227,
-433.846972415349,-432.84732501347,-431.847677611592,-431.349349928405),
 .UNSPECIFIED.);
#6452=B_SPLINE_CURVE_WITH_KNOTS('',3,(#47798,#47799,#47800,#47801,#47802,
#47803,#47804,#47805,#47806,#47807,#47808,#47809,#47810,#47811,#47812,#47813,
#47814,#47815,#47816,#47817,#47818,#47819),.UNSPECIFIED.,.F.,.F.,(4,3,3,
3,3,3,3,4),(428.366646099124,428.848735405956,429.848382807834,430.848030209713,
431.847677611592,432.84732501347,433.846972415349,434.649831406304),
 .UNSPECIFIED.);
#6453=B_SPLINE_CURVE_WITH_KNOTS('',3,(#47824,#47825,#47826,#47827,#47828,
#47829,#47830,#47831,#47832,#47833,#47834,#47835,#47836,#47837,#47838,#47839,
#47840,#47841,#47842,#47843,#47844,#47845,#47846,#47847,#47848),
 .UNSPECIFIED.,.F.,.F.,(4,3,3,3,3,3,3,3,4),(-443.915720542764,-443.843446434136,
-442.843799032257,-441.844151630378,-440.8445042285,-439.844856826621,-438.845209424742,
-437.845562022864,-437.632535235585),.UNSPECIFIED.);
#6454=B_SPLINE_CURVE_WITH_KNOTS('',3,(#47849,#47850,#47851,#47852,#47853,
#47854,#47855,#47856,#47857,#47858,#47859,#47860,#47861,#47862,#47863,#47864,
#47865,#47866,#47867,#47868,#47869,#47870,#47871,#47872,#47873),
 .UNSPECIFIED.,.F.,.F.,(4,3,3,3,3,3,3,3,4),(434.649831406304,434.846619817228,
435.846267219106,436.845914620985,437.845562022864,438.845209424743,439.844856826621,
440.8445042285,440.933016713483),.UNSPECIFIED.);
#6455=B_SPLINE_CURVE_WITH_KNOTS('',3,(#47878,#47879,#47880,#47881,#47882,
#47883,#47884,#47885,#47886,#47887,#47888,#47889,#47890,#47891,#47892,#47893,
#47894,#47895,#47896,#47897,#47898,#47899),.UNSPECIFIED.,.F.,.F.,(4,3,3,
3,3,3,3,4),(-450.198905849944,-449.841330845408,-448.841683443529,-447.84203604165,
-446.842388639772,-445.842741237893,-444.843093836014,-443.915720542764),
 .UNSPECIFIED.);
#6456=B_SPLINE_CURVE_WITH_KNOTS('',3,(#47900,#47901,#47902,#47903,#47904,
#47905,#47906,#47907,#47908,#47909,#47910,#47911,#47912,#47913,#47914,#47915,
#47916,#47917,#47918,#47919,#47920,#47921),.UNSPECIFIED.,.F.,.F.,(4,3,3,
3,3,3,3,4),(440.933016713483,441.844151630379,442.843799032257,443.843446434136,
444.843093836015,445.842741237893,446.842388639772,447.216202020663),
 .UNSPECIFIED.);
#6457=B_SPLINE_CURVE_WITH_KNOTS('',3,(#47926,#47927,#47928,#47929,#47930,
#47931,#47932,#47933,#47934,#47935,#47936,#47937,#47938,#47939,#47940,#47941,
#47942,#47943,#47944,#47945,#47946,#47947),.UNSPECIFIED.,.F.,.F.,(4,3,3,
3,3,3,3,4),(-456.482091157123,-455.83921525668,-454.839567854801,-453.839920452923,
-452.840273051044,-451.840625649165,-450.840978247287,-450.198905849944),
 .UNSPECIFIED.);
#6458=B_SPLINE_CURVE_WITH_KNOTS('',3,(#47948,#47949,#47950,#47951,#47952,
#47953,#47954,#47955,#47956,#47957,#47958,#47959,#47960,#47961,#47962,#47963,
#47964,#47965,#47966,#47967,#47968,#47969),.UNSPECIFIED.,.F.,.F.,(4,3,3,
3,3,3,3,4),(447.216202020663,447.842036041651,448.841683443529,449.841330845408,
450.840978247287,451.840625649165,452.840273051044,453.499387327842),
 .UNSPECIFIED.);
#6459=B_SPLINE_CURVE_WITH_KNOTS('',3,(#47974,#47975,#47976,#47977,#47978,
#47979,#47980,#47981,#47982,#47983,#47984,#47985,#47986,#47987,#47988,#47989,
#47990,#47991,#47992,#47993,#47994,#47995),.UNSPECIFIED.,.F.,.F.,(4,3,3,
3,3,3,3,4),(-462.765276464303,-461.837099667952,-460.837452266073,-459.837804864195,
-458.838157462316,-457.838510060437,-456.838862658559,-456.482091157123),
 .UNSPECIFIED.);
#6460=B_SPLINE_CURVE_WITH_KNOTS('',3,(#47996,#47997,#47998,#47999,#48000,
#48001,#48002,#48003,#48004,#48005,#48006,#48007,#48008,#48009,#48010,#48011,
#48012,#48013,#48014,#48015,#48016,#48017),.UNSPECIFIED.,.F.,.F.,(4,3,3,
3,3,3,3,4),(453.499387327842,453.839920452923,454.839567854801,455.83921525668,
456.838862658559,457.838510060438,458.838157462316,459.782572635022),
 .UNSPECIFIED.);
#6461=B_SPLINE_CURVE_WITH_KNOTS('',3,(#48022,#48023,#48024,#48025,#48026,
#48027,#48028,#48029,#48030,#48031,#48032,#48033,#48034,#48035,#48036,#48037,
#48038,#48039,#48040,#48041,#48042,#48043,#48044,#48045,#48046),
 .UNSPECIFIED.,.F.,.F.,(4,3,3,3,3,3,3,3,4),(-469.048461771483,-468.834631481103,
-467.834984079224,-466.835336677345,-465.835689275467,-464.836041873588,
-463.836394471709,-462.836747069831,-462.765276464303),.UNSPECIFIED.);
#6462=B_SPLINE_CURVE_WITH_KNOTS('',3,(#48047,#48048,#48049,#48050,#48051,
#48052,#48053,#48054,#48055,#48056,#48057,#48058,#48059,#48060,#48061,#48062,
#48063,#48064,#48065,#48066,#48067,#48068,#48069,#48070,#48071),
 .UNSPECIFIED.,.F.,.F.,(4,3,3,3,3,3,3,3,4),(459.782572635022,459.837804864195,
460.837452266074,461.837099667952,462.836747069831,463.83639447171,464.836041873588,
465.835689275467,466.065757942202),.UNSPECIFIED.);
#6463=B_SPLINE_CURVE_WITH_KNOTS('',3,(#48076,#48077,#48078,#48079,#48080,
#48081,#48082,#48083,#48084,#48085,#48086,#48087,#48088,#48089,#48090,#48091,
#48092,#48093,#48094,#48095,#48096,#48097),.UNSPECIFIED.,.F.,.F.,(4,3,3,
3,3,3,3,4),(-475.331647078662,-474.832515892375,-473.832868490496,-472.833221088618,
-471.833573686739,-470.83392628486,-469.834278882981,-469.048461771483),
 .UNSPECIFIED.);
#6464=B_SPLINE_CURVE_WITH_KNOTS('',3,(#48098,#48099,#48100,#48101,#48102,
#48103,#48104,#48105,#48106,#48107,#48108,#48109,#48110,#48111,#48112,#48113,
#48114,#48115,#48116,#48117,#48118,#48119),.UNSPECIFIED.,.F.,.F.,(4,3,3,
3,3,3,3,4),(466.065757942202,466.835336677346,467.834984079224,468.834631481103,
469.834278882982,470.833926284861,471.833573686739,472.348943249381),
 .UNSPECIFIED.);
#6465=B_SPLINE_CURVE_WITH_KNOTS('',3,(#48124,#48125,#48126,#48127,#48128,
#48129,#48130,#48131,#48132,#48133,#48134,#48135,#48136,#48137,#48138,#48139,
#48140,#48141,#48142,#48143,#48144,#48145),.UNSPECIFIED.,.F.,.F.,(4,3,3,
3,3,3,3,4),(-481.614832385842,-480.830400303647,-479.830752901768,-478.83110549989,
-477.831458098011,-476.831810696132,-475.832163294254,-475.331647078662),
 .UNSPECIFIED.);
#6466=B_SPLINE_CURVE_WITH_KNOTS('',3,(#48146,#48147,#48148,#48149,#48150,
#48151,#48152,#48153,#48154,#48155,#48156,#48157,#48158,#48159,#48160,#48161,
#48162,#48163,#48164,#48165,#48166,#48167),.UNSPECIFIED.,.F.,.F.,(4,3,3,
3,3,3,3,4),(472.348943249381,472.833221088618,473.832868490496,474.832515892375,
475.832163294254,476.831810696133,477.831458098011,478.632128556561),
 .UNSPECIFIED.);
#6467=B_SPLINE_CURVE_WITH_KNOTS('',3,(#48172,#48173,#48174,#48175,#48176,
#48177,#48178,#48179,#48180,#48181,#48182,#48183,#48184,#48185,#48186,#48187,
#48188,#48189,#48190,#48191,#48192,#48193,#48194,#48195,#48196),
 .UNSPECIFIED.,.F.,.F.,(4,3,3,3,3,3,3,3,4),(-487.898017693021,-487.827932116798,
-486.828284714919,-485.82863731304,-484.828989911162,-483.829342509283,
-482.829695107404,-481.830047705526,-481.614832385842),.UNSPECIFIED.);
#6468=B_SPLINE_CURVE_WITH_KNOTS('',3,(#48197,#48198,#48199,#48200,#48201,
#48202,#48203,#48204,#48205,#48206,#48207,#48208,#48209,#48210,#48211,#48212,
#48213,#48214,#48215,#48216,#48217,#48218,#48219,#48220,#48221),
 .UNSPECIFIED.,.F.,.F.,(4,3,3,3,3,3,3,3,4),(478.632128556561,478.83110549989,
479.830752901769,480.830400303647,481.830047705526,482.829695107405,483.829342509283,
484.828989911162,484.91531386374),.UNSPECIFIED.);
#6469=B_SPLINE_CURVE_WITH_KNOTS('',3,(#48226,#48227,#48228,#48229,#48230,
#48231,#48232,#48233,#48234,#48235,#48236,#48237,#48238,#48239,#48240,#48241,
#48242,#48243,#48244,#48245,#48246,#48247),.UNSPECIFIED.,.F.,.F.,(4,3,3,
3,3,3,3,4),(-494.181203000201,-493.82581652807,-492.826169126191,-491.826521724312,
-490.826874322434,-489.827226920555,-488.827579518676,-487.898017693021),
 .UNSPECIFIED.);
#6470=B_SPLINE_CURVE_WITH_KNOTS('',3,(#48248,#48249,#48250,#48251,#48252,
#48253,#48254,#48255,#48256,#48257,#48258,#48259,#48260,#48261,#48262,#48263,
#48264,#48265,#48266,#48267,#48268,#48269),.UNSPECIFIED.,.F.,.F.,(4,3,3,
3,3,3,3,4),(484.91531386374,485.828637313041,486.828284714919,487.827932116798,
488.827579518677,489.827226920556,490.826874322434,491.19849917092),
 .UNSPECIFIED.);
#6471=B_SPLINE_CURVE_WITH_KNOTS('',3,(#48274,#48275,#48276,#48277,#48278,
#48279,#48280,#48281,#48282,#48283,#48284,#48285,#48286,#48287,#48288,#48289,
#48290,#48291,#48292,#48293,#48294,#48295),.UNSPECIFIED.,.F.,.F.,(4,3,3,
3,3,3,3,4),(-500.46438830738,-499.823700939342,-498.824053537463,-497.824406135585,
-496.824758733706,-495.825111331827,-494.825463929949,-494.181203000201),
 .UNSPECIFIED.);
#6472=B_SPLINE_CURVE_WITH_KNOTS('',3,(#48296,#48297,#48298,#48299,#48300,
#48301,#48302,#48303,#48304,#48305,#48306,#48307,#48308,#48309,#48310,#48311,
#48312,#48313,#48314,#48315,#48316,#48317),.UNSPECIFIED.,.F.,.F.,(4,3,3,
3,3,3,3,4),(491.19849917092,491.826521724313,492.826169126192,493.82581652807,
494.825463929949,495.825111331828,496.824758733706,497.481684478099),
 .UNSPECIFIED.);
#6473=B_SPLINE_CURVE_WITH_KNOTS('',3,(#48322,#48323,#48324,#48325,#48326,
#48327,#48328,#48329,#48330,#48331,#48332,#48333,#48334,#48335,#48336,#48337,
#48338,#48339,#48340,#48341,#48342,#48343),.UNSPECIFIED.,.F.,.F.,(4,3,3,
3,3,3,3,4),(-506.74757361456,-505.821585350614,-504.821937948735,-503.822290546857,
-502.822643144978,-501.822995743099,-500.823348341221,-500.46438830738),
 .UNSPECIFIED.);
#6474=B_SPLINE_CURVE_WITH_KNOTS('',3,(#48344,#48345,#48346,#48347,#48348,
#48349,#48350,#48351,#48352,#48353,#48354,#48355,#48356,#48357,#48358,#48359,
#48360,#48361,#48362,#48363,#48364,#48365),.UNSPECIFIED.,.F.,.F.,(4,3,3,
3,3,3,3,4),(497.481684478099,497.824406135585,498.824053537464,499.823700939342,
500.823348341221,501.8229957431,502.822643144978,503.764869785279),
 .UNSPECIFIED.);
#6475=B_SPLINE_CURVE_WITH_KNOTS('',3,(#48370,#48371,#48372,#48373,#48374,
#48375,#48376,#48377,#48378,#48379,#48380,#48381,#48382,#48383,#48384,#48385,
#48386,#48387,#48388,#48389,#48390,#48391,#48392,#48393,#48394),
 .UNSPECIFIED.,.F.,.F.,(4,3,3,3,3,3,3,3,4),(-513.03075892174,-512.819117163765,
-511.819469761886,-510.819822360007,-509.820174958129,-508.82052755625,
-507.820880154371,-506.821232752493,-506.74757361456),.UNSPECIFIED.);
#6476=B_SPLINE_CURVE_WITH_KNOTS('',3,(#48395,#48396,#48397,#48398,#48399,
#48400,#48401,#48402,#48403,#48404,#48405,#48406,#48407,#48408,#48409,#48410,
#48411,#48412,#48413,#48414,#48415,#48416,#48417,#48418,#48419),
 .UNSPECIFIED.,.F.,.F.,(4,3,3,3,3,3,3,3,4),(503.764869785279,503.822290546857,
504.821937948736,505.821585350615,506.821232752493,507.820880154372,508.820527556251,
509.820174958129,510.048055092458),.UNSPECIFIED.);
#6477=B_SPLINE_CURVE_WITH_KNOTS('',3,(#48424,#48425,#48426,#48427,#48428,
#48429,#48430,#48431,#48432,#48433,#48434,#48435,#48436,#48437,#48438,#48439,
#48440,#48441,#48442,#48443,#48444,#48445),.UNSPECIFIED.,.F.,.F.,(4,3,3,
3,3,3,3,4),(-519.313944228919,-518.817001575037,-517.817354173158,-516.81770677128,
-515.818059369401,-514.818411967522,-513.818764565644,-513.03075892174),
 .UNSPECIFIED.);
#6478=B_SPLINE_CURVE_WITH_KNOTS('',3,(#48446,#48447,#48448,#48449,#48450,
#48451,#48452,#48453,#48454,#48455,#48456,#48457,#48458,#48459,#48460,#48461,
#48462,#48463,#48464,#48465,#48466,#48467),.UNSPECIFIED.,.F.,.F.,(4,3,3,
3,3,3,3,4),(510.048055092458,510.819822360008,511.819469761886,512.819117163765,
513.818764565644,514.818411967523,515.818059369401,516.331240399638),
 .UNSPECIFIED.);
#6479=B_SPLINE_CURVE_WITH_KNOTS('',3,(#48472,#48473,#48474,#48475,#48476,
#48477,#48478,#48479,#48480,#48481,#48482,#48483,#48484,#48485,#48486,#48487,
#48488,#48489,#48490,#48491,#48492,#48493),.UNSPECIFIED.,.F.,.F.,(4,3,3,
3,3,3,3,4),(-525.597129536099,-524.814885986309,-523.815238584431,-522.815591182552,
-521.815943780673,-520.816296378794,-519.816648976916,-519.313944228919),
 .UNSPECIFIED.);
#6480=B_SPLINE_CURVE_WITH_KNOTS('',3,(#48494,#48495,#48496,#48497,#48498,
#48499,#48500,#48501,#48502,#48503,#48504,#48505,#48506,#48507,#48508,#48509,
#48510,#48511,#48512,#48513,#48514,#48515),.UNSPECIFIED.,.F.,.F.,(4,3,3,
3,3,3,3,4),(516.331240399638,516.81770677128,517.817354173159,518.817001575037,
519.816648976916,520.816296378795,521.815943780673,522.614425706818),
 .UNSPECIFIED.);
#6481=B_SPLINE_CURVE_WITH_KNOTS('',3,(#48520,#48521,#48522,#48523,#48524,
#48525,#48526,#48527,#48528,#48529,#48530,#48531,#48532,#48533,#48534,#48535,
#48536,#48537,#48538,#48539,#48540,#48541,#48542,#48543,#48544),
 .UNSPECIFIED.,.F.,.F.,(4,3,3,3,3,3,3,3,4),(-531.880314843278,-531.81241779946,
-530.812770397581,-529.813122995703,-528.813475593824,-527.813828191945,
-526.814180790067,-525.814533388188,-525.597129536099),.UNSPECIFIED.);
#6482=B_SPLINE_CURVE_WITH_KNOTS('',3,(#48545,#48546,#48547,#48548,#48549,
#48550,#48551,#48552,#48553,#48554,#48555,#48556,#48557,#48558,#48559,#48560,
#48561,#48562,#48563,#48564,#48565,#48566,#48567,#48568,#48569),
 .UNSPECIFIED.,.F.,.F.,(4,3,3,3,3,3,3,3,4),(522.614425706818,522.815591182552,
523.815238584431,524.814885986309,525.814533388188,526.814180790067,527.813828191946,
528.813475593824,528.897611013997),.UNSPECIFIED.);
#6483=B_SPLINE_CURVE_WITH_KNOTS('',3,(#48574,#48575,#48576,#48577,#48578,
#48579,#48580,#48581,#48582,#48583,#48584,#48585,#48586,#48587,#48588,#48589,
#48590,#48591,#48592,#48593,#48594,#48595),.UNSPECIFIED.,.F.,.F.,(4,3,3,
3,3,3,3,4),(-538.163500150458,-537.810302210732,-536.810654808853,-535.811007406975,
-534.811360005096,-533.811712603217,-532.812065201339,-531.880314843278),
 .UNSPECIFIED.);
#6484=B_SPLINE_CURVE_WITH_KNOTS('',3,(#48596,#48597,#48598,#48599,#48600,
#48601,#48602,#48603,#48604,#48605,#48606,#48607,#48608,#48609,#48610,#48611,
#48612,#48613,#48614,#48615,#48616,#48617),.UNSPECIFIED.,.F.,.F.,(4,3,3,
3,3,3,3,4),(528.897611013997,529.813122995703,530.812770397582,531.81241779946,
532.812065201339,533.811712603218,534.811360005096,535.180796321177),
 .UNSPECIFIED.);
#6485=B_SPLINE_CURVE_WITH_KNOTS('',3,(#48622,#48623,#48624,#48625,#48626,
#48627,#48628,#48629,#48630,#48631,#48632,#48633,#48634,#48635,#48636,#48637,
#48638,#48639,#48640,#48641,#48642,#48643),.UNSPECIFIED.,.F.,.F.,(4,3,3,
3,3,3,3,4),(-544.446685457637,-543.808186622004,-542.808539220125,-541.808891818247,
-540.809244416368,-539.809597014489,-538.809949612611,-538.163500150458),
 .UNSPECIFIED.);
#6486=B_SPLINE_CURVE_WITH_KNOTS('',3,(#48644,#48645,#48646,#48647,#48648,
#48649,#48650,#48651,#48652,#48653,#48654,#48655,#48656,#48657,#48658,#48659,
#48660,#48661,#48662,#48663,#48664,#48665),.UNSPECIFIED.,.F.,.F.,(4,3,3,
3,3,3,3,4),(535.180796321177,535.811007406975,536.810654808854,537.810302210732,
538.809949612611,539.80959701449,540.809244416369,541.463981628356),
 .UNSPECIFIED.);
#6487=B_SPLINE_CURVE_WITH_KNOTS('',3,(#48670,#48671,#48672,#48673,#48674,
#48675,#48676,#48677,#48678,#48679,#48680,#48681,#48682,#48683,#48684,#48685,
#48686,#48687,#48688,#48689,#48690,#48691),.UNSPECIFIED.,.F.,.F.,(4,3,3,
3,3,3,3,4),(-550.729870764817,-549.806071033276,-548.806423631398,-547.806776229519,
-546.80712882764,-545.807481425761,-544.807834023883,-544.446685457637),
 .UNSPECIFIED.);
#6488=B_SPLINE_CURVE_WITH_KNOTS('',3,(#48692,#48693,#48694,#48695,#48696,
#48697,#48698,#48699,#48700,#48701,#48702,#48703,#48704,#48705,#48706,#48707,
#48708,#48709,#48710,#48711,#48712,#48713),.UNSPECIFIED.,.F.,.F.,(4,3,3,
3,3,3,3,4),(541.463981628356,541.808891818247,542.808539220126,543.808186622004,
544.807834023883,545.807481425762,546.80712882764,547.747166935536),
 .UNSPECIFIED.);
#6489=B_SPLINE_CURVE_WITH_KNOTS('',3,(#48719,#48720,#48721,#48722),
 .UNSPECIFIED.,.F.,.F.,(4,4),(562.345084992573,562.359025869153),
 .UNSPECIFIED.);
#6490=B_SPLINE_CURVE_WITH_KNOTS('',3,(#48728,#48729,#48730,#48731,#48732,
#48733,#48734,#48735,#48736,#48737,#48738,#48739,#48740,#48741,#48742,#48743,
#48744,#48745,#48746,#48747,#48748,#48749),.UNSPECIFIED.,.F.,.F.,(4,3,3,
3,3,3,3,4),(556.061899685393,556.423048251639,557.422695653518,558.422343055396,
559.421990457275,560.421637859154,561.421285261032,562.345084992573),
 .UNSPECIFIED.);
#6491=B_SPLINE_CURVE_WITH_KNOTS('',3,(#48752,#48753,#48754,#48755,#48756,
#48757,#48758,#48759,#48760),.UNSPECIFIED.,.F.,.F.,(4,1,1,1,1,1,4),(556.061899685393,
556.121508979378,557.121156381257,558.120803783136,559.120451185014,560.120098586893,
561.119745988772),.UNSPECIFIED.);
#6492=B_SPLINE_CURVE_WITH_KNOTS('',3,(#48765,#48766,#48767,#48768,#48769,
#48770,#48771,#48772,#48773,#48774,#48775,#48776,#48777,#48778,#48779,#48780,
#48781,#48782,#48783,#48784,#48785,#48786),.UNSPECIFIED.,.F.,.F.,(4,3,3,
3,3,3,3,4),(549.778714378214,550.425163840367,551.424811242246,552.424458644124,
553.424106046003,554.423753447882,555.42340084976,556.061899685393),
 .UNSPECIFIED.);
#6493=B_SPLINE_CURVE_WITH_KNOTS('',3,(#48787,#48788,#48789,#48790,#48791,
#48792,#48793,#48794,#48795,#48796,#48797,#48798,#48799,#48800,#48801,#48802,
#48803,#48804,#48805,#48806,#48807,#48808),.UNSPECIFIED.,.F.,.F.,(4,3,3,
3,3,3,3,4),(549.778714378214,550.123624568106,551.123271969985,552.122919371864,
553.122566773742,554.122214175621,555.1218615775,556.061899685393),
 .UNSPECIFIED.);
#6494=B_SPLINE_CURVE_WITH_KNOTS('',3,(#48813,#48814,#48815,#48816,#48817,
#48818,#48819,#48820,#48821,#48822,#48823,#48824,#48825,#48826,#48827,#48828,
#48829,#48830,#48831,#48832,#48833,#48834),.UNSPECIFIED.,.F.,.F.,(4,3,3,
3,3,3,3,4),(543.495529071034,544.427279429095,545.426926830973,546.426574232852,
547.426221634731,548.42586903661,549.425516438488,549.778714378214),
 .UNSPECIFIED.);
#6495=B_SPLINE_CURVE_WITH_KNOTS('',3,(#48835,#48836,#48837,#48838,#48839,
#48840,#48841,#48842,#48843,#48844,#48845,#48846,#48847,#48848,#48849,#48850,
#48851,#48852,#48853,#48854,#48855,#48856),.UNSPECIFIED.,.F.,.F.,(4,3,3,
3,3,3,3,4),(543.495529071034,544.125740156834,545.125387558713,546.125034960591,
547.12468236247,548.124329764349,549.123977166228,549.778714378214),
 .UNSPECIFIED.);
#6496=B_SPLINE_CURVE_WITH_KNOTS('',3,(#48861,#48862,#48863,#48864,#48865,
#48866,#48867,#48868,#48869,#48870,#48871),.UNSPECIFIED.,.F.,.F.,(4,1,1,
1,1,1,1,1,4),(537.212343763854,537.429747615944,538.429395017823,539.429042419701,
540.42868982158,541.428337223459,542.427984625337,543.427632027216,543.495529071034),
 .UNSPECIFIED.);
#6497=B_SPLINE_CURVE_WITH_KNOTS('',3,(#48872,#48873,#48874,#48875,#48876,
#48877,#48878,#48879,#48880,#48881),.UNSPECIFIED.,.F.,.F.,(4,1,1,1,1,1,
1,4),(537.212343763855,538.127855745562,539.127503147441,540.127150549319,
541.126797951198,542.126445353077,543.126092754955,543.495529071034),
 .UNSPECIFIED.);
#6498=B_SPLINE_CURVE_WITH_KNOTS('',3,(#48886,#48887,#48888,#48889,#48890,
#48891,#48892,#48893,#48894,#48895),.UNSPECIFIED.,.F.,.F.,(4,1,1,1,1,1,
1,4),(530.929158456675,531.431863204672,532.431510606551,533.431158008429,
534.430805410308,535.430452812187,536.430100214065,537.212343763854),
 .UNSPECIFIED.);
#6499=B_SPLINE_CURVE_WITH_KNOTS('',3,(#48896,#48897,#48898,#48899,#48900,
#48901,#48902,#48903,#48904,#48905,#48906),.UNSPECIFIED.,.F.,.F.,(4,1,1,
1,1,1,1,1,4),(530.929158456675,531.130323932411,532.12997133429,533.129618736168,
534.129266138047,535.128913539926,536.128560941805,537.128208343683,537.212343763855),
 .UNSPECIFIED.);
#6500=B_SPLINE_CURVE_WITH_KNOTS('',3,(#48911,#48912,#48913,#48914,#48915,
#48916,#48917,#48918,#48919,#48920),.UNSPECIFIED.,.F.,.F.,(4,1,1,1,1,1,
1,4),(524.645973149495,525.4339787934,526.433626195278,527.433273597157,
528.432920999036,529.432568400914,530.432215802793,530.929158456675),
 .UNSPECIFIED.);
#6501=B_SPLINE_CURVE_WITH_KNOTS('',3,(#48921,#48922,#48923,#48924,#48925,
#48926,#48927,#48928,#48929,#48930),.UNSPECIFIED.,.F.,.F.,(4,1,1,1,1,1,
1,4),(524.645973149496,525.132439521139,526.132086923018,527.131734324896,
528.131381726775,529.131029128654,530.130676530532,530.929158456675),
 .UNSPECIFIED.);
#6502=B_SPLINE_CURVE_WITH_KNOTS('',3,(#48935,#48936,#48937,#48938,#48939,
#48940,#48941,#48942,#48943,#48944,#48945),.UNSPECIFIED.,.F.,.F.,(4,1,1,
1,1,1,1,1,4),(518.362787842316,518.436446980249,519.436094382128,520.435741784006,
521.435389185885,522.435036587764,523.434683989642,524.434331391521,524.645973149495),
 .UNSPECIFIED.);
#6503=B_SPLINE_CURVE_WITH_KNOTS('',3,(#48946,#48947,#48948,#48949,#48950,
#48951,#48952,#48953,#48954,#48955),.UNSPECIFIED.,.F.,.F.,(4,1,1,1,1,1,
1,4),(518.362787842316,519.134555109867,520.134202511746,521.133849913624,
522.133497315503,523.133144717382,524.13279211926,524.645973149496),
 .UNSPECIFIED.);
#6504=B_SPLINE_CURVE_WITH_KNOTS('',3,(#48960,#48961,#48962,#48963,#48964,
#48965,#48966,#48967,#48968,#48969),.UNSPECIFIED.,.F.,.F.,(4,1,1,1,1,1,
1,4),(512.079602535136,512.438562568977,513.438209970855,514.437857372734,
515.437504774613,516.437152176492,517.43679957837,518.362787842316),
 .UNSPECIFIED.);
#6505=B_SPLINE_CURVE_WITH_KNOTS('',3,(#48970,#48971,#48972,#48973,#48974,
#48975,#48976,#48977,#48978,#48979,#48980,#48981,#48982,#48983,#48984,#48985,
#48986,#48987,#48988,#48989,#48990,#48991,#48992,#48993,#48994),
 .UNSPECIFIED.,.F.,.F.,(4,3,3,3,3,3,3,3,4),(512.079602535136,512.137023296716,
513.136670698595,514.136318100474,515.135965502352,516.135612904231,517.13526030611,
518.134907707988,518.362787842316),.UNSPECIFIED.);
#6506=B_SPLINE_CURVE_WITH_KNOTS('',3,(#48999,#49000,#49001,#49002,#49003,
#49004,#49005,#49006,#49007,#49008),.UNSPECIFIED.,.F.,.F.,(4,1,1,1,1,1,
1,4),(505.796417227957,506.440678157705,507.440325559583,508.439972961462,
509.439620363341,510.439267765219,511.438915167098,512.079602535136),
 .UNSPECIFIED.);
#6507=B_SPLINE_CURVE_WITH_KNOTS('',3,(#49009,#49010,#49011,#49012,#49013,
#49014,#49015,#49016,#49017,#49018,#49019,#49020,#49021,#49022,#49023,#49024,
#49025,#49026,#49027,#49028,#49029,#49030),.UNSPECIFIED.,.F.,.F.,(4,3,3,
3,3,3,3,4),(505.796417227957,506.139138885444,507.138786287323,508.138433689201,
509.13808109108,510.137728492959,511.137375894838,512.079602535136),
 .UNSPECIFIED.);
#6508=B_SPLINE_CURVE_WITH_KNOTS('',3,(#49035,#49036,#49037,#49038,#49039,
#49040,#49041,#49042,#49043,#49044),.UNSPECIFIED.,.F.,.F.,(4,1,1,1,1,1,
1,4),(499.513231920777,500.442793746433,501.442441148311,502.44208855019,
503.441735952069,504.441383353947,505.441030755826,505.796417227957),
 .UNSPECIFIED.);
#6509=B_SPLINE_CURVE_WITH_KNOTS('',3,(#49045,#49046,#49047,#49048,#49049,
#49050,#49051,#49052,#49053,#49054),.UNSPECIFIED.,.F.,.F.,(4,1,1,1,1,1,
1,4),(499.513231920777,500.141254474172,501.140901876051,502.140549277929,
503.140196679808,504.139844081687,505.139491483565,505.796417227957),
 .UNSPECIFIED.);
#6510=B_SPLINE_CURVE_WITH_KNOTS('',3,(#49059,#49060,#49061,#49062,#49063,
#49064,#49065,#49066,#49067,#49068,#49069),.UNSPECIFIED.,.F.,.F.,(4,1,1,
1,1,1,1,1,4),(493.230046613597,493.445261933282,494.44490933516,495.444556737039,
496.444204138918,497.443851540797,498.443498942675,499.443146344554,499.513231920777),
 .UNSPECIFIED.);
#6511=B_SPLINE_CURVE_WITH_KNOTS('',3,(#49070,#49071,#49072,#49073,#49074,
#49075,#49076,#49077,#49078,#49079),.UNSPECIFIED.,.F.,.F.,(4,1,1,1,1,1,
1,4),(493.230046613598,494.1433700629,495.143017464778,496.142664866657,
497.142312268536,498.141959670415,499.141607072293,499.513231920777),
 .UNSPECIFIED.);
#6512=B_SPLINE_CURVE_WITH_KNOTS('',3,(#49084,#49085,#49086,#49087,#49088,
#49089,#49090,#49091,#49092,#49093),.UNSPECIFIED.,.F.,.F.,(4,1,1,1,1,1,
1,4),(486.946861306418,487.44737752201,488.447024923888,489.446672325767,
490.446319727646,491.445967129524,492.445614531403,493.230046613597),
 .UNSPECIFIED.);
#6513=B_SPLINE_CURVE_WITH_KNOTS('',3,(#49094,#49095,#49096,#49097,#49098,
#49099,#49100,#49101,#49102,#49103,#49104),.UNSPECIFIED.,.F.,.F.,(4,1,1,
1,1,1,1,1,4),(486.946861306418,487.145838249749,488.145485651628,489.145133053506,
490.144780455385,491.144427857264,492.144075259142,493.143722661021,493.230046613598),
 .UNSPECIFIED.);
#6514=B_SPLINE_CURVE_WITH_KNOTS('',3,(#49109,#49110,#49111,#49112,#49113,
#49114,#49115,#49116,#49117,#49118),.UNSPECIFIED.,.F.,.F.,(4,1,1,1,1,1,
1,4),(480.663675999238,481.449493110738,482.449140512616,483.448787914495,
484.448435316374,485.448082718252,486.447730120131,486.946861306418),
 .UNSPECIFIED.);
#6515=B_SPLINE_CURVE_WITH_KNOTS('',3,(#49119,#49120,#49121,#49122,#49123,
#49124,#49125,#49126,#49127,#49128),.UNSPECIFIED.,.F.,.F.,(4,1,1,1,1,1,
1,4),(480.663675999239,481.147953838477,482.147601240356,483.147248642234,
484.146896044113,485.146543445992,486.14619084787,486.946861306418),
 .UNSPECIFIED.);
#6516=B_SPLINE_CURVE_WITH_KNOTS('',3,(#49133,#49134,#49135,#49136,#49137,
#49138,#49139,#49140,#49141,#49142,#49143),.UNSPECIFIED.,.F.,.F.,(4,1,1,
1,1,1,1,1,4),(474.380490692059,474.451961297587,475.451608699465,476.451256101344,
477.450903503223,478.450550905102,479.45019830698,480.449845708859,480.663675999238),
 .UNSPECIFIED.);
#6517=B_SPLINE_CURVE_WITH_KNOTS('',3,(#49144,#49145,#49146,#49147,#49148,
#49149,#49150,#49151,#49152,#49153),.UNSPECIFIED.,.F.,.F.,(4,1,1,1,1,1,
1,4),(474.380490692059,475.150069427205,476.149716829084,477.149364230962,
478.149011632841,479.14865903472,480.148306436598,480.663675999239),
 .UNSPECIFIED.);
#6518=B_SPLINE_CURVE_WITH_KNOTS('',3,(#49158,#49159,#49160,#49161,#49162,
#49163,#49164,#49165,#49166,#49167),.UNSPECIFIED.,.F.,.F.,(4,1,1,1,1,1,
1,4),(468.097305384879,468.454076886315,469.453724288193,470.453371690072,
471.453019091951,472.452666493829,473.452313895708,474.380490692059),
 .UNSPECIFIED.);
#6519=B_SPLINE_CURVE_WITH_KNOTS('',3,(#49168,#49169,#49170,#49171,#49172,
#49173,#49174,#49175,#49176,#49177,#49178),.UNSPECIFIED.,.F.,.F.,(4,1,1,
1,1,1,1,1,4),(468.09730538488,468.152537614054,469.152185015933,470.151832417811,
471.15147981969,472.151127221569,473.150774623447,474.150422025326,474.380490692059),
 .UNSPECIFIED.);
#6520=B_SPLINE_CURVE_WITH_KNOTS('',3,(#49183,#49184,#49185,#49186,#49187,
#49188,#49189,#49190,#49191,#49192,#49193,#49194,#49195,#49196,#49197,#49198,
#49199,#49200,#49201,#49202,#49203,#49204),.UNSPECIFIED.,.F.,.F.,(4,3,3,
3,3,3,3,4),(461.814120077699,462.456192475043,463.455839876921,464.4554872788,
465.455134680679,466.454782082557,467.454429484436,468.097305384879),
 .UNSPECIFIED.);
#6521=B_SPLINE_CURVE_WITH_KNOTS('',3,(#49205,#49206,#49207,#49208,#49209,
#49210,#49211,#49212,#49213,#49214),.UNSPECIFIED.,.F.,.F.,(4,1,1,1,1,1,
1,4),(461.8141200777,462.154653202782,463.154300604661,464.153948006539,
465.153595408418,466.153242810297,467.152890212175,468.09730538488),
 .UNSPECIFIED.);
#6522=B_SPLINE_CURVE_WITH_KNOTS('',3,(#49219,#49220,#49221,#49222,#49223,
#49224,#49225,#49226,#49227,#49228,#49229,#49230,#49231,#49232,#49233,#49234,
#49235,#49236,#49237,#49238,#49239,#49240),.UNSPECIFIED.,.F.,.F.,(4,3,3,
3,3,3,3,4),(455.53093477052,456.458308063771,457.457955465649,458.457602867528,
459.457250269407,460.456897671285,461.456545073164,461.814120077699),
 .UNSPECIFIED.);
#6523=B_SPLINE_CURVE_WITH_KNOTS('',3,(#49241,#49242,#49243,#49244,#49245,
#49246,#49247,#49248,#49249,#49250),.UNSPECIFIED.,.F.,.F.,(4,1,1,1,1,1,
1,4),(455.53093477052,456.15676879151,457.156416193389,458.156063595267,
459.155710997146,460.155358399025,461.155005800903,461.8141200777),
 .UNSPECIFIED.);
#6524=B_SPLINE_CURVE_WITH_KNOTS('',3,(#49255,#49256,#49257,#49258,#49259,
#49260,#49261,#49262,#49263,#49264,#49265),.UNSPECIFIED.,.F.,.F.,(4,1,1,
1,1,1,1,1,4),(449.24774946334,449.46077625062,450.460423652498,451.460071054377,
452.459718456256,453.459365858134,454.459013260013,455.458660661892,455.53093477052),
 .UNSPECIFIED.);
#6525=B_SPLINE_CURVE_WITH_KNOTS('',3,(#49266,#49267,#49268,#49269,#49270,
#49271,#49272,#49273,#49274,#49275),.UNSPECIFIED.,.F.,.F.,(4,1,1,1,1,1,
1,4),(449.247749463341,450.158884380238,451.158531782116,452.158179183995,
453.157826585874,454.157473987752,455.157121389631,455.53093477052),
 .UNSPECIFIED.);
#6526=B_SPLINE_CURVE_WITH_KNOTS('',3,(#49280,#49281,#49282,#49283,#49284,
#49285,#49286,#49287,#49288,#49289),.UNSPECIFIED.,.F.,.F.,(4,1,1,1,1,1,
1,4),(442.964564156161,443.462891839348,444.462539241226,445.462186643105,
446.461834044984,447.461481446862,448.461128848741,449.24774946334),
 .UNSPECIFIED.);
#6527=B_SPLINE_CURVE_WITH_KNOTS('',3,(#49290,#49291,#49292,#49293,#49294,
#49295,#49296,#49297,#49298,#49299,#49300),.UNSPECIFIED.,.F.,.F.,(4,1,1,
1,1,1,1,1,4),(442.964564156161,443.161352567087,444.160999968966,445.160647370844,
446.160294772723,447.159942174602,448.15958957648,449.159236978359,449.247749463341),
 .UNSPECIFIED.);
#6528=B_SPLINE_CURVE_WITH_KNOTS('',3,(#49305,#49306,#49307,#49308,#49309,
#49310,#49311,#49312,#49313,#49314),.UNSPECIFIED.,.F.,.F.,(4,1,1,1,1,1,
1,4),(436.681378848981,437.465007428075,438.464654829954,439.464302231833,
440.463949633712,441.46359703559,442.463244437469,442.964564156161),
 .UNSPECIFIED.);
#6529=B_SPLINE_CURVE_WITH_KNOTS('',3,(#49315,#49316,#49317,#49318,#49319,
#49320,#49321,#49322,#49323,#49324),.UNSPECIFIED.,.F.,.F.,(4,1,1,1,1,1,
1,4),(436.681378848982,437.163468155815,438.163115557694,439.162762959572,
440.162410361451,441.16205776333,442.161705165208,442.964564156161),
 .UNSPECIFIED.);
#6530=B_SPLINE_CURVE_WITH_KNOTS('',3,(#49329,#49330,#49331,#49332,#49333,
#49334,#49335,#49336,#49337,#49338,#49339),.UNSPECIFIED.,.F.,.F.,(4,1,1,
1,1,1,1,1,4),(430.398193541802,430.467475614925,431.467123016803,432.466770418682,
433.466417820561,434.466065222439,435.465712624318,436.465360026197,436.681378848981),
 .UNSPECIFIED.);
#6531=B_SPLINE_CURVE_WITH_KNOTS('',3,(#49340,#49341,#49342,#49343,#49344,
#49345,#49346,#49347,#49348,#49349),.UNSPECIFIED.,.F.,.F.,(4,1,1,1,1,1,
1,4),(430.398193541802,431.165583744543,432.165231146421,433.1648785483,
434.164525950179,435.164173352057,436.163820753936,436.681378848982),
 .UNSPECIFIED.);
#6532=B_SPLINE_CURVE_WITH_KNOTS('',3,(#49354,#49355,#49356,#49357,#49358,
#49359,#49360,#49361,#49362,#49363),.UNSPECIFIED.,.F.,.F.,(4,1,1,1,1,1,
1,4),(424.115008234622,424.469591203653,425.469238605531,426.46888600741,
427.468533409289,428.468180811167,429.467828213046,430.398193541802),
 .UNSPECIFIED.);
#6533=B_SPLINE_CURVE_WITH_KNOTS('',3,(#49364,#49365,#49366,#49367,#49368,
#49369,#49370,#49371,#49372,#49373,#49374),.UNSPECIFIED.,.F.,.F.,(4,1,1,
1,1,1,1,1,4),(424.115008234623,424.168051931392,425.167699333271,426.167346735149,
427.166994137028,428.166641538907,429.166288940785,430.165936342664,430.398193541802),
 .UNSPECIFIED.);
#6534=B_SPLINE_CURVE_WITH_KNOTS('',3,(#49379,#49380,#49381,#49382,#49383,
#49384,#49385,#49386,#49387,#49388),.UNSPECIFIED.,.F.,.F.,(4,1,1,1,1,1,
1,4),(417.831822927443,418.47170679238,419.471354194259,420.471001596138,
421.470648998017,422.470296399895,423.469943801774,424.115008234622),
 .UNSPECIFIED.);
#6535=B_SPLINE_CURVE_WITH_KNOTS('',3,(#49389,#49390,#49391,#49392,#49393,
#49394,#49395,#49396,#49397,#49398),.UNSPECIFIED.,.F.,.F.,(4,1,1,1,1,1,
1,4),(417.831822927443,418.17016752012,419.169814921998,420.169462323877,
421.169109725756,422.168757127635,423.168404529513,424.115008234623),
 .UNSPECIFIED.);
#6536=B_SPLINE_CURVE_WITH_KNOTS('',3,(#49403,#49404,#49405,#49406,#49407,
#49408,#49409,#49410,#49411,#49412),.UNSPECIFIED.,.F.,.F.,(4,1,1,1,1,1,
1,4),(411.548637620263,412.473822381108,413.473469782987,414.473117184866,
415.472764586744,416.472411988623,417.472059390502,417.831822927443),
 .UNSPECIFIED.);
#6537=B_SPLINE_CURVE_WITH_KNOTS('',3,(#49413,#49414,#49415,#49416,#49417,
#49418,#49419,#49420,#49421,#49422),.UNSPECIFIED.,.F.,.F.,(4,1,1,1,1,1,
1,4),(411.548637620263,412.172283108848,413.171930510726,414.171577912605,
415.171225314484,416.170872716362,417.170520118241,417.831822927443),
 .UNSPECIFIED.);
#6538=B_SPLINE_CURVE_WITH_KNOTS('',3,(#49427,#49428,#49429,#49430,#49431,
#49432,#49433,#49434,#49435,#49436,#49437),.UNSPECIFIED.,.F.,.F.,(4,1,1,
1,1,1,1,1,4),(405.265452313084,405.476290567958,406.475937969836,407.475585371715,
408.475232773594,409.474880175472,410.474527577351,411.47417497923,411.548637620263),
 .UNSPECIFIED.);
#6539=B_SPLINE_CURVE_WITH_KNOTS('',3,(#49438,#49439,#49440,#49441,#49442,
#49443,#49444,#49445,#49446,#49447),.UNSPECIFIED.,.F.,.F.,(4,1,1,1,1,1,
1,4),(405.265452313084,406.174398697576,407.174046099454,408.173693501333,
409.173340903212,410.17298830509,411.172635706969,411.548637620263),
 .UNSPECIFIED.);
#6540=B_SPLINE_CURVE_WITH_KNOTS('',3,(#49452,#49453,#49454,#49455,#49456,
#49457,#49458,#49459,#49460,#49461),.UNSPECIFIED.,.F.,.F.,(4,1,1,1,1,1,
1,4),(398.982267005904,399.478406156685,400.478053558564,401.477700960443,
402.477348362322,403.4769957642,404.476643166079,405.265452313084),
 .UNSPECIFIED.);
#6541=B_SPLINE_CURVE_WITH_KNOTS('',3,(#49462,#49463,#49464,#49465,#49466,
#49467,#49468,#49469,#49470,#49471,#49472),.UNSPECIFIED.,.F.,.F.,(4,1,1,
1,1,1,1,1,4),(398.982267005904,399.176866884425,400.176514286303,401.176161688182,
402.175809090061,403.17545649194,404.175103893818,405.174751295697,405.265452313084),
 .UNSPECIFIED.);
#6542=B_SPLINE_CURVE_WITH_KNOTS('',3,(#49477,#49478,#49479,#49480,#49481,
#49482,#49483,#49484,#49485,#49486),.UNSPECIFIED.,.F.,.F.,(4,1,1,1,1,1,
1,4),(392.699081698724,393.480521745413,394.480169147292,395.479816549171,
396.479463951049,397.479111352928,398.478758754807,398.982267005904),
 .UNSPECIFIED.);
#6543=B_SPLINE_CURVE_WITH_KNOTS('',3,(#49487,#49488,#49489,#49490,#49491,
#49492,#49493,#49494,#49495,#49496),.UNSPECIFIED.,.F.,.F.,(4,1,1,1,1,1,
1,4),(392.699081698725,393.178982473153,394.178629875031,395.17827727691,
396.177924678789,397.177572080667,398.177219482546,398.982267005904),
 .UNSPECIFIED.);
#6544=B_SPLINE_CURVE_WITH_KNOTS('',3,(#49501,#49502,#49503,#49504,#49505,
#49506,#49507,#49508,#49509,#49510,#49511),.UNSPECIFIED.,.F.,.F.,(4,1,1,
1,1,1,1,1,4),(386.415896391545,386.482989932263,387.482637334141,388.48228473602,
389.481932137899,390.481579539777,391.481226941656,392.480874343535,392.699081698724),
 .UNSPECIFIED.);
#6545=B_SPLINE_CURVE_WITH_KNOTS('',3,(#49512,#49513,#49514,#49515,#49516,
#49517,#49518,#49519,#49520,#49521),.UNSPECIFIED.,.F.,.F.,(4,1,1,1,1,1,
1,4),(386.415896391545,387.181098061881,388.180745463759,389.180392865638,
390.180040267517,391.179687669395,392.179335071274,392.699081698725),
 .UNSPECIFIED.);
#6546=B_SPLINE_CURVE_WITH_KNOTS('',3,(#49526,#49527,#49528,#49529,#49530,
#49531,#49532,#49533,#49534,#49535),.UNSPECIFIED.,.F.,.F.,(4,1,1,1,1,1,
1,4),(380.132711084365,380.48510552099,381.484752922869,382.484400324748,
383.484047726626,384.483695128505,385.483342530384,386.415896391545),
 .UNSPECIFIED.);
#6547=B_SPLINE_CURVE_WITH_KNOTS('',3,(#49536,#49537,#49538,#49539,#49540,
#49541,#49542,#49543,#49544,#49545,#49546),.UNSPECIFIED.,.F.,.F.,(4,1,1,
1,1,1,1,1,4),(380.132711084366,380.18356624873,381.183213650608,382.182861052487,
383.182508454366,384.182155856244,385.181803258123,386.181450660002,386.415896391545),
 .UNSPECIFIED.);
#6548=B_SPLINE_CURVE_WITH_KNOTS('',3,(#49551,#49552,#49553,#49554,#49555,
#49556,#49557,#49558,#49559,#49560),.UNSPECIFIED.,.F.,.F.,(4,1,1,1,1,1,
1,4),(373.849525777186,374.487221109718,375.486868511597,376.486515913476,
377.486163315354,378.485810717233,379.485458119112,380.132711084365),
 .UNSPECIFIED.);
#6549=B_SPLINE_CURVE_WITH_KNOTS('',3,(#49561,#49562,#49563,#49564,#49565,
#49566,#49567,#49568,#49569,#49570),.UNSPECIFIED.,.F.,.F.,(4,1,1,1,1,1,
1,4),(373.849525777186,374.185681837458,375.185329239336,376.184976641215,
377.184624043094,378.184271444972,379.183918846851,380.132711084366),
 .UNSPECIFIED.);
#6550=B_SPLINE_CURVE_WITH_KNOTS('',3,(#49575,#49576,#49577,#49578,#49579,
#49580,#49581,#49582,#49583,#49584),.UNSPECIFIED.,.F.,.F.,(4,1,1,1,1,1,
1,4),(367.566340470006,368.489336698446,369.488984100325,370.488631502204,
371.488278904082,372.487926305961,373.48757370784,373.849525777186),
 .UNSPECIFIED.);
#6551=B_SPLINE_CURVE_WITH_KNOTS('',3,(#49585,#49586,#49587,#49588,#49589,
#49590,#49591,#49592,#49593,#49594),.UNSPECIFIED.,.F.,.F.,(4,1,1,1,1,1,
1,4),(367.566340470006,368.187797426186,369.187444828064,370.187092229943,
371.186739631822,372.1863870337,373.186034435579,373.849525777186),
 .UNSPECIFIED.);
#6552=B_SPLINE_CURVE_WITH_KNOTS('',3,(#49599,#49600,#49601,#49602,#49603,
#49604,#49605,#49606,#49607,#49608,#49609),.UNSPECIFIED.,.F.,.F.,(4,1,1,
1,1,1,1,1,4),(361.283155162827,361.491804885295,362.491452287174,363.491099689053,
364.490747090932,365.49039449281,366.490041894689,367.489689296568,367.566340470006),
 .UNSPECIFIED.);
#6553=B_SPLINE_CURVE_WITH_KNOTS('',3,(#49610,#49611,#49612,#49613,#49614,
#49615,#49616,#49617,#49618,#49619),.UNSPECIFIED.,.F.,.F.,(4,1,1,1,1,1,
1,4),(361.283155162827,362.189913014913,363.189560416792,364.189207818671,
365.188855220549,366.188502622428,367.188150024307,367.566340470006),
 .UNSPECIFIED.);
#6554=B_SPLINE_CURVE_WITH_KNOTS('',3,(#49624,#49625,#49626,#49627,#49628,
#49629,#49630,#49631,#49632,#49633),.UNSPECIFIED.,.F.,.F.,(4,1,1,1,1,1,
1,4),(354.999969855647,355.493920474023,356.493567875902,357.493215277781,
358.492862679659,359.492510081538,360.492157483417,361.283155162827),
 .UNSPECIFIED.);
#6555=B_SPLINE_CURVE_WITH_KNOTS('',3,(#49634,#49635,#49636,#49637,#49638,
#49639,#49640,#49641,#49642,#49643,#49644),.UNSPECIFIED.,.F.,.F.,(4,1,1,
1,1,1,1,1,4),(354.999969855647,355.192381201763,356.192028603641,357.19167600552,
358.191323407399,359.190970809277,360.190618211156,361.190265613035,361.283155162827),
 .UNSPECIFIED.);
#6556=B_SPLINE_CURVE_WITH_KNOTS('',3,(#49649,#49650,#49651,#49652,#49653,
#49654,#49655,#49656,#49657,#49658),.UNSPECIFIED.,.F.,.F.,(4,1,1,1,1,1,
1,4),(348.716784548467,349.496036062751,350.49568346463,351.495330866509,
352.494978268387,353.494625670266,354.494273072145,354.999969855647),
 .UNSPECIFIED.);
#6557=B_SPLINE_CURVE_WITH_KNOTS('',3,(#49659,#49660,#49661,#49662,#49663,
#49664,#49665,#49666,#49667,#49668),.UNSPECIFIED.,.F.,.F.,(4,1,1,1,1,1,
1,4),(348.716784548468,349.194496790491,350.194144192369,351.193791594248,
352.193438996127,353.193086398005,354.192733799884,354.999969855647),
 .UNSPECIFIED.);
#6558=B_SPLINE_CURVE_WITH_KNOTS('',3,(#49673,#49674,#49675,#49676,#49677,
#49678,#49679,#49680,#49681,#49682,#49683),.UNSPECIFIED.,.F.,.F.,(4,1,1,
1,1,1,1,1,4),(342.433599241288,342.498504249601,343.498151651479,344.497799053358,
345.497446455237,346.497093857115,347.496741258994,348.496388660873,348.716784548467),
 .UNSPECIFIED.);
#6559=B_SPLINE_CURVE_WITH_KNOTS('',3,(#49684,#49685,#49686,#49687,#49688,
#49689,#49690,#49691,#49692,#49693),.UNSPECIFIED.,.F.,.F.,(4,1,1,1,1,1,
1,4),(342.433599241288,343.196612379218,344.196259781097,345.195907182976,
346.195554584855,347.195201986733,348.194849388612,348.716784548468),
 .UNSPECIFIED.);
#6560=B_SPLINE_CURVE_WITH_KNOTS('',3,(#49698,#49699,#49700,#49701,#49702,
#49703,#49704,#49705,#49706,#49707),.UNSPECIFIED.,.F.,.F.,(4,1,1,1,1,1,
1,4),(336.150413934108,336.500619838328,337.500267240207,338.499914642086,
339.499562043964,340.499209445843,341.498856847722,342.433599241288),
 .UNSPECIFIED.);
#6561=B_SPLINE_CURVE_WITH_KNOTS('',3,(#49708,#49709,#49710,#49711,#49712,
#49713,#49714,#49715,#49716,#49717,#49718),.UNSPECIFIED.,.F.,.F.,(4,1,1,
1,1,1,1,1,4),(336.150413934109,336.199080566068,337.198727967946,338.198375369825,
339.198022771704,340.197670173582,341.197317575461,342.19696497734,342.433599241288),
 .UNSPECIFIED.);
#6562=B_SPLINE_CURVE_WITH_KNOTS('',3,(#49723,#49724,#49725,#49726,#49727,
#49728,#49729,#49730,#49731,#49732),.UNSPECIFIED.,.F.,.F.,(4,1,1,1,1,1,
1,4),(329.867228626929,330.502735427056,331.502382828935,332.502030230814,
333.501677632692,334.501325034571,335.50097243645,336.150413934108),
 .UNSPECIFIED.);
#6563=B_SPLINE_CURVE_WITH_KNOTS('',3,(#49733,#49734,#49735,#49736,#49737,
#49738,#49739,#49740,#49741,#49742),.UNSPECIFIED.,.F.,.F.,(4,1,1,1,1,1,
1,4),(329.867228626929,330.201196154796,331.200843556674,332.200490958553,
333.200138360432,334.19978576231,335.199433164189,336.150413934109),
 .UNSPECIFIED.);
#6564=B_SPLINE_CURVE_WITH_KNOTS('',3,(#49747,#49748,#49749,#49750,#49751,
#49752,#49753,#49754,#49755,#49756),.UNSPECIFIED.,.F.,.F.,(4,1,1,1,1,1,
1,4),(323.584043319749,324.504851015784,325.504498417663,326.504145819542,
327.50379322142,328.503440623299,329.503088025178,329.867228626929),
 .UNSPECIFIED.);
#6565=B_SPLINE_CURVE_WITH_KNOTS('',3,(#49757,#49758,#49759,#49760,#49761,
#49762,#49763,#49764,#49765,#49766),.UNSPECIFIED.,.F.,.F.,(4,1,1,1,1,1,
1,4),(323.58404331975,324.203311743523,325.202959145402,326.202606547281,
327.20225394916,328.201901351038,329.201548752917,329.867228626929),
 .UNSPECIFIED.);
#6566=B_SPLINE_CURVE_WITH_KNOTS('',3,(#49771,#49772,#49773,#49774,#49775,
#49776,#49777,#49778,#49779,#49780,#49781),.UNSPECIFIED.,.F.,.F.,(4,1,1,
1,1,1,1,1,4),(317.30085801257,317.507319202633,318.506966604512,319.506614006391,
320.506261408269,321.505908810148,322.505556212027,323.505203613906,323.584043319749),
 .UNSPECIFIED.);
#6567=B_SPLINE_CURVE_WITH_KNOTS('',3,(#49782,#49783,#49784,#49785,#49786,
#49787,#49788,#49789,#49790,#49791),.UNSPECIFIED.,.F.,.F.,(4,1,1,1,1,1,
1,4),(317.30085801257,318.205427332251,319.20507473413,320.204722136009,
321.204369537887,322.204016939766,323.203664341645,323.58404331975),
 .UNSPECIFIED.);
#6568=B_SPLINE_CURVE_WITH_KNOTS('',3,(#49796,#49797,#49798,#49799,#49800,
#49801,#49802,#49803,#49804,#49805),.UNSPECIFIED.,.F.,.F.,(4,1,1,1,1,1,
1,4),(311.01767270539,311.509434791361,312.50908219324,313.508729595119,
314.508376996997,315.508024398876,316.507671800755,317.30085801257),
 .UNSPECIFIED.);
#6569=B_SPLINE_CURVE_WITH_KNOTS('',3,(#49806,#49807,#49808,#49809,#49810,
#49811,#49812,#49813,#49814,#49815,#49816),.UNSPECIFIED.,.F.,.F.,(4,1,1,
1,1,1,1,1,4),(311.01767270539,311.207895519101,312.207542920979,313.207190322858,
314.206837724737,315.206485126615,316.206132528494,317.205779930373,317.30085801257),
 .UNSPECIFIED.);
#6570=B_SPLINE_CURVE_WITH_KNOTS('',3,(#49821,#49822,#49823,#49824,#49825,
#49826,#49827,#49828,#49829,#49830),.UNSPECIFIED.,.F.,.F.,(4,1,1,1,1,1,
1,4),(304.73448739821,305.511550380089,306.511197781968,307.510845183847,
308.510492585725,309.510139987604,310.509787389483,311.01767270539),
 .UNSPECIFIED.);
#6571=B_SPLINE_CURVE_WITH_KNOTS('',3,(#49831,#49832,#49833,#49834,#49835,
#49836,#49837,#49838,#49839,#49840),.UNSPECIFIED.,.F.,.F.,(4,1,1,1,1,1,
1,4),(304.734487398211,305.210011107828,306.209658509707,307.209305911586,
308.208953313464,309.208600715343,310.208248117222,311.01767270539),
 .UNSPECIFIED.);
#6572=B_SPLINE_CURVE_WITH_KNOTS('',3,(#49845,#49846,#49847,#49848,#49849,
#49850,#49851,#49852,#49853,#49854,#49855),.UNSPECIFIED.,.F.,.F.,(4,1,1,
1,1,1,1,1,4),(298.451302091031,298.514018566938,299.513665968817,300.513313370696,
301.512960772574,302.512608174453,303.512255576332,304.511902978211,304.73448739821),
 .UNSPECIFIED.);
#6573=B_SPLINE_CURVE_WITH_KNOTS('',3,(#49856,#49857,#49858,#49859,#49860,
#49861,#49862,#49863,#49864,#49865),.UNSPECIFIED.,.F.,.F.,(4,1,1,1,1,1,
1,4),(298.451302091031,299.212126696556,300.211774098435,301.211421500314,
302.211068902192,303.210716304071,304.21036370595,304.734487398211),
 .UNSPECIFIED.);
#6574=B_SPLINE_CURVE_WITH_KNOTS('',3,(#49870,#49871,#49872,#49873,#49874,
#49875,#49876,#49877,#49878,#49879),.UNSPECIFIED.,.F.,.F.,(4,1,1,1,1,1,
1,4),(292.168116783851,292.516134155666,293.515781557545,294.515428959424,
295.515076361302,296.514723763181,297.51437116506,298.451302091031),
 .UNSPECIFIED.);
#6575=B_SPLINE_CURVE_WITH_KNOTS('',3,(#49880,#49881,#49882,#49883,#49884,
#49885,#49886,#49887,#49888,#49889,#49890),.UNSPECIFIED.,.F.,.F.,(4,1,1,
1,1,1,1,1,4),(292.168116783852,292.214594883406,293.214242285284,294.213889687163,
295.213537089042,296.21318449092,297.212831892799,298.212479294678,298.451302091031),
 .UNSPECIFIED.);
#6576=B_SPLINE_CURVE_WITH_KNOTS('',3,(#49895,#49896,#49897,#49898,#49899,
#49900,#49901,#49902,#49903,#49904),.UNSPECIFIED.,.F.,.F.,(4,1,1,1,1,1,
1,4),(285.884931476672,286.518249744394,287.517897146273,288.517544548152,
289.51719195003,290.516839351909,291.516486753788,292.168116783851),
 .UNSPECIFIED.);
#6577=B_SPLINE_CURVE_WITH_KNOTS('',3,(#49905,#49906,#49907,#49908,#49909,
#49910,#49911,#49912,#49913,#49914),.UNSPECIFIED.,.F.,.F.,(4,1,1,1,1,1,
1,4),(285.884931476672,286.216710472133,287.216357874012,288.216005275891,
289.215652677769,290.215300079648,291.214947481527,292.168116783852),
 .UNSPECIFIED.);
#6578=B_SPLINE_CURVE_WITH_KNOTS('',3,(#49919,#49920,#49921,#49922,#49923,
#49924,#49925,#49926,#49927,#49928),.UNSPECIFIED.,.F.,.F.,(4,1,1,1,1,1,
1,4),(279.601746169492,280.520365333122,281.520012735001,282.519660136879,
283.519307538758,284.518954940637,285.518602342516,285.884931476672),
 .UNSPECIFIED.);
#6579=B_SPLINE_CURVE_WITH_KNOTS('',3,(#49929,#49930,#49931,#49932,#49933,
#49934,#49935,#49936,#49937,#49938),.UNSPECIFIED.,.F.,.F.,(4,1,1,1,1,1,
1,4),(279.601746169493,280.218826060861,281.21847346274,282.218120864619,
283.217768266497,284.217415668376,285.217063070255,285.884931476672),
 .UNSPECIFIED.);
#6580=B_SPLINE_CURVE_WITH_KNOTS('',3,(#49943,#49944,#49945,#49946,#49947,
#49948,#49949,#49950,#49951,#49952,#49953),.UNSPECIFIED.,.F.,.F.,(4,1,1,
1,1,1,1,1,4),(273.318560862313,273.522833519971,274.52248092185,275.522128323729,
276.521775725607,277.521423127486,278.521070529365,279.520717931243,279.601746169492),
 .UNSPECIFIED.);
#6581=B_SPLINE_CURVE_WITH_KNOTS('',3,(#49954,#49955,#49956,#49957,#49958,
#49959,#49960,#49961,#49962,#49963),.UNSPECIFIED.,.F.,.F.,(4,1,1,1,1,1,
1,4),(273.318560862313,274.220941649589,275.220589051468,276.220236453347,
277.219883855225,278.219531257104,279.219178658983,279.601746169493),
 .UNSPECIFIED.);
#6582=B_SPLINE_CURVE_WITH_KNOTS('',3,(#49968,#49969,#49970,#49971,#49972,
#49973,#49974,#49975,#49976,#49977),.UNSPECIFIED.,.F.,.F.,(4,1,1,1,1,1,
1,4),(267.035375555133,267.524949108699,268.524596510578,269.524243912457,
270.523891314335,271.523538716214,272.523186118093,273.318560862313),
 .UNSPECIFIED.);
#6583=B_SPLINE_CURVE_WITH_KNOTS('',3,(#49978,#49979,#49980,#49981,#49982,
#49983,#49984,#49985,#49986,#49987,#49988),.UNSPECIFIED.,.F.,.F.,(4,1,1,
1,1,1,1,1,4),(267.035375555133,267.223409836438,268.223057238317,269.222704640196,
270.222352042074,271.221999443953,272.221646845832,273.221294247711,273.318560862313),
 .UNSPECIFIED.);
#6584=B_SPLINE_CURVE_WITH_KNOTS('',3,(#49993,#49994,#49995,#49996,#49997,
#49998,#49999,#50000,#50001,#50002),.UNSPECIFIED.,.F.,.F.,(4,1,1,1,1,1,
1,4),(260.752190247954,261.527064697427,262.526712099306,263.526359501184,
264.526006903063,265.525654304942,266.525301706821,267.035375555133),
 .UNSPECIFIED.);
#6585=B_SPLINE_CURVE_WITH_KNOTS('',3,(#50003,#50004,#50005,#50006,#50007,
#50008,#50009,#50010,#50011,#50012),.UNSPECIFIED.,.F.,.F.,(4,1,1,1,1,1,
1,4),(260.752190247954,261.225525425166,262.225172827045,263.224820228924,
264.224467630802,265.224115032681,266.22376243456,267.035375555133),
 .UNSPECIFIED.);
#6586=B_SPLINE_CURVE_WITH_KNOTS('',3,(#50017,#50018,#50019,#50020,#50021,
#50022,#50023,#50024,#50025,#50026,#50027),.UNSPECIFIED.,.F.,.F.,(4,1,1,
1,1,1,1,1,4),(254.469004940774,254.529532884276,255.529180286155,256.528827688034,
257.528475089912,258.528122491791,259.52776989367,260.527417295548,260.752190247954),
 .UNSPECIFIED.);
#6587=B_SPLINE_CURVE_WITH_KNOTS('',3,(#50028,#50029,#50030,#50031,#50032,
#50033,#50034,#50035,#50036,#50037),.UNSPECIFIED.,.F.,.F.,(4,1,1,1,1,1,
1,4),(254.469004940774,255.227641013894,256.227288415773,257.226935817652,
258.22658321953,259.226230621409,260.225878023288,260.752190247954),
 .UNSPECIFIED.);
#6588=B_SPLINE_CURVE_WITH_KNOTS('',3,(#50042,#50043,#50044,#50045,#50046,
#50047,#50048,#50049,#50050,#50051),.UNSPECIFIED.,.F.,.F.,(4,1,1,1,1,1,
1,4),(248.185819633594,248.531648473004,249.531295874883,250.530943276762,
251.53059067864,252.530238080519,253.529885482398,254.469004940774),
 .UNSPECIFIED.);
#6589=B_SPLINE_CURVE_WITH_KNOTS('',3,(#50052,#50053,#50054,#50055,#50056,
#50057,#50058,#50059,#50060,#50061,#50062),.UNSPECIFIED.,.F.,.F.,(4,1,1,
1,1,1,1,1,4),(248.185819633595,248.230109200743,249.229756602622,250.229404004501,
251.229051406379,252.228698808258,253.228346210137,254.227993612015,254.469004940774),
 .UNSPECIFIED.);
#6590=B_SPLINE_CURVE_WITH_KNOTS('',3,(#50067,#50068,#50069,#50070,#50071,
#50072,#50073,#50074,#50075,#50076),.UNSPECIFIED.,.F.,.F.,(4,1,1,1,1,1,
1,4),(241.902634326415,242.533764061732,243.533411463611,244.533058865489,
245.532706267368,246.532353669247,247.532001071126,248.185819633594),
 .UNSPECIFIED.);
#6591=B_SPLINE_CURVE_WITH_KNOTS('',3,(#50077,#50078,#50079,#50080,#50081,
#50082,#50083,#50084,#50085,#50086),.UNSPECIFIED.,.F.,.F.,(4,1,1,1,1,1,
1,4),(241.902634326415,242.232224789471,243.23187219135,244.231519593229,
245.231166995107,246.230814396986,247.230461798865,248.185819633595),
 .UNSPECIFIED.);
#6592=B_SPLINE_CURVE_WITH_KNOTS('',3,(#50091,#50092,#50093,#50094,#50095,
#50096,#50097,#50098,#50099,#50100),.UNSPECIFIED.,.F.,.F.,(4,1,1,1,1,1,
1,4),(235.619449019235,236.53587965046,237.535527052339,238.535174454217,
239.534821856096,240.534469257975,241.534116659853,241.902634326415),
 .UNSPECIFIED.);
#6593=B_SPLINE_CURVE_WITH_KNOTS('',3,(#50101,#50102,#50103,#50104,#50105,
#50106,#50107,#50108,#50109,#50110),.UNSPECIFIED.,.F.,.F.,(4,1,1,1,1,1,
1,4),(235.619449019236,236.234340378199,237.233987780078,238.233635181957,
239.233282583835,240.232929985714,241.232577387593,241.902634326415),
 .UNSPECIFIED.);
#6594=B_SPLINE_CURVE_WITH_KNOTS('',3,(#50115,#50116,#50117,#50118,#50119,
#50120,#50121,#50122,#50123,#50124,#50125),.UNSPECIFIED.,.F.,.F.,(4,1,1,
1,1,1,1,1,4),(229.336263712056,229.538347837309,230.537995239188,231.537642641067,
232.537290042945,233.536937444824,234.536584846703,235.536232248581,235.619449019235),
 .UNSPECIFIED.);
#6595=B_SPLINE_CURVE_WITH_KNOTS('',3,(#50126,#50127,#50128,#50129,#50130,
#50131,#50132,#50133,#50134,#50135),.UNSPECIFIED.,.F.,.F.,(4,1,1,1,1,1,
1,4),(229.336263712056,230.236455966927,231.236103368806,232.235750770684,
233.235398172563,234.235045574442,235.23469297632,235.619449019236),
 .UNSPECIFIED.);
#6596=B_SPLINE_CURVE_WITH_KNOTS('',3,(#50140,#50141,#50142,#50143,#50144,
#50145,#50146,#50147,#50148,#50149),.UNSPECIFIED.,.F.,.F.,(4,1,1,1,1,1,
1,4),(223.053078404876,223.540463426037,224.540110827916,225.539758229795,
226.539405631673,227.539053033552,228.538700435431,229.336263712056),
 .UNSPECIFIED.);
#6597=B_SPLINE_CURVE_WITH_KNOTS('',3,(#50150,#50151,#50152,#50153,#50154,
#50155,#50156,#50157,#50158,#50159,#50160),.UNSPECIFIED.,.F.,.F.,(4,1,1,
1,1,1,1,1,4),(223.053078404876,223.238924153776,224.238571555655,225.238218957534,
226.237866359412,227.237513761291,228.23716116317,229.236808565048,229.336263712056),
 .UNSPECIFIED.);
#6598=B_SPLINE_CURVE_WITH_KNOTS('',3,(#50165,#50166,#50167,#50168,#50169,
#50170,#50171,#50172,#50173,#50174),.UNSPECIFIED.,.F.,.F.,(4,1,1,1,1,1,
1,4),(216.769893097697,217.542579014765,218.542226416644,219.541873818522,
220.541521220401,221.54116862228,222.540816024158,223.053078404876),
 .UNSPECIFIED.);
#6599=B_SPLINE_CURVE_WITH_KNOTS('',3,(#50175,#50176,#50177,#50178,#50179,
#50180,#50181,#50182,#50183,#50184),.UNSPECIFIED.,.F.,.F.,(4,1,1,1,1,1,
1,4),(216.769893097697,217.241039742504,218.240687144383,219.240334546262,
220.23998194814,221.239629350019,222.239276751898,223.053078404876),
 .UNSPECIFIED.);
#6600=B_SPLINE_CURVE_WITH_KNOTS('',3,(#50189,#50190,#50191,#50192,#50193,
#50194,#50195,#50196,#50197,#50198,#50199),.UNSPECIFIED.,.F.,.F.,(4,1,1,
1,1,1,1,1,4),(210.486707790517,210.545047201614,211.544694603493,212.544342005372,
213.54398940725,214.543636809129,215.543284211008,216.542931612886,216.769893097697),
 .UNSPECIFIED.);
#6601=B_SPLINE_CURVE_WITH_KNOTS('',3,(#50200,#50201,#50202,#50203,#50204,
#50205,#50206,#50207,#50208,#50209),.UNSPECIFIED.,.F.,.F.,(4,1,1,1,1,1,
1,4),(210.486707790517,211.243155331232,212.242802733111,213.242450134989,
214.242097536868,215.241744938747,216.241392340625,216.769893097697),
 .UNSPECIFIED.);
#6602=B_SPLINE_CURVE_WITH_KNOTS('',3,(#50214,#50215,#50216,#50217,#50218,
#50219,#50220,#50221,#50222,#50223),.UNSPECIFIED.,.F.,.F.,(4,1,1,1,1,1,
1,4),(204.203522483337,204.547162790342,205.546810192221,206.5464575941,
207.546104995978,208.545752397857,209.545399799736,210.486707790517),
 .UNSPECIFIED.);
#6603=B_SPLINE_CURVE_WITH_KNOTS('',3,(#50224,#50225,#50226,#50227,#50228,
#50229,#50230,#50231,#50232,#50233,#50234),.UNSPECIFIED.,.F.,.F.,(4,1,1,
1,1,1,1,1,4),(204.203522483338,204.245623518081,205.24527091996,206.244918321839,
207.244565723717,208.244213125596,209.243860527475,210.243507929353,210.486707790517),
 .UNSPECIFIED.);
#6604=B_SPLINE_CURVE_WITH_KNOTS('',3,(#50239,#50240,#50241,#50242,#50243,
#50244,#50245,#50246,#50247,#50248),.UNSPECIFIED.,.F.,.F.,(4,1,1,1,1,1,
1,4),(197.920337176158,198.54927837907,199.548925780949,200.548573182827,
201.548220584706,202.547867986585,203.547515388463,204.203522483337),
 .UNSPECIFIED.);
#6605=B_SPLINE_CURVE_WITH_KNOTS('',3,(#50249,#50250,#50251,#50252,#50253,
#50254,#50255,#50256,#50257,#50258),.UNSPECIFIED.,.F.,.F.,(4,1,1,1,1,1,
1,4),(197.920337176158,198.247739106809,199.247386508688,200.247033910567,
201.246681312445,202.246328714324,203.245976116203,204.203522483338),
 .UNSPECIFIED.);
#6606=B_SPLINE_CURVE_WITH_KNOTS('',3,(#50263,#50264,#50265,#50266,#50267,
#50268,#50269,#50270,#50271,#50272),.UNSPECIFIED.,.F.,.F.,(4,1,1,1,1,1,
1,4),(191.637151868978,192.551393967798,193.551041369677,194.550688771555,
195.550336173434,196.549983575313,197.549630977191,197.920337176158),
 .UNSPECIFIED.);
#6607=B_SPLINE_CURVE_WITH_KNOTS('',3,(#50273,#50274,#50275,#50276,#50277,
#50278,#50279,#50280,#50281,#50282),.UNSPECIFIED.,.F.,.F.,(4,1,1,1,1,1,
1,4),(191.637151868979,192.249854695537,193.249502097416,194.249149499294,
195.248796901173,196.248444303052,197.24809170493,197.920337176158),
 .UNSPECIFIED.);
#6608=B_SPLINE_CURVE_WITH_KNOTS('',3,(#50287,#50288,#50289,#50290,#50291,
#50292,#50293,#50294,#50295,#50296,#50297),.UNSPECIFIED.,.F.,.F.,(4,1,1,
1,1,1,1,1,4),(185.353966561799,185.553862154647,186.553509556526,187.553156958405,
188.552804360283,189.552451762162,190.552099164041,191.551746565919,191.637151868978),
 .UNSPECIFIED.);
#6609=B_SPLINE_CURVE_WITH_KNOTS('',3,(#50298,#50299,#50300,#50301,#50302,
#50303,#50304,#50305,#50306,#50307),.UNSPECIFIED.,.F.,.F.,(4,1,1,1,1,1,
1,4),(185.353966561799,186.251970284265,187.251617686144,188.251265088022,
189.250912489901,190.25055989178,191.250207293658,191.637151868979),
 .UNSPECIFIED.);
#6610=B_SPLINE_CURVE_WITH_KNOTS('',3,(#50312,#50313,#50314,#50315,#50316,
#50317,#50318,#50319,#50320,#50321),.UNSPECIFIED.,.F.,.F.,(4,1,1,1,1,1,
1,4),(179.070781254619,179.555977743375,180.555625145254,181.555272547132,
182.554919949011,183.55456735089,184.554214752768,185.353966561799),
 .UNSPECIFIED.);
#6611=B_SPLINE_CURVE_WITH_KNOTS('',3,(#50322,#50323,#50324,#50325,#50326,
#50327,#50328,#50329,#50330,#50331,#50332),.UNSPECIFIED.,.F.,.F.,(4,1,1,
1,1,1,1,1,4),(179.07078125462,179.254438471114,180.254085872993,181.253733274872,
182.25338067675,183.253028078629,184.252675480508,185.252322882386,185.353966561799),
 .UNSPECIFIED.);
#6612=B_SPLINE_CURVE_WITH_KNOTS('',3,(#50337,#50338,#50339,#50340,#50341,
#50342,#50343,#50344,#50345,#50346),.UNSPECIFIED.,.F.,.F.,(4,1,1,1,1,1,
1,4),(172.78759594744,173.558093332103,174.557740733982,175.55738813586,
176.557035537739,177.556682939618,178.556330341496,179.070781254619),
 .UNSPECIFIED.);
#6613=B_SPLINE_CURVE_WITH_KNOTS('',3,(#50347,#50348,#50349,#50350,#50351,
#50352,#50353,#50354,#50355,#50356),.UNSPECIFIED.,.F.,.F.,(4,1,1,1,1,1,
1,4),(172.78759594744,173.256554059842,174.256201461721,175.255848863599,
176.255496265478,177.255143667357,178.254791069235,179.07078125462),
 .UNSPECIFIED.);
#6614=B_SPLINE_CURVE_WITH_KNOTS('',3,(#50361,#50362,#50363,#50364,#50365,
#50366,#50367,#50368,#50369,#50370,#50371),.UNSPECIFIED.,.F.,.F.,(4,1,1,
1,1,1,1,1,4),(166.50441064026,166.560561518952,167.560208920831,168.559856322709,
169.559503724588,170.559151126467,171.558798528346,172.558445930224,172.78759594744),
 .UNSPECIFIED.);
#6615=B_SPLINE_CURVE_WITH_KNOTS('',3,(#50372,#50373,#50374,#50375,#50376,
#50377,#50378,#50379,#50380,#50381),.UNSPECIFIED.,.F.,.F.,(4,1,1,1,1,1,
1,4),(166.50441064026,167.25866964857,168.258317050449,169.257964452327,
170.257611854206,171.257259256085,172.256906657963,172.78759594744),
 .UNSPECIFIED.);
#6616=B_SPLINE_CURVE_WITH_KNOTS('',3,(#50386,#50387,#50388,#50389,#50390,
#50391,#50392,#50393,#50394,#50395),.UNSPECIFIED.,.F.,.F.,(4,1,1,1,1,1,
1,4),(160.22122533308,160.56267710768,161.562324509559,162.561971911437,
163.561619313316,164.561266715195,165.560914117073,166.50441064026),
 .UNSPECIFIED.);
#6617=B_SPLINE_CURVE_WITH_KNOTS('',3,(#50396,#50397,#50398,#50399,#50400,
#50401,#50402,#50403,#50404,#50405,#50406),.UNSPECIFIED.,.F.,.F.,(4,1,1,
1,1,1,1,1,4),(160.221225333081,160.261137835419,161.260785237298,162.260432639177,
163.260080041055,164.259727442934,165.259374844813,166.259022246691,166.50441064026),
 .UNSPECIFIED.);
#6618=B_SPLINE_CURVE_WITH_KNOTS('',3,(#50411,#50412,#50413,#50414,#50415,
#50416,#50417,#50418,#50419,#50420),.UNSPECIFIED.,.F.,.F.,(4,1,1,1,1,1,
1,4),(153.938040025901,154.564792696408,155.564440098287,156.564087500165,
157.563734902044,158.563382303923,159.563029705801,160.22122533308),
 .UNSPECIFIED.);
#6619=B_SPLINE_CURVE_WITH_KNOTS('',3,(#50421,#50422,#50423,#50424,#50425,
#50426,#50427,#50428,#50429,#50430),.UNSPECIFIED.,.F.,.F.,(4,1,1,1,1,1,
1,4),(153.938040025901,154.263253424147,155.262900826026,156.262548227904,
157.262195629783,158.261843031662,159.26149043354,160.221225333081),
 .UNSPECIFIED.);
#6620=B_SPLINE_CURVE_WITH_KNOTS('',3,(#50435,#50436,#50437,#50438,#50439,
#50440,#50441,#50442,#50443,#50444),.UNSPECIFIED.,.F.,.F.,(4,1,1,1,1,1,
1,4),(147.654854718721,148.566908285136,149.566555687014,150.566203088893,
151.565850490772,152.565497892651,153.565145294529,153.938040025901),
 .UNSPECIFIED.);
#6621=B_SPLINE_CURVE_WITH_KNOTS('',3,(#50445,#50446,#50447,#50448,#50449,
#50450,#50451,#50452,#50453,#50454),.UNSPECIFIED.,.F.,.F.,(4,1,1,1,1,1,
1,4),(147.654854718722,148.265369012875,149.265016414754,150.264663816632,
151.264311218511,152.26395862039,153.263606022268,153.938040025901),
 .UNSPECIFIED.);
#6622=B_SPLINE_CURVE_WITH_KNOTS('',3,(#50459,#50460,#50461,#50462,#50463,
#50464,#50465,#50466,#50467,#50468,#50469),.UNSPECIFIED.,.F.,.F.,(4,1,1,
1,1,1,1,1,4),(141.371669411542,141.569376471985,142.569023873864,143.568671275742,
144.568318677621,145.5679660795,146.567613481378,147.567260883257,147.654854718721),
 .UNSPECIFIED.);
#6623=B_SPLINE_CURVE_WITH_KNOTS('',3,(#50470,#50471,#50472,#50473,#50474,
#50475,#50476,#50477,#50478,#50479),.UNSPECIFIED.,.F.,.F.,(4,1,1,1,1,1,
1,4),(141.371669411542,142.267484601603,143.267132003481,144.26677940536,
145.266426807239,146.266074209118,147.265721610996,147.654854718722),
 .UNSPECIFIED.);
#6624=B_SPLINE_CURVE_WITH_KNOTS('',3,(#50484,#50485,#50486,#50487,#50488,
#50489,#50490,#50491,#50492,#50493),.UNSPECIFIED.,.F.,.F.,(4,1,1,1,1,1,
1,4),(135.088484104362,135.571492060713,136.571139462592,137.57078686447,
138.570434266349,139.570081668228,140.569729070106,141.371669411542),
 .UNSPECIFIED.);
#6625=B_SPLINE_CURVE_WITH_KNOTS('',3,(#50494,#50495,#50496,#50497,#50498,
#50499,#50500,#50501,#50502,#50503,#50504),.UNSPECIFIED.,.F.,.F.,(4,1,1,
1,1,1,1,1,4),(135.088484104362,135.269952788452,136.269600190331,137.269247592209,
138.268894994088,139.268542395967,140.268189797845,141.267837199724,141.371669411542),
 .UNSPECIFIED.);
#6626=B_SPLINE_CURVE_WITH_KNOTS('',3,(#50509,#50510,#50511,#50512,#50513,
#50514,#50515,#50516,#50517,#50518),.UNSPECIFIED.,.F.,.F.,(4,1,1,1,1,1,
1,4),(128.805298797183,129.573607649441,130.57325505132,131.572902453198,
132.572549855077,133.572197256956,134.571844658834,135.088484104362),
 .UNSPECIFIED.);
#6627=B_SPLINE_CURVE_WITH_KNOTS('',3,(#50519,#50520,#50521,#50522,#50523,
#50524,#50525,#50526,#50527,#50528),.UNSPECIFIED.,.F.,.F.,(4,1,1,1,1,1,
1,4),(128.805298797183,129.27206837718,130.271715779059,131.271363180937,
132.271010582816,133.270657984695,134.270305386573,135.088484104362),
 .UNSPECIFIED.);
#6628=B_SPLINE_CURVE_WITH_KNOTS('',3,(#50533,#50534,#50535,#50536,#50537,
#50538,#50539,#50540,#50541,#50542,#50543),.UNSPECIFIED.,.F.,.F.,(4,1,1,
1,1,1,1,1,4),(122.522113490003,122.57607583629,123.575723238169,124.575370640047,
125.575018041926,126.574665443805,127.574312845683,128.573960247562,128.805298797183),
 .UNSPECIFIED.);
#6629=B_SPLINE_CURVE_WITH_KNOTS('',3,(#50544,#50545,#50546,#50547,#50548,
#50549,#50550,#50551,#50552,#50553),.UNSPECIFIED.,.F.,.F.,(4,1,1,1,1,1,
1,4),(122.522113490003,123.274183965908,124.273831367786,125.273478769665,
126.273126171544,127.272773573423,128.272420975301,128.805298797183),
 .UNSPECIFIED.);
#6630=B_SPLINE_CURVE_WITH_KNOTS('',3,(#50558,#50559,#50560,#50561,#50562,
#50563,#50564,#50565,#50566,#50567),.UNSPECIFIED.,.F.,.F.,(4,1,1,1,1,1,
1,4),(116.238928182823,116.578191425018,117.577838826897,118.577486228775,
119.577133630654,120.576781032533,121.576428434411,122.522113490003),
 .UNSPECIFIED.);
#6631=B_SPLINE_CURVE_WITH_KNOTS('',3,(#50568,#50569,#50570,#50571,#50572,
#50573,#50574,#50575,#50576,#50577,#50578),.UNSPECIFIED.,.F.,.F.,(4,1,1,
1,1,1,1,1,4),(116.238928182824,116.276652152757,117.276299554636,118.275946956514,
119.275594358393,120.275241760272,121.27488916215,122.274536564029,122.522113490003),
 .UNSPECIFIED.);
#6632=B_SPLINE_CURVE_WITH_KNOTS('',3,(#50583,#50584,#50585,#50586,#50587,
#50588,#50589,#50590,#50591,#50592),.UNSPECIFIED.,.F.,.F.,(4,1,1,1,1,1,
1,4),(109.955742875644,110.580307013746,111.579954415625,112.579601817503,
113.579249219382,114.578896621261,115.578544023139,116.238928182823),
 .UNSPECIFIED.);
#6633=B_SPLINE_CURVE_WITH_KNOTS('',3,(#50593,#50594,#50595,#50596,#50597,
#50598,#50599,#50600,#50601,#50602),.UNSPECIFIED.,.F.,.F.,(4,1,1,1,1,1,
1,4),(109.955742875644,110.278767741485,111.278415143364,112.278062545242,
113.277709947121,114.277357349,115.277004750878,116.238928182824),
 .UNSPECIFIED.);
#6634=B_SPLINE_CURVE_WITH_KNOTS('',3,(#50607,#50608,#50609,#50610,#50611,
#50612,#50613,#50614,#50615,#50616),.UNSPECIFIED.,.F.,.F.,(4,1,1,1,1,1,
1,4),(103.672557568464,104.582422602474,105.582070004352,106.581717406231,
107.58136480811,108.581012209988,109.580659611867,109.955742875644),
 .UNSPECIFIED.);
#6635=B_SPLINE_CURVE_WITH_KNOTS('',3,(#50617,#50618,#50619,#50620,#50621,
#50622,#50623,#50624,#50625,#50626),.UNSPECIFIED.,.F.,.F.,(4,1,1,1,1,1,
1,4),(103.672557568465,104.280883330213,105.280530732091,106.28017813397,
107.279825535849,108.279472937728,109.279120339606,109.955742875644),
 .UNSPECIFIED.);
#6636=B_SPLINE_CURVE_WITH_KNOTS('',3,(#50631,#50632,#50633,#50634,#50635,
#50636,#50637,#50638,#50639,#50640,#50641),.UNSPECIFIED.,.F.,.F.,(4,1,1,
1,1,1,1,1,4),(97.3893722612846,97.5848907893229,98.5845381912016,99.5841855930803,
100.583832994959,101.583480396838,102.583127798716,103.582775200595,103.672557568464),
 .UNSPECIFIED.);
#6637=B_SPLINE_CURVE_WITH_KNOTS('',3,(#50642,#50643,#50644,#50645,#50646,
#50647,#50648,#50649,#50650,#50651),.UNSPECIFIED.,.F.,.F.,(4,1,1,1,1,1,
1,4),(97.389372261285,98.2829989189407,99.2826463208194,100.282293722698,
101.281941124577,102.281588526455,103.281235928334,103.672557568465),
 .UNSPECIFIED.);
#6638=B_SPLINE_CURVE_WITH_KNOTS('',3,(#50656,#50657,#50658,#50659,#50660,
#50661,#50662,#50663,#50664,#50665),.UNSPECIFIED.,.F.,.F.,(4,1,1,1,1,1,
1,4),(91.1061869541051,91.5870063780508,92.5866537799295,93.5863011818082,
94.5859485836869,95.5855959855656,96.5852433874443,97.3893722612846),
 .UNSPECIFIED.);
#6639=B_SPLINE_CURVE_WITH_KNOTS('',3,(#50666,#50667,#50668,#50669,#50670,
#50671,#50672,#50673,#50674,#50675,#50676),.UNSPECIFIED.,.F.,.F.,(4,1,1,
1,1,1,1,1,4),(91.1061869541054,91.2854671057899,92.2851145076686,93.2847619095473,
94.2844093114259,95.2840567133046,96.2837041151833,97.283351517062,97.389372261285),
 .UNSPECIFIED.);
#6640=B_SPLINE_CURVE_WITH_KNOTS('',3,(#50681,#50682,#50683,#50684,#50685,
#50686,#50687,#50688,#50689,#50690),.UNSPECIFIED.,.F.,.F.,(4,1,1,1,1,1,
1,4),(84.8230016469255,85.5891219667787,86.5887693686574,87.5884167705361,
88.5880641724148,89.5877115742935,90.5873589761722,91.1061869541051),
 .UNSPECIFIED.);
#6641=B_SPLINE_CURVE_WITH_KNOTS('',3,(#50691,#50692,#50693,#50694,#50695,
#50696,#50697,#50698,#50699,#50700),.UNSPECIFIED.,.F.,.F.,(4,1,1,1,1,1,
1,4),(84.8230016469258,85.2875826945178,86.2872300963965,87.2868774982752,
88.2865249001539,89.2861723020325,90.2858197039112,91.1061869541054),
 .UNSPECIFIED.);
#6642=B_SPLINE_CURVE_WITH_KNOTS('',3,(#50705,#50706,#50707,#50708,#50709,
#50710,#50711,#50712,#50713,#50714,#50715),.UNSPECIFIED.,.F.,.F.,(4,1,1,
1,1,1,1,1,4),(78.5398163397459,78.5915901536279,79.5912375555066,80.5908849573853,
81.590532359264,82.5901797611427,83.5898271630214,84.5894745649001,84.8230016469255),
 .UNSPECIFIED.);
#6643=B_SPLINE_CURVE_WITH_KNOTS('',3,(#50716,#50717,#50718,#50719,#50720,
#50721,#50722,#50723,#50724,#50725),.UNSPECIFIED.,.F.,.F.,(4,1,1,1,1,1,
1,4),(78.5398163397463,79.2896982832457,80.2893456851244,81.2889930870031,
82.2886404888818,83.2882878907604,84.2879352926391,84.8230016469258),
 .UNSPECIFIED.);
#6644=B_SPLINE_CURVE_WITH_KNOTS('',3,(#50730,#50731,#50732,#50733,#50734,
#50735,#50736,#50737,#50738,#50739),.UNSPECIFIED.,.F.,.F.,(4,1,1,1,1,1,
1,4),(72.2566310325663,72.5937057423558,73.5933531442345,74.5930005461132,
75.5926479479919,76.5922953498706,77.5919427517493,78.5398163397459),
 .UNSPECIFIED.);
#6645=B_SPLINE_CURVE_WITH_KNOTS('',3,(#50740,#50741,#50742,#50743,#50744,
#50745,#50746,#50747,#50748,#50749,#50750),.UNSPECIFIED.,.F.,.F.,(4,1,1,
1,1,1,1,1,4),(72.2566310325667,72.2921664700949,73.2918138719736,74.2914612738523,
75.291108675731,76.2907560776096,77.2904034794883,78.290050881367,78.5398163397463),
 .UNSPECIFIED.);
#6646=B_SPLINE_CURVE_WITH_KNOTS('',3,(#50755,#50756,#50757,#50758,#50759,
#50760,#50761,#50762,#50763,#50764),.UNSPECIFIED.,.F.,.F.,(4,1,1,1,1,1,
1,4),(65.9734457253867,66.5958213310837,67.5954687329624,68.5951161348411,
69.5947635367198,70.5944109385985,71.5940583404772,72.2566310325663),
 .UNSPECIFIED.);
#6647=B_SPLINE_CURVE_WITH_KNOTS('',3,(#50765,#50766,#50767,#50768,#50769,
#50770,#50771,#50772,#50773,#50774),.UNSPECIFIED.,.F.,.F.,(4,1,1,1,1,1,
1,4),(65.9734457253871,66.2942820588228,67.2939294607015,68.2935768625802,
69.2932242644588,70.2928716663375,71.2925190682162,72.2566310325667),
 .UNSPECIFIED.);
#6648=B_SPLINE_CURVE_WITH_KNOTS('',3,(#50779,#50780,#50781,#50782,#50783,
#50784,#50785,#50786,#50787,#50788),.UNSPECIFIED.,.F.,.F.,(4,1,1,1,1,1,
1,4),(59.6902604182071,60.5979369198116,61.5975843216903,62.597231723569,
63.5968791254477,64.5965265273264,65.5961739292051,65.9734457253867),
 .UNSPECIFIED.);
#6649=B_SPLINE_CURVE_WITH_KNOTS('',3,(#50789,#50790,#50791,#50792,#50793,
#50794,#50795,#50796,#50797,#50798),.UNSPECIFIED.,.F.,.F.,(4,1,1,1,1,1,
1,4),(59.6902604182075,60.2963976475507,61.2960450494294,62.295692451308,
63.2953398531867,64.2949872550654,65.2946346569441,65.9734457253871),
 .UNSPECIFIED.);
#6650=B_SPLINE_CURVE_WITH_KNOTS('',3,(#50803,#50804,#50805,#50806,#50807,
#50808,#50809,#50810,#50811,#50812,#50813),.UNSPECIFIED.,.F.,.F.,(4,1,1,
1,1,1,1,1,4),(53.4070751110275,53.6004051066608,54.6000525085395,55.5996999104182,
56.5993473122969,57.5989947141756,58.5986421160543,59.5982895179329,59.6902604182071),
 .UNSPECIFIED.);
#6651=B_SPLINE_CURVE_WITH_KNOTS('',3,(#50814,#50815,#50816,#50817,#50818,
#50819,#50820,#50821,#50822,#50823),.UNSPECIFIED.,.F.,.F.,(4,1,1,1,1,1,
1,4),(53.4070751110279,54.2985132362786,55.2981606381573,56.2978080400359,
57.2974554419146,58.2971028437933,59.296750245672,59.6902604182075),
 .UNSPECIFIED.);
#6652=B_SPLINE_CURVE_WITH_KNOTS('',3,(#50828,#50829,#50830,#50831,#50832,
#50833,#50834,#50835,#50836,#50837),.UNSPECIFIED.,.F.,.F.,(4,1,1,1,1,1,
1,4),(47.123889803848,47.6025206953887,48.6021680972674,49.6018154991461,
50.6014629010248,51.6011103029035,52.6007577047822,53.4070751110275),
 .UNSPECIFIED.);
#6653=B_SPLINE_CURVE_WITH_KNOTS('',3,(#50838,#50839,#50840,#50841,#50842,
#50843,#50844,#50845,#50846,#50847,#50848),.UNSPECIFIED.,.F.,.F.,(4,1,1,
1,1,1,1,1,4),(47.1238898038483,47.3009814231278,48.3006288250065,49.3002762268852,
50.2999236287638,51.2995710306425,52.2992184325212,53.2988658343999,53.4070751110279),
 .UNSPECIFIED.);
#6654=B_SPLINE_CURVE_WITH_KNOTS('',3,(#50853,#50854,#50855,#50856,#50857,
#50858,#50859,#50860,#50861,#50862),.UNSPECIFIED.,.F.,.F.,(4,1,1,1,1,1,
1,4),(40.8407044966684,41.6046362841166,42.6042836859953,43.603931087874,
44.6035784897527,45.6032258916314,46.6028732935101,47.123889803848),
 .UNSPECIFIED.);
#6655=B_SPLINE_CURVE_WITH_KNOTS('',3,(#50863,#50864,#50865,#50866,#50867,
#50868,#50869,#50870,#50871,#50872),.UNSPECIFIED.,.F.,.F.,(4,1,1,1,1,1,
1,4),(40.8407044966687,41.3030970118557,42.3027444137344,43.302391815613,
44.3020392174917,45.3016866193704,46.3013340212491,47.1238898038483),
 .UNSPECIFIED.);
#6656=B_SPLINE_CURVE_WITH_KNOTS('',3,(#50877,#50878,#50879,#50880,#50881,
#50882,#50883,#50884,#50885,#50886,#50887),.UNSPECIFIED.,.F.,.F.,(4,1,1,
1,1,1,1,1,4),(34.5575191894888,34.6071044709659,35.6067518728445,36.6063992747232,
37.6060466766019,38.6056940784806,39.6053414803593,40.604988882238,40.8407044966684),
 .UNSPECIFIED.);
#6657=B_SPLINE_CURVE_WITH_KNOTS('',3,(#50888,#50889,#50890,#50891,#50892,
#50893,#50894,#50895,#50896,#50897),.UNSPECIFIED.,.F.,.F.,(4,1,1,1,1,1,
1,4),(34.5575191894891,35.3052126005836,36.3048600024622,37.3045074043409,
38.3041548062196,39.3038022080983,40.303449609977,40.8407044966687),
 .UNSPECIFIED.);
#6658=B_SPLINE_CURVE_WITH_KNOTS('',3,(#50902,#50903,#50904,#50905,#50906,
#50907,#50908,#50909,#50910,#50911),.UNSPECIFIED.,.F.,.F.,(4,1,1,1,1,1,
1,4),(28.2743338823092,28.6092200596937,29.6088674615724,30.6085148634511,
31.6081622653298,32.6078096672085,33.6074570690872,34.5575191894888),
 .UNSPECIFIED.);
#6659=B_SPLINE_CURVE_WITH_KNOTS('',3,(#50912,#50913,#50914,#50915,#50916,
#50917,#50918,#50919,#50920,#50921,#50922),.UNSPECIFIED.,.F.,.F.,(4,1,1,
1,1,1,1,1,4),(28.2743338823096,28.3076807874328,29.3073281893115,30.3069755911901,
31.3066229930688,32.3062703949475,33.3059177968262,34.3055651987049,34.5575191894891),
 .UNSPECIFIED.);
#6660=B_SPLINE_CURVE_WITH_KNOTS('',3,(#50927,#50928,#50929,#50930,#50931,
#50932,#50933,#50934,#50935,#50936),.UNSPECIFIED.,.F.,.F.,(4,1,1,1,1,1,
1,4),(21.9911485751296,22.6113356484216,23.6109830503003,24.610630452179,
25.6102778540577,26.6099252559364,27.6095726578151,28.2743338823092),
 .UNSPECIFIED.);
#6661=B_SPLINE_CURVE_WITH_KNOTS('',3,(#50937,#50938,#50939,#50940,#50941,
#50942,#50943,#50944,#50945,#50946),.UNSPECIFIED.,.F.,.F.,(4,1,1,1,1,1,
1,4),(21.99114857513,22.3097963761607,23.3094437780394,24.309091179918,
25.3087385817967,26.3083859836754,27.3080333855541,28.2743338823096),
 .UNSPECIFIED.);
#6662=B_SPLINE_CURVE_WITH_KNOTS('',3,(#50951,#50952,#50953,#50954,#50955,
#50956,#50957,#50958,#50959,#50960),.UNSPECIFIED.,.F.,.F.,(4,1,1,1,1,1,
1,4),(15.70796326795,16.6134512371495,17.6130986390282,18.6127460409069,
19.6123934427856,20.6120408446643,21.611688246543,21.9911485751296),
 .UNSPECIFIED.);
#6663=B_SPLINE_CURVE_WITH_KNOTS('',3,(#50961,#50962,#50963,#50964,#50965,
#50966,#50967,#50968,#50969,#50970),.UNSPECIFIED.,.F.,.F.,(4,1,1,1,1,1,
1,4),(15.7079632679504,16.3119119648886,17.3115593667672,18.3112067686459,
19.3108541705246,20.3105015724033,21.310148974282,21.99114857513),
 .UNSPECIFIED.);
#6664=B_SPLINE_CURVE_WITH_KNOTS('',3,(#53196,#53197,#53198,#53199,#53200,
#53201,#53202,#53203,#53204,#53205,#53206,#53207,#53208,#53209,#53210,#53211,
#53212,#53213,#53214,#53215,#53216,#53217,#53218,#53219,#53220,#53221,#53222,
#53223,#53224,#53225,#53226,#53227,#53228,#53229,#53230,#53231,#53232,#53233,
#53234,#53235,#53236,#53237,#53238,#53239,#53240,#53241,#53242,#53243,#53244,
#53245,#53246,#53247,#53248,#53249,#53250,#53251,#53252,#53253,#53254,#53255,
#53256,#53257,#53258,#53259,#53260,#53261,#53262,#53263,#53264,#53265,#53266,
#53267,#53268,#53269,#53270,#53271,#53272,#53273,#53274,#53275,#53276,#53277,
#53278,#53279,#53280,#53281,#53282,#53283,#53284,#53285,#53286,#53287,#53288,
#53289,#53290,#53291,#53292),.UNSPECIFIED.,.F.,.F.,(4,3,3,3,3,3,3,3,3,3,
3,3,3,3,3,3,3,3,3,3,3,3,3,3,3,3,3,3,3,3,3,3,4),(-0.741270768406061,-0.71696452138596,
-0.680440927304282,-0.659057791363252,-0.642652406304131,-0.636144085542677,
-0.599356622373509,-0.567167592100486,-0.553072383076001,-0.544362289353481,
-0.537677944349364,-0.502276237676446,-0.467138641981718,-0.433041019009119,
-0.410241859304171,-0.399246154564429,-0.394829851421709,-0.361211327226496,
-0.341844380189328,-0.307582718262882,-0.273165311582215,-0.262890280829855,
-0.257095817481949,-0.2236637832585,-0.190201737698465,-0.157152119987324,
-0.137508104988908,-0.127905898067162,-0.123173244372197,-0.0909734111245149,
-0.0592276901225634,-0.0284580599725401,0.),.UNSPECIFIED.);
#6665=B_SPLINE_CURVE_WITH_KNOTS('',3,(#53293,#53294,#53295,#53296,#53297,
#53298,#53299,#53300,#53301,#53302,#53303,#53304,#53305),.UNSPECIFIED.,
 .F.,.F.,(4,3,3,3,4),(547.747166935536,547.806776229519,548.806423631398,
549.806071033277,550.743811641397),.UNSPECIFIED.);
#6666=B_SPLINE_CURVE_WITH_KNOTS('',3,(#53307,#53308,#53309,#53310,#53311,
#53312,#53313,#53314,#53315,#53316,#53317,#53318,#53319,#53320,#53321,#53322,
#53323,#53324,#53325,#53326,#53327,#53328,#53329,#53330,#53331,#53332,#53333,
#53334,#53335,#53336,#53337,#53338,#53339,#53340,#53341,#53342,#53343,#53344,
#53345,#53346,#53347,#53348,#53349,#53350,#53351,#53352,#53353,#53354,#53355,
#53356,#53357,#53358,#53359,#53360,#53361,#53362,#53363,#53364,#53365,#53366,
#53367,#53368,#53369,#53370,#53371,#53372,#53373,#53374,#53375,#53376,#53377,
#53378,#53379,#53380,#53381,#53382,#53383,#53384,#53385,#53386,#53387,#53388,
#53389,#53390,#53391,#53392,#53393,#53394,#53395,#53396,#53397,#53398,#53399,
#53400,#53401,#53402,#53403),.UNSPECIFIED.,.F.,.F.,(4,3,3,3,3,3,3,3,3,3,
3,3,3,3,3,3,3,3,3,3,3,3,3,3,3,3,3,3,3,3,3,3,4),(-0.744397949170487,-0.724177512305599,
-0.693104810887909,-0.673480410559028,-0.660865919846913,-0.655179200686015,
-0.623187078074113,-0.592677994018076,-0.579330269743559,-0.573127817992138,
-0.567887494883166,-0.534520276836344,-0.500626959353002,-0.466813781988586,
-0.444888937897893,-0.437603624926938,-0.432876525336586,-0.397960991396844,
-0.379114405625813,-0.345405658901566,-0.311054469280115,-0.300315140774403,
-0.295343553676723,-0.261000993005831,-0.225526526851419,-0.189691877406385,
-0.165980392730587,-0.15447337421228,-0.147027486947459,-0.110270615210594,
-0.0734630229077671,-0.0367315114538836,0.),.UNSPECIFIED.);
#6667=B_SPLINE_CURVE_WITH_KNOTS('',3,(#53404,#53405,#53406,#53407,#53408,
#53409,#53410,#53411,#53412),.UNSPECIFIED.,.F.,.F.,(4,1,1,1,1,1,4),(10.3759343473751,
11.3136749554951,12.3133223573738,13.3129697592525,14.3126171611312,15.3122645630099,
15.7079632679504),.UNSPECIFIED.);
#6668=B_SPLINE_CURVE_WITH_KNOTS('',3,(#53418,#53419,#53420,#53421,#53422,
#53423,#53424,#53425,#53426,#53427,#53428,#53429,#53430,#53431,#53432,#53433,
#53434,#53435,#53436,#53437,#53438,#53439,#53440,#53441,#53442,#53443,#53444,
#53445,#53446,#53447,#53448,#53449,#53450,#53451,#53452,#53453,#53454,#53455,
#53456,#53457,#53458,#53459,#53460,#53461,#53462,#53463,#53464,#53465,#53466,
#53467,#53468,#53469,#53470,#53471,#53472,#53473,#53474,#53475,#53476,#53477,
#53478,#53479,#53480,#53481,#53482,#53483,#53484,#53485,#53486,#53487,#53488,
#53489,#53490,#53491,#53492,#53493,#53494,#53495,#53496,#53497,#53498,#53499,
#53500,#53501,#53502,#53503,#53504,#53505,#53506,#53507,#53508,#53509,#53510,
#53511,#53512,#53513,#53514),.UNSPECIFIED.,.F.,.F.,(4,3,3,3,3,3,3,3,3,3,
3,3,3,3,3,3,3,3,3,3,3,3,3,3,3,3,3,3,3,3,3,3,4),(-0.741270768406467,-0.716964521386347,
-0.680440927292735,-0.659057791393028,-0.642652406228543,-0.636144086243808,
-0.599356622987026,-0.567167592637341,-0.553072383177883,-0.544362289404779,
-0.537677944378733,-0.50227623772544,-0.467138642075895,-0.433041019100885,
-0.410241859373051,-0.399246154678599,-0.394829851420893,-0.361211327215821,
-0.341844380189548,-0.307582718280384,-0.273165311644367,-0.262890280934216,
-0.25709581734905,-0.223663783123785,-0.190201737572306,-0.157152119931196,
-0.137508104939796,-0.127905897837719,-0.123173244323147,-0.0909734110776745,
-0.0592276900781323,-0.0284580599372398,0.),.UNSPECIFIED.);
#6669=B_SPLINE_CURVE_WITH_KNOTS('',3,(#53517,#53518,#53519,#53520,#53521,
#53522,#53523,#53524),.UNSPECIFIED.,.F.,.F.,(4,1,1,1,1,4),(11.6152142277561,
12.6148616296348,13.6145090315135,14.6141564333922,15.6138038352709,15.70796326795),
 .UNSPECIFIED.);
#6670=B_SPLINE_CURVE_WITH_KNOTS('',3,(#55750,#55751,#55752,#55753,#55754,
#55755,#55756,#55757,#55758,#55759,#55760,#55761,#55762,#55763,#55764,#55765,
#55766,#55767,#55768,#55769,#55770,#55771,#55772,#55773,#55774,#55775,#55776,
#55777,#55778,#55779,#55780,#55781,#55782,#55783,#55784,#55785,#55786,#55787,
#55788,#55789,#55790,#55791,#55792,#55793,#55794,#55795,#55796,#55797,#55798,
#55799,#55800,#55801,#55802,#55803,#55804,#55805,#55806,#55807,#55808,#55809,
#55810,#55811,#55812,#55813,#55814,#55815,#55816,#55817,#55818,#55819,#55820,
#55821,#55822,#55823,#55824,#55825,#55826,#55827,#55828,#55829,#55830,#55831,
#55832,#55833,#55834,#55835,#55836,#55837,#55838,#55839,#55840,#55841,#55842,
#55843,#55844,#55845,#55846),.UNSPECIFIED.,.F.,.F.,(4,3,3,3,3,3,3,3,3,3,
3,3,3,3,3,3,3,3,3,3,3,3,3,3,3,3,3,3,3,3,3,3,4),(-0.744397949170763,-0.724177512305978,
-0.693104810875057,-0.673480410546995,-0.660865919810601,-0.655179200975098,
-0.623187078406178,-0.592677994308664,-0.579330270016002,-0.573127818760234,
-0.567887496175861,-0.534520278122044,-0.500626960665077,-0.466813783274203,
-0.444888938862169,-0.437603634425512,-0.432876535092151,-0.397961001197226,
-0.379114405626065,-0.345405658896003,-0.31105446923983,-0.300315140715421,
-0.29534355375871,-0.261000992978768,-0.225526526817216,-0.189691877366772,
-0.165980392695925,-0.154473374164193,-0.147027486633724,-0.110270614975293,
-0.0734630226814967,-0.0367315113407483,0.),.UNSPECIFIED.);
#6671=B_SPLINE_CURVE_WITH_KNOTS('',3,(#55847,#55848,#55849,#55850,#55851,
#55852,#55853,#55854,#55855,#55856),.UNSPECIFIED.,.F.,.F.,(4,3,3,4),(-552.805013238912,
-551.805365837034,-550.805718435155,-550.729870764817),.UNSPECIFIED.);
#6672=B_SPLINE_CURVE_WITH_KNOTS('',3,(#55929,#55930,#55931,#55932,#55933,
#55934,#55935,#55936,#55937,#55938,#55939,#55940,#55941,#55942,#55943,#55944,
#55945,#55946,#55947),.UNSPECIFIED.,.F.,.F.,(4,3,3,3,3,3,4),(-0.136738994562975,
-0.122118862870872,-0.0885145718176996,-0.0747535058851621,-0.0395493225812212,
-0.00612228981501024,0.),.UNSPECIFIED.);
#6673=B_SPLINE_CURVE_WITH_KNOTS('',3,(#55951,#55952,#55953,#55954,#55955,
#55956,#55957,#55958,#55959,#55960,#55961,#55962,#55963,#55964,#55965,#55966,
#55967,#55968,#55969,#55970,#55971,#55972,#55973,#55974,#55975,#55976,#55977,
#55978,#55979,#55980,#55981),.UNSPECIFIED.,.F.,.F.,(4,3,3,3,3,3,3,3,3,3,
4),(-0.273459791663231,-0.23953153084867,-0.216807499006331,-0.179324588754136,
-0.164307407772797,-0.122118862870832,-0.0885145718176626,-0.0747535058851424,
-0.0395513512837351,-0.00612692919564764,0.),.UNSPECIFIED.);
#6674=B_SPLINE_CURVE_WITH_KNOTS('',3,(#55985,#55986,#55987,#55988,#55989,
#55990,#55991,#55992,#55993,#55994,#55995,#55996,#55997,#55998,#55999,#56000,
#56001,#56002,#56003,#56004,#56005,#56006,#56007,#56008,#56009,#56010,#56011,
#56012,#56013,#56014,#56015),.UNSPECIFIED.,.F.,.F.,(4,3,3,3,3,3,3,3,3,3,
4),(-0.273459791663253,-0.239669924355099,-0.21680749900636,-0.184963318451147,
-0.16430740777285,-0.122118862870878,-0.0827567027783513,-0.0747535058851617,
-0.0395111290131105,-0.00593748200146239,0.),.UNSPECIFIED.);
#6675=B_SPLINE_CURVE_WITH_KNOTS('',3,(#56019,#56020,#56021,#56022,#56023,
#56024,#56025,#56026,#56027,#56028,#56029,#56030,#56031,#56032,#56033,#56034,
#56035,#56036,#56037,#56038,#56039,#56040,#56041,#56042,#56043,#56044,#56045,
#56046,#56047,#56048,#56049),.UNSPECIFIED.,.F.,.F.,(4,3,3,3,3,3,3,3,3,3,
4),(-0.273459791663475,-0.239530723478153,-0.216807499006455,-0.179324881519317,
-0.164307407772862,-0.122118862870871,-0.0885145718177087,-0.0747535058851606,
-0.0395493225800805,-0.00612228981348414,0.),.UNSPECIFIED.);
#6676=B_SPLINE_CURVE_WITH_KNOTS('',3,(#56053,#56054,#56055,#56056,#56057,
#56058,#56059,#56060,#56061,#56062,#56063,#56064,#56065,#56066,#56067,#56068,
#56069,#56070,#56071,#56072,#56073,#56074,#56075,#56076,#56077,#56078,#56079,
#56080,#56081,#56082,#56083),.UNSPECIFIED.,.F.,.F.,(4,3,3,3,3,3,3,3,3,3,
4),(-0.273459791663443,-0.239531530848477,-0.216807499006449,-0.179324588753778,
-0.164307407772894,-0.122118862870893,-0.0885145718177228,-0.0747535058851679,
-0.0395513512850697,-0.00612692919683943,0.),.UNSPECIFIED.);
#6677=B_SPLINE_CURVE_WITH_KNOTS('',3,(#56087,#56088,#56089,#56090,#56091,
#56092,#56093,#56094,#56095,#56096,#56097,#56098,#56099,#56100,#56101,#56102,
#56103,#56104,#56105,#56106,#56107,#56108,#56109,#56110,#56111,#56112,#56113,
#56114,#56115,#56116,#56117),.UNSPECIFIED.,.F.,.F.,(4,3,3,3,3,3,3,3,3,3,
4),(-0.273459791663401,-0.239669924355128,-0.216807499006408,-0.184963318451192,
-0.164307407772861,-0.122118862870879,-0.0827567027776284,-0.0747535058851694,
-0.0395111290123009,-0.00593748200080557,0.),.UNSPECIFIED.);
#6678=B_SPLINE_CURVE_WITH_KNOTS('',3,(#56120,#56121,#56122,#56123,#56124,
#56125,#56126,#56127,#56128,#56129,#56130,#56131,#56132,#56133,#56134,#56135),
 .UNSPECIFIED.,.F.,.F.,(4,3,3,3,3,4),(-0.273459791663231,-0.239530723478429,
-0.216807499006338,-0.179324881517841,-0.16430740777284,-0.136738994562975),
 .UNSPECIFIED.);
#6679=B_SPLINE_CURVE_WITH_KNOTS('',3,(#56157,#56158,#56159,#56160),
 .UNSPECIFIED.,.F.,.F.,(4,4),(0.718335936055936,0.955209640017503),
 .UNSPECIFIED.);
#6680=B_SPLINE_CURVE_WITH_KNOTS('',3,(#56162,#56163,#56164,#56165,#56166,
#56167),.UNSPECIFIED.,.F.,.F.,(4,2,4),(-0.0458340621949542,-0.0229142437600697,
0.),.UNSPECIFIED.);
#6681=B_SPLINE_CURVE_WITH_KNOTS('',3,(#56169,#56170,#56171,#56172,#56173),
 .UNSPECIFIED.,.F.,.F.,(4,1,4),(-0.952706230317623,-0.504344050522728,-0.168698268101591),
 .UNSPECIFIED.);
#6682=B_SPLINE_CURVE_WITH_KNOTS('',3,(#56175,#56176,#56177,#56178,#56179,
#56180),.UNSPECIFIED.,.F.,.F.,(4,2,4),(-0.0458340597127026,-0.022919521896342,
0.),.UNSPECIFIED.);
#6683=B_SPLINE_CURVE_WITH_KNOTS('',3,(#56181,#56182,#56183,#56184),
 .UNSPECIFIED.,.F.,.F.,(4,4),(0.166194858401647,0.403068562363093),
 .UNSPECIFIED.);
#6684=B_SPLINE_CURVE_WITH_KNOTS('',3,(#56206,#56207,#56208,#56209),
 .UNSPECIFIED.,.F.,.F.,(4,4),(0.718335936055936,0.955209640017503),
 .UNSPECIFIED.);
#6685=B_SPLINE_CURVE_WITH_KNOTS('',3,(#56211,#56212,#56213,#56214,#56215,
#56216),.UNSPECIFIED.,.F.,.F.,(4,2,4),(-0.0458340621875639,-0.0229142437586445,
0.),.UNSPECIFIED.);
#6686=B_SPLINE_CURVE_WITH_KNOTS('',3,(#56218,#56219,#56220,#56221,#56222),
 .UNSPECIFIED.,.F.,.F.,(4,1,4),(-0.952706230317622,-0.504344050522728,-0.168698268101591),
 .UNSPECIFIED.);
#6687=B_SPLINE_CURVE_WITH_KNOTS('',3,(#56223,#56224,#56225,#56226,#56227,
#56228),.UNSPECIFIED.,.F.,.F.,(4,2,4),(-0.0458340597191651,-0.0229195218989816,
0.),.UNSPECIFIED.);
#6688=B_SPLINE_CURVE_WITH_KNOTS('',3,(#56229,#56230,#56231,#56232),
 .UNSPECIFIED.,.F.,.F.,(4,4),(0.166194858401647,0.403068562363093),
 .UNSPECIFIED.);
#6689=B_SPLINE_CURVE_WITH_KNOTS('',3,(#56235,#56236,#56237,#56238),
 .UNSPECIFIED.,.F.,.F.,(4,4),(0.166194858401646,0.403068562363093),
 .UNSPECIFIED.);
#6690=B_SPLINE_CURVE_WITH_KNOTS('',3,(#56241,#56242,#56243,#56244),
 .UNSPECIFIED.,.F.,.F.,(4,4),(0.166194858401646,0.403068562363093),
 .UNSPECIFIED.);
#6691=B_SPLINE_CURVE_WITH_KNOTS('',3,(#56245,#56246,#56247,#56248),
 .UNSPECIFIED.,.F.,.F.,(4,4),(0.718335936055935,0.955209640017502),
 .UNSPECIFIED.);
#6692=B_SPLINE_CURVE_WITH_KNOTS('',3,(#56251,#56252,#56253,#56254),
 .UNSPECIFIED.,.F.,.F.,(4,4),(0.166194858401647,0.403068562363092),
 .UNSPECIFIED.);
#6693=B_SPLINE_CURVE_WITH_KNOTS('',3,(#56255,#56256,#56257,#56258),
 .UNSPECIFIED.,.F.,.F.,(4,4),(0.718335936055935,0.955209640017502),
 .UNSPECIFIED.);
#6694=B_SPLINE_CURVE_WITH_KNOTS('',3,(#56261,#56262,#56263,#56264),
 .UNSPECIFIED.,.F.,.F.,(4,4),(0.166194858401647,0.403068562363094),
 .UNSPECIFIED.);
#6695=B_SPLINE_CURVE_WITH_KNOTS('',3,(#56265,#56266,#56267,#56268),
 .UNSPECIFIED.,.F.,.F.,(4,4),(0.718335936055935,0.955209640017502),
 .UNSPECIFIED.);
#6696=B_SPLINE_CURVE_WITH_KNOTS('',3,(#56270,#56271,#56272,#56273),
 .UNSPECIFIED.,.F.,.F.,(4,4),(0.718335936055935,0.955209640017502),
 .UNSPECIFIED.);
#6697=B_SPLINE_CURVE_WITH_KNOTS('',3,(#56295,#56296,#56297,#56298,#56299,
#56300),.UNSPECIFIED.,.F.,.F.,(4,2,4),(-0.0458340621934442,-0.0229142437595665,
0.),.UNSPECIFIED.);
#6698=B_SPLINE_CURVE_WITH_KNOTS('',3,(#56302,#56303,#56304,#56305,#56306),
 .UNSPECIFIED.,.F.,.F.,(4,1,4),(-0.952706230317622,-0.617060447896421,-0.168698268101591),
 .UNSPECIFIED.);
#6699=B_SPLINE_CURVE_WITH_KNOTS('',3,(#56307,#56308,#56309,#56310,#56311,
#56312),.UNSPECIFIED.,.F.,.F.,(4,2,4),(-0.0458340597159227,-0.022919521898133,
0.),.UNSPECIFIED.);
#6700=B_SPLINE_CURVE_WITH_KNOTS('',3,(#56320,#56321,#56322,#56323,#56324,
#56325),.UNSPECIFIED.,.F.,.F.,(4,2,4),(-0.045834059720736,-0.0229195218988986,
0.),.UNSPECIFIED.);
#6701=B_SPLINE_CURVE_WITH_KNOTS('',3,(#56331,#56332,#56333,#56334,#56335,
#56336),.UNSPECIFIED.,.F.,.F.,(4,2,4),(-0.0458340621946948,-0.0229142437601225,
0.),.UNSPECIFIED.);
#6702=B_SPLINE_CURVE_WITH_KNOTS('',3,(#56338,#56339,#56340,#56341,#56342,
#56343),.UNSPECIFIED.,.F.,.F.,(4,2,4),(-0.0458340597183968,-0.0229195218978244,
0.),.UNSPECIFIED.);
#6703=B_SPLINE_CURVE_WITH_KNOTS('',3,(#56348,#56349,#56350,#56351,#56352,
#56353),.UNSPECIFIED.,.F.,.F.,(4,2,4),(-0.0458340621954861,-0.0229142437603453,
0.),.UNSPECIFIED.);
#6704=B_SPLINE_CURVE_WITH_KNOTS('',3,(#56356,#56357,#56358,#56359,#56360,
#56361),.UNSPECIFIED.,.F.,.F.,(4,2,4),(-0.0458340621957891,-0.022914243760215,
0.),.UNSPECIFIED.);
#6705=B_SPLINE_CURVE_WITH_KNOTS('',3,(#56363,#56364,#56365,#56366,#56367,
#56368),.UNSPECIFIED.,.F.,.F.,(4,2,4),(-0.0458340597171303,-0.0229195218977166,
0.),.UNSPECIFIED.);
#6706=B_SPLINE_CURVE_WITH_KNOTS('',3,(#56390,#56391,#56392,#56393,#56394),
 .UNSPECIFIED.,.F.,.F.,(4,1,4),(-0.952706230317622,-0.617060447896421,-0.168698268101591),
 .UNSPECIFIED.);
#6707=B_SPLINE_CURVE_WITH_KNOTS('',3,(#56423,#56424,#56425,#56426,#56427),
 .UNSPECIFIED.,.F.,.F.,(4,1,4),(-0.952706230317622,-0.504344050522728,-0.168698268101591),
 .UNSPECIFIED.);
#6708=B_SPLINE_CURVE_WITH_KNOTS('',3,(#56464,#56465,#56466,#56467,#56468),
 .UNSPECIFIED.,.F.,.F.,(4,1,4),(-0.952706230317622,-0.504344050522728,-0.168698268101591),
 .UNSPECIFIED.);
#6709=VERTEX_POINT('',#22944);
#6710=VERTEX_POINT('',#22945);
#6711=VERTEX_POINT('',#22954);
#6712=VERTEX_POINT('',#22956);
#6713=VERTEX_POINT('',#22960);
#6714=VERTEX_POINT('',#22962);
#6715=VERTEX_POINT('',#22971);
#6716=VERTEX_POINT('',#22973);
#6717=VERTEX_POINT('',#22975);
#6718=VERTEX_POINT('',#22979);
#6719=VERTEX_POINT('',#22981);
#6720=VERTEX_POINT('',#22983);
#6721=VERTEX_POINT('',#22994);
#6722=VERTEX_POINT('',#23003);
#6723=VERTEX_POINT('',#23007);
#6724=VERTEX_POINT('',#23009);
#6725=VERTEX_POINT('',#23015);
#6726=VERTEX_POINT('',#23016);
#6727=VERTEX_POINT('',#23025);
#6728=VERTEX_POINT('',#23027);
#6729=VERTEX_POINT('',#23031);
#6730=VERTEX_POINT('',#23033);
#6731=VERTEX_POINT('',#23042);
#6732=VERTEX_POINT('',#23044);
#6733=VERTEX_POINT('',#23046);
#6734=VERTEX_POINT('',#23050);
#6735=VERTEX_POINT('',#23052);
#6736=VERTEX_POINT('',#23054);
#6737=VERTEX_POINT('',#23065);
#6738=VERTEX_POINT('',#23074);
#6739=VERTEX_POINT('',#23078);
#6740=VERTEX_POINT('',#23080);
#6741=VERTEX_POINT('',#23086);
#6742=VERTEX_POINT('',#23090);
#6743=VERTEX_POINT('',#23091);
#6744=VERTEX_POINT('',#23093);
#6745=VERTEX_POINT('',#23095);
#6746=VERTEX_POINT('',#23097);
#6747=VERTEX_POINT('',#23099);
#6748=VERTEX_POINT('',#23101);
#6749=VERTEX_POINT('',#23103);
#6750=VERTEX_POINT('',#23106);
#6751=VERTEX_POINT('',#23108);
#6752=VERTEX_POINT('',#23113);
#6753=VERTEX_POINT('',#23115);
#6754=VERTEX_POINT('',#23119);
#6755=VERTEX_POINT('',#23120);
#6756=VERTEX_POINT('',#23122);
#6757=VERTEX_POINT('',#23124);
#6758=VERTEX_POINT('',#23126);
#6759=VERTEX_POINT('',#23128);
#6760=VERTEX_POINT('',#23130);
#6761=VERTEX_POINT('',#23132);
#6762=VERTEX_POINT('',#23135);
#6763=VERTEX_POINT('',#23137);
#6764=VERTEX_POINT('',#23140);
#6765=VERTEX_POINT('',#23144);
#6766=VERTEX_POINT('',#23148);
#6767=VERTEX_POINT('',#23152);
#6768=VERTEX_POINT('',#23153);
#6769=VERTEX_POINT('',#23162);
#6770=VERTEX_POINT('',#23164);
#6771=VERTEX_POINT('',#23179);
#6772=VERTEX_POINT('',#23186);
#6773=VERTEX_POINT('',#23188);
#6774=VERTEX_POINT('',#23195);
#6775=VERTEX_POINT('',#23204);
#6776=VERTEX_POINT('',#23205);
#6777=VERTEX_POINT('',#23214);
#6778=VERTEX_POINT('',#23216);
#6779=VERTEX_POINT('',#23225);
#6780=VERTEX_POINT('',#23229);
#6781=VERTEX_POINT('',#23234);
#6782=VERTEX_POINT('',#23238);
#6783=VERTEX_POINT('',#23245);
#6784=VERTEX_POINT('',#23258);
#6785=VERTEX_POINT('',#23260);
#6786=VERTEX_POINT('',#23262);
#6787=VERTEX_POINT('',#23267);
#6788=VERTEX_POINT('',#23283);
#6789=VERTEX_POINT('',#23299);
#6790=VERTEX_POINT('',#23314);
#6791=VERTEX_POINT('',#23332);
#6792=VERTEX_POINT('',#23333);
#6793=VERTEX_POINT('',#23335);
#6794=VERTEX_POINT('',#23337);
#6795=VERTEX_POINT('',#23340);
#6796=VERTEX_POINT('',#23341);
#6797=VERTEX_POINT('',#23343);
#6798=VERTEX_POINT('',#23345);
#6799=VERTEX_POINT('',#23348);
#6800=VERTEX_POINT('',#23349);
#6801=VERTEX_POINT('',#23351);
#6802=VERTEX_POINT('',#23353);
#6803=VERTEX_POINT('',#23356);
#6804=VERTEX_POINT('',#23357);
#6805=VERTEX_POINT('',#23359);
#6806=VERTEX_POINT('',#23361);
#6807=VERTEX_POINT('',#23364);
#6808=VERTEX_POINT('',#23365);
#6809=VERTEX_POINT('',#23367);
#6810=VERTEX_POINT('',#23369);
#6811=VERTEX_POINT('',#23372);
#6812=VERTEX_POINT('',#23373);
#6813=VERTEX_POINT('',#23375);
#6814=VERTEX_POINT('',#23377);
#6815=VERTEX_POINT('',#23381);
#6816=VERTEX_POINT('',#23382);
#6817=VERTEX_POINT('',#23393);
#6818=VERTEX_POINT('',#23395);
#6819=VERTEX_POINT('',#23400);
#6820=VERTEX_POINT('',#23413);
#6821=VERTEX_POINT('',#23422);
#6822=VERTEX_POINT('',#23425);
#6823=VERTEX_POINT('',#23427);
#6824=VERTEX_POINT('',#23433);
#6825=VERTEX_POINT('',#23435);
#6826=VERTEX_POINT('',#23437);
#6827=VERTEX_POINT('',#23440);
#6828=VERTEX_POINT('',#23449);
#6829=VERTEX_POINT('',#23451);
#6830=VERTEX_POINT('',#23460);
#6831=VERTEX_POINT('',#23465);
#6832=VERTEX_POINT('',#23472);
#6833=VERTEX_POINT('',#23474);
#6834=VERTEX_POINT('',#23481);
#6835=VERTEX_POINT('',#23486);
#6836=VERTEX_POINT('',#23488);
#6837=VERTEX_POINT('',#23495);
#6838=VERTEX_POINT('',#23503);
#6839=VERTEX_POINT('',#23507);
#6840=VERTEX_POINT('',#23508);
#6841=VERTEX_POINT('',#23513);
#6842=VERTEX_POINT('',#23515);
#6843=VERTEX_POINT('',#23526);
#6844=VERTEX_POINT('',#23537);
#6845=VERTEX_POINT('',#23542);
#6846=VERTEX_POINT('',#23545);
#6847=VERTEX_POINT('',#23547);
#6848=VERTEX_POINT('',#23557);
#6849=VERTEX_POINT('',#23559);
#6850=VERTEX_POINT('',#23561);
#6851=VERTEX_POINT('',#23581);
#6852=VERTEX_POINT('',#23585);
#6853=VERTEX_POINT('',#23587);
#6854=VERTEX_POINT('',#23589);
#6855=VERTEX_POINT('',#23591);
#6856=VERTEX_POINT('',#23593);
#6857=VERTEX_POINT('',#23595);
#6858=VERTEX_POINT('',#23597);
#6859=VERTEX_POINT('',#23600);
#6860=VERTEX_POINT('',#23602);
#6861=VERTEX_POINT('',#23606);
#6862=VERTEX_POINT('',#23607);
#6863=VERTEX_POINT('',#23612);
#6864=VERTEX_POINT('',#23613);
#6865=VERTEX_POINT('',#23618);
#6866=VERTEX_POINT('',#23619);
#6867=VERTEX_POINT('',#23630);
#6868=VERTEX_POINT('',#23632);
#6869=VERTEX_POINT('',#23634);
#6870=VERTEX_POINT('',#23636);
#6871=VERTEX_POINT('',#23640);
#6872=VERTEX_POINT('',#23642);
#6873=VERTEX_POINT('',#23649);
#6874=VERTEX_POINT('',#23653);
#6875=VERTEX_POINT('',#23657);
#6876=VERTEX_POINT('',#23661);
#6877=VERTEX_POINT('',#23665);
#6878=VERTEX_POINT('',#23669);
#6879=VERTEX_POINT('',#23675);
#6880=VERTEX_POINT('',#23680);
#6881=VERTEX_POINT('',#23686);
#6882=VERTEX_POINT('',#23688);
#6883=VERTEX_POINT('',#23697);
#6884=VERTEX_POINT('',#23699);
#6885=VERTEX_POINT('',#23707);
#6886=VERTEX_POINT('',#23709);
#6887=VERTEX_POINT('',#23713);
#6888=VERTEX_POINT('',#23715);
#6889=VERTEX_POINT('',#23719);
#6890=VERTEX_POINT('',#23820);
#6891=VERTEX_POINT('',#23821);
#6892=VERTEX_POINT('',#23967);
#6893=VERTEX_POINT('',#23972);
#6894=VERTEX_POINT('',#23983);
#6895=VERTEX_POINT('',#23993);
#6896=VERTEX_POINT('',#24003);
#6897=VERTEX_POINT('',#24052);
#6898=VERTEX_POINT('',#24054);
#6899=VERTEX_POINT('',#24059);
#6900=VERTEX_POINT('',#24061);
#6901=VERTEX_POINT('',#24110);
#6902=VERTEX_POINT('',#24111);
#6903=VERTEX_POINT('',#24117);
#6904=VERTEX_POINT('',#24119);
#6905=VERTEX_POINT('',#24239);
#6906=VERTEX_POINT('',#24240);
#6907=VERTEX_POINT('',#24384);
#6908=VERTEX_POINT('',#24409);
#6909=VERTEX_POINT('',#24413);
#6910=VERTEX_POINT('',#24416);
#6911=VERTEX_POINT('',#24420);
#6912=VERTEX_POINT('',#24422);
#6913=VERTEX_POINT('',#24426);
#6914=VERTEX_POINT('',#24427);
#6915=VERTEX_POINT('',#24439);
#6916=VERTEX_POINT('',#24441);
#6917=VERTEX_POINT('',#24445);
#6918=VERTEX_POINT('',#24446);
#6919=VERTEX_POINT('',#24451);
#6920=VERTEX_POINT('',#24452);
#6921=VERTEX_POINT('',#24462);
#6922=VERTEX_POINT('',#24464);
#6923=VERTEX_POINT('',#24468);
#6924=VERTEX_POINT('',#24477);
#6925=VERTEX_POINT('',#24479);
#6926=VERTEX_POINT('',#24483);
#6927=VERTEX_POINT('',#24487);
#6928=VERTEX_POINT('',#24498);
#6929=VERTEX_POINT('',#24506);
#6930=VERTEX_POINT('',#24508);
#6931=VERTEX_POINT('',#24513);
#6932=VERTEX_POINT('',#24517);
#6933=VERTEX_POINT('',#24519);
#6934=VERTEX_POINT('',#24528);
#6935=VERTEX_POINT('',#24532);
#6936=VERTEX_POINT('',#24533);
#6937=VERTEX_POINT('',#24545);
#6938=VERTEX_POINT('',#24547);
#6939=VERTEX_POINT('',#24609);
#6940=VERTEX_POINT('',#24613);
#6941=VERTEX_POINT('',#24616);
#6942=VERTEX_POINT('',#24621);
#6943=VERTEX_POINT('',#24657);
#6944=VERTEX_POINT('',#24659);
#6945=VERTEX_POINT('',#24663);
#6946=VERTEX_POINT('',#24667);
#6947=VERTEX_POINT('',#24670);
#6948=VERTEX_POINT('',#24674);
#6949=VERTEX_POINT('',#24676);
#6950=VERTEX_POINT('',#24718);
#6951=VERTEX_POINT('',#24720);
#6952=VERTEX_POINT('',#24722);
#6953=VERTEX_POINT('',#24726);
#6954=VERTEX_POINT('',#24730);
#6955=VERTEX_POINT('',#24732);
#6956=VERTEX_POINT('',#24734);
#6957=VERTEX_POINT('',#24736);
#6958=VERTEX_POINT('',#24738);
#6959=VERTEX_POINT('',#24740);
#6960=VERTEX_POINT('',#24742);
#6961=VERTEX_POINT('',#24745);
#6962=VERTEX_POINT('',#24750);
#6963=VERTEX_POINT('',#24754);
#6964=VERTEX_POINT('',#24758);
#6965=VERTEX_POINT('',#24762);
#6966=VERTEX_POINT('',#24766);
#6967=VERTEX_POINT('',#24770);
#6968=VERTEX_POINT('',#24774);
#6969=VERTEX_POINT('',#24776);
#6970=VERTEX_POINT('',#24779);
#6971=VERTEX_POINT('',#24783);
#6972=VERTEX_POINT('',#24787);
#6973=VERTEX_POINT('',#24795);
#6974=VERTEX_POINT('',#24797);
#6975=VERTEX_POINT('',#24801);
#6976=VERTEX_POINT('',#24805);
#6977=VERTEX_POINT('',#24808);
#6978=VERTEX_POINT('',#24810);
#6979=VERTEX_POINT('',#24812);
#6980=VERTEX_POINT('',#24821);
#6981=VERTEX_POINT('',#24822);
#6982=VERTEX_POINT('',#24825);
#6983=VERTEX_POINT('',#24829);
#6984=VERTEX_POINT('',#24831);
#6985=VERTEX_POINT('',#24833);
#6986=VERTEX_POINT('',#24835);
#6987=VERTEX_POINT('',#24837);
#6988=VERTEX_POINT('',#24839);
#6989=VERTEX_POINT('',#24841);
#6990=VERTEX_POINT('',#24844);
#6991=VERTEX_POINT('',#24895);
#6992=VERTEX_POINT('',#24900);
#6993=VERTEX_POINT('',#24904);
#6994=VERTEX_POINT('',#24908);
#6995=VERTEX_POINT('',#24912);
#6996=VERTEX_POINT('',#24916);
#6997=VERTEX_POINT('',#24920);
#6998=VERTEX_POINT('',#24924);
#6999=VERTEX_POINT('',#24928);
#7000=VERTEX_POINT('',#24932);
#7001=VERTEX_POINT('',#24935);
#7002=VERTEX_POINT('',#24939);
#7003=VERTEX_POINT('',#24945);
#7004=VERTEX_POINT('',#24947);
#7005=VERTEX_POINT('',#24951);
#7006=VERTEX_POINT('',#24953);
#7007=VERTEX_POINT('',#24957);
#7008=VERTEX_POINT('',#24959);
#7009=VERTEX_POINT('',#24963);
#7010=VERTEX_POINT('',#24965);
#7011=VERTEX_POINT('',#24969);
#7012=VERTEX_POINT('',#24971);
#7013=VERTEX_POINT('',#24975);
#7014=VERTEX_POINT('',#24977);
#7015=VERTEX_POINT('',#24981);
#7016=VERTEX_POINT('',#24983);
#7017=VERTEX_POINT('',#24987);
#7018=VERTEX_POINT('',#24990);
#7019=VERTEX_POINT('',#24996);
#7020=VERTEX_POINT('',#24998);
#7021=VERTEX_POINT('',#25002);
#7022=VERTEX_POINT('',#25004);
#7023=VERTEX_POINT('',#25008);
#7024=VERTEX_POINT('',#25010);
#7025=VERTEX_POINT('',#25014);
#7026=VERTEX_POINT('',#25016);
#7027=VERTEX_POINT('',#25020);
#7028=VERTEX_POINT('',#25022);
#7029=VERTEX_POINT('',#25026);
#7030=VERTEX_POINT('',#25028);
#7031=VERTEX_POINT('',#25032);
#7032=VERTEX_POINT('',#25034);
#7033=VERTEX_POINT('',#25038);
#7034=VERTEX_POINT('',#25041);
#7035=VERTEX_POINT('',#25045);
#7036=VERTEX_POINT('',#25048);
#7037=VERTEX_POINT('',#25052);
#7038=VERTEX_POINT('',#25055);
#7039=VERTEX_POINT('',#25061);
#7040=VERTEX_POINT('',#25062);
#7041=VERTEX_POINT('',#25065);
#7042=VERTEX_POINT('',#25069);
#7043=VERTEX_POINT('',#25072);
#7044=VERTEX_POINT('',#25076);
#7045=VERTEX_POINT('',#25080);
#7046=VERTEX_POINT('',#25086);
#7047=VERTEX_POINT('',#25088);
#7048=VERTEX_POINT('',#25090);
#7049=VERTEX_POINT('',#25094);
#7050=VERTEX_POINT('',#25097);
#7051=VERTEX_POINT('',#25101);
#7052=VERTEX_POINT('',#25103);
#7053=VERTEX_POINT('',#25105);
#7054=VERTEX_POINT('',#25109);
#7055=VERTEX_POINT('',#25110);
#7056=VERTEX_POINT('',#25115);
#7057=VERTEX_POINT('',#25123);
#7058=VERTEX_POINT('',#25124);
#7059=VERTEX_POINT('',#25126);
#7060=VERTEX_POINT('',#25143);
#7061=VERTEX_POINT('',#25156);
#7062=VERTEX_POINT('',#25157);
#7063=VERTEX_POINT('',#25240);
#7064=VERTEX_POINT('',#25241);
#7065=VERTEX_POINT('',#25330);
#7066=VERTEX_POINT('',#25331);
#7067=VERTEX_POINT('',#25420);
#7068=VERTEX_POINT('',#25421);
#7069=VERTEX_POINT('',#25504);
#7070=VERTEX_POINT('',#25505);
#7071=VERTEX_POINT('',#25594);
#7072=VERTEX_POINT('',#25595);
#7073=VERTEX_POINT('',#25678);
#7074=VERTEX_POINT('',#25679);
#7075=VERTEX_POINT('',#25765);
#7076=VERTEX_POINT('',#25766);
#7077=VERTEX_POINT('',#25840);
#7078=VERTEX_POINT('',#25841);
#7079=VERTEX_POINT('',#25924);
#7080=VERTEX_POINT('',#25925);
#7081=VERTEX_POINT('',#26014);
#7082=VERTEX_POINT('',#26015);
#7083=VERTEX_POINT('',#26098);
#7084=VERTEX_POINT('',#26099);
#7085=VERTEX_POINT('',#26185);
#7086=VERTEX_POINT('',#26186);
#7087=VERTEX_POINT('',#26275);
#7088=VERTEX_POINT('',#26276);
#7089=VERTEX_POINT('',#26359);
#7090=VERTEX_POINT('',#26360);
#7091=VERTEX_POINT('',#26362);
#7092=VERTEX_POINT('',#26372);
#7093=VERTEX_POINT('',#26381);
#7094=VERTEX_POINT('',#26382);
#7095=VERTEX_POINT('',#26418);
#7096=VERTEX_POINT('',#26419);
#7097=VERTEX_POINT('',#26455);
#7098=VERTEX_POINT('',#26456);
#7099=VERTEX_POINT('',#26493);
#7100=VERTEX_POINT('',#26494);
#7101=VERTEX_POINT('',#26530);
#7102=VERTEX_POINT('',#26531);
#7103=VERTEX_POINT('',#26567);
#7104=VERTEX_POINT('',#26568);
#7105=VERTEX_POINT('',#26604);
#7106=VERTEX_POINT('',#26605);
#7107=VERTEX_POINT('',#26639);
#7108=VERTEX_POINT('',#26640);
#7109=VERTEX_POINT('',#26673);
#7110=VERTEX_POINT('',#26674);
#7111=VERTEX_POINT('',#26710);
#7112=VERTEX_POINT('',#26711);
#7113=VERTEX_POINT('',#26747);
#7114=VERTEX_POINT('',#26748);
#7115=VERTEX_POINT('',#26784);
#7116=VERTEX_POINT('',#26785);
#7117=VERTEX_POINT('',#26821);
#7118=VERTEX_POINT('',#26822);
#7119=VERTEX_POINT('',#26859);
#7120=VERTEX_POINT('',#26860);
#7121=VERTEX_POINT('',#26896);
#7122=VERTEX_POINT('',#26897);
#7123=VERTEX_POINT('',#26899);
#7124=VERTEX_POINT('',#26916);
#7125=VERTEX_POINT('',#26929);
#7126=VERTEX_POINT('',#26930);
#7127=VERTEX_POINT('',#27013);
#7128=VERTEX_POINT('',#27014);
#7129=VERTEX_POINT('',#27103);
#7130=VERTEX_POINT('',#27104);
#7131=VERTEX_POINT('',#27193);
#7132=VERTEX_POINT('',#27194);
#7133=VERTEX_POINT('',#27277);
#7134=VERTEX_POINT('',#27278);
#7135=VERTEX_POINT('',#27367);
#7136=VERTEX_POINT('',#27368);
#7137=VERTEX_POINT('',#27451);
#7138=VERTEX_POINT('',#27452);
#7139=VERTEX_POINT('',#27538);
#7140=VERTEX_POINT('',#27539);
#7141=VERTEX_POINT('',#27613);
#7142=VERTEX_POINT('',#27614);
#7143=VERTEX_POINT('',#27697);
#7144=VERTEX_POINT('',#27698);
#7145=VERTEX_POINT('',#27787);
#7146=VERTEX_POINT('',#27788);
#7147=VERTEX_POINT('',#27871);
#7148=VERTEX_POINT('',#27872);
#7149=VERTEX_POINT('',#27958);
#7150=VERTEX_POINT('',#27959);
#7151=VERTEX_POINT('',#28048);
#7152=VERTEX_POINT('',#28049);
#7153=VERTEX_POINT('',#28132);
#7154=VERTEX_POINT('',#28133);
#7155=VERTEX_POINT('',#28135);
#7156=VERTEX_POINT('',#28145);
#7157=VERTEX_POINT('',#28154);
#7158=VERTEX_POINT('',#28155);
#7159=VERTEX_POINT('',#28191);
#7160=VERTEX_POINT('',#28192);
#7161=VERTEX_POINT('',#28228);
#7162=VERTEX_POINT('',#28229);
#7163=VERTEX_POINT('',#28266);
#7164=VERTEX_POINT('',#28267);
#7165=VERTEX_POINT('',#28303);
#7166=VERTEX_POINT('',#28304);
#7167=VERTEX_POINT('',#28340);
#7168=VERTEX_POINT('',#28341);
#7169=VERTEX_POINT('',#28377);
#7170=VERTEX_POINT('',#28378);
#7171=VERTEX_POINT('',#28412);
#7172=VERTEX_POINT('',#28413);
#7173=VERTEX_POINT('',#28446);
#7174=VERTEX_POINT('',#28447);
#7175=VERTEX_POINT('',#28483);
#7176=VERTEX_POINT('',#28484);
#7177=VERTEX_POINT('',#28520);
#7178=VERTEX_POINT('',#28521);
#7179=VERTEX_POINT('',#28557);
#7180=VERTEX_POINT('',#28558);
#7181=VERTEX_POINT('',#28594);
#7182=VERTEX_POINT('',#28595);
#7183=VERTEX_POINT('',#28632);
#7184=VERTEX_POINT('',#28633);
#7185=VERTEX_POINT('',#28669);
#7186=VERTEX_POINT('',#28782);
#7187=VERTEX_POINT('',#28784);
#7188=VERTEX_POINT('',#29708);
#7189=VERTEX_POINT('',#29836);
#7190=VERTEX_POINT('',#31544);
#7191=VERTEX_POINT('',#31691);
#7192=VERTEX_POINT('',#31819);
#7193=VERTEX_POINT('',#31822);
#7194=VERTEX_POINT('',#32722);
#7195=VERTEX_POINT('',#32867);
#7196=VERTEX_POINT('',#32874);
#7197=VERTEX_POINT('',#32877);
#7198=VERTEX_POINT('',#32882);
#7199=VERTEX_POINT('',#32888);
#7200=VERTEX_POINT('',#32890);
#7201=VERTEX_POINT('',#32892);
#7202=VERTEX_POINT('',#32912);
#7203=VERTEX_POINT('',#32914);
#7204=VERTEX_POINT('',#32946);
#7205=VERTEX_POINT('',#32948);
#7206=VERTEX_POINT('',#32980);
#7207=VERTEX_POINT('',#32982);
#7208=VERTEX_POINT('',#33014);
#7209=VERTEX_POINT('',#33016);
#7210=VERTEX_POINT('',#33048);
#7211=VERTEX_POINT('',#33050);
#7212=VERTEX_POINT('',#33082);
#7213=VERTEX_POINT('',#33120);
#7214=VERTEX_POINT('',#33125);
#7215=VERTEX_POINT('',#33132);
#7216=VERTEX_POINT('',#33138);
#7217=VERTEX_POINT('',#33169);
#7218=VERTEX_POINT('',#33174);
#7219=VERTEX_POINT('',#33181);
#7220=VERTEX_POINT('',#33204);
#7221=VERTEX_POINT('',#33214);
#7222=VERTEX_POINT('',#33224);
#7223=VERTEX_POINT('',#33258);
#7224=VERTEX_POINT('',#33265);
#7225=VERTEX_POINT('',#33278);
#7226=VERTEX_POINT('',#33283);
#7227=VERTEX_POINT('',#33294);
#7228=VERTEX_POINT('',#33301);
#7229=VERTEX_POINT('',#33310);
#7230=VERTEX_POINT('',#33319);
#7231=VERTEX_POINT('',#33326);
#7232=VERTEX_POINT('',#33360);
#7233=VERTEX_POINT('',#33361);
#7234=VERTEX_POINT('',#33393);
#7235=VERTEX_POINT('',#33394);
#7236=VERTEX_POINT('',#33401);
#7237=VERTEX_POINT('',#33402);
#7238=VERTEX_POINT('',#33434);
#7239=VERTEX_POINT('',#33435);
#7240=VERTEX_POINT('',#33442);
#7241=VERTEX_POINT('',#33443);
#7242=VERTEX_POINT('',#33450);
#7243=VERTEX_POINT('',#33451);
#7244=VERTEX_POINT('',#33470);
#7245=VERTEX_POINT('',#33472);
#7246=VERTEX_POINT('',#33487);
#7247=VERTEX_POINT('',#33489);
#7248=VERTEX_POINT('',#33493);
#7249=VERTEX_POINT('',#33504);
#7250=VERTEX_POINT('',#33506);
#7251=VERTEX_POINT('',#33508);
#7252=VERTEX_POINT('',#33512);
#7253=VERTEX_POINT('',#33515);
#7254=VERTEX_POINT('',#33517);
#7255=VERTEX_POINT('',#33519);
#7256=VERTEX_POINT('',#33522);
#7257=VERTEX_POINT('',#33525);
#7258=VERTEX_POINT('',#33529);
#7259=VERTEX_POINT('',#33531);
#7260=VERTEX_POINT('',#33535);
#7261=VERTEX_POINT('',#33538);
#7262=VERTEX_POINT('',#33542);
#7263=VERTEX_POINT('',#33546);
#7264=VERTEX_POINT('',#33548);
#7265=VERTEX_POINT('',#33552);
#7266=VERTEX_POINT('',#33556);
#7267=VERTEX_POINT('',#33559);
#7268=VERTEX_POINT('',#33561);
#7269=VERTEX_POINT('',#33563);
#7270=VERTEX_POINT('',#33567);
#7271=VERTEX_POINT('',#33571);
#7272=VERTEX_POINT('',#33574);
#7273=VERTEX_POINT('',#33578);
#7274=VERTEX_POINT('',#33581);
#7275=VERTEX_POINT('',#33582);
#7276=VERTEX_POINT('',#33584);
#7277=VERTEX_POINT('',#33586);
#7278=VERTEX_POINT('',#33590);
#7279=VERTEX_POINT('',#33591);
#7280=VERTEX_POINT('',#33596);
#7281=VERTEX_POINT('',#33597);
#7282=VERTEX_POINT('',#33602);
#7283=VERTEX_POINT('',#33603);
#7284=VERTEX_POINT('',#33608);
#7285=VERTEX_POINT('',#33609);
#7286=VERTEX_POINT('',#33614);
#7287=VERTEX_POINT('',#33615);
#7288=VERTEX_POINT('',#33620);
#7289=VERTEX_POINT('',#33621);
#7290=VERTEX_POINT('',#33629);
#7291=VERTEX_POINT('',#33631);
#7292=VERTEX_POINT('',#33635);
#7293=VERTEX_POINT('',#33639);
#7294=VERTEX_POINT('',#33643);
#7295=VERTEX_POINT('',#33646);
#7296=VERTEX_POINT('',#33649);
#7297=VERTEX_POINT('',#33651);
#7298=VERTEX_POINT('',#33653);
#7299=VERTEX_POINT('',#33656);
#7300=VERTEX_POINT('',#33658);
#7301=VERTEX_POINT('',#33662);
#7302=VERTEX_POINT('',#33666);
#7303=VERTEX_POINT('',#33670);
#7304=VERTEX_POINT('',#33674);
#7305=VERTEX_POINT('',#33675);
#7306=VERTEX_POINT('',#33680);
#7307=VERTEX_POINT('',#33681);
#7308=VERTEX_POINT('',#33686);
#7309=VERTEX_POINT('',#33687);
#7310=VERTEX_POINT('',#33701);
#7311=VERTEX_POINT('',#33703);
#7312=VERTEX_POINT('',#33706);
#7313=VERTEX_POINT('',#33707);
#7314=VERTEX_POINT('',#33709);
#7315=VERTEX_POINT('',#33711);
#7316=VERTEX_POINT('',#33715);
#7317=VERTEX_POINT('',#33716);
#7318=VERTEX_POINT('',#33721);
#7319=VERTEX_POINT('',#33722);
#7320=VERTEX_POINT('',#33727);
#7321=VERTEX_POINT('',#33728);
#7322=VERTEX_POINT('',#33733);
#7323=VERTEX_POINT('',#33734);
#7324=VERTEX_POINT('',#33739);
#7325=VERTEX_POINT('',#33740);
#7326=VERTEX_POINT('',#33745);
#7327=VERTEX_POINT('',#33746);
#7328=VERTEX_POINT('',#33754);
#7329=VERTEX_POINT('',#33756);
#7330=VERTEX_POINT('',#33760);
#7331=VERTEX_POINT('',#33764);
#7332=VERTEX_POINT('',#33768);
#7333=VERTEX_POINT('',#33771);
#7334=VERTEX_POINT('',#33774);
#7335=VERTEX_POINT('',#33776);
#7336=VERTEX_POINT('',#33778);
#7337=VERTEX_POINT('',#33781);
#7338=VERTEX_POINT('',#33783);
#7339=VERTEX_POINT('',#33787);
#7340=VERTEX_POINT('',#33791);
#7341=VERTEX_POINT('',#33795);
#7342=VERTEX_POINT('',#33799);
#7343=VERTEX_POINT('',#33800);
#7344=VERTEX_POINT('',#33805);
#7345=VERTEX_POINT('',#33806);
#7346=VERTEX_POINT('',#33811);
#7347=VERTEX_POINT('',#33812);
#7348=VERTEX_POINT('',#33826);
#7349=VERTEX_POINT('',#33828);
#7350=VERTEX_POINT('',#33880);
#7351=VERTEX_POINT('',#33984);
#7352=VERTEX_POINT('',#34054);
#7353=VERTEX_POINT('',#34059);
#7354=VERTEX_POINT('',#34067);
#7355=VERTEX_POINT('',#34068);
#7356=VERTEX_POINT('',#34070);
#7357=VERTEX_POINT('',#34087);
#7358=VERTEX_POINT('',#34100);
#7359=VERTEX_POINT('',#34101);
#7360=VERTEX_POINT('',#34184);
#7361=VERTEX_POINT('',#34185);
#7362=VERTEX_POINT('',#34274);
#7363=VERTEX_POINT('',#34275);
#7364=VERTEX_POINT('',#34358);
#7365=VERTEX_POINT('',#34359);
#7366=VERTEX_POINT('',#34448);
#7367=VERTEX_POINT('',#34449);
#7368=VERTEX_POINT('',#34538);
#7369=VERTEX_POINT('',#34539);
#7370=VERTEX_POINT('',#34541);
#7371=VERTEX_POINT('',#34548);
#7372=VERTEX_POINT('',#34549);
#7373=VERTEX_POINT('',#34568);
#7374=VERTEX_POINT('',#34585);
#7375=VERTEX_POINT('',#34586);
#7376=VERTEX_POINT('',#34623);
#7377=VERTEX_POINT('',#34624);
#7378=VERTEX_POINT('',#34660);
#7379=VERTEX_POINT('',#34661);
#7380=VERTEX_POINT('',#34697);
#7381=VERTEX_POINT('',#34698);
#7382=VERTEX_POINT('',#34734);
#7383=VERTEX_POINT('',#34736);
#7384=VERTEX_POINT('',#34738);
#7385=VERTEX_POINT('',#34742);
#7386=VERTEX_POINT('',#34744);
#7387=VERTEX_POINT('',#34748);
#7388=VERTEX_POINT('',#34882);
#7389=VERTEX_POINT('',#35018);
#7390=VERTEX_POINT('',#35020);
#7391=VERTEX_POINT('',#35024);
#7392=VERTEX_POINT('',#35026);
#7393=VERTEX_POINT('',#35030);
#7394=VERTEX_POINT('',#35034);
#7395=VERTEX_POINT('',#35035);
#7396=VERTEX_POINT('',#35037);
#7397=VERTEX_POINT('',#35039);
#7398=VERTEX_POINT('',#35041);
#7399=VERTEX_POINT('',#35043);
#7400=VERTEX_POINT('',#35047);
#7401=VERTEX_POINT('',#35049);
#7402=VERTEX_POINT('',#35053);
#7403=VERTEX_POINT('',#35057);
#7404=VERTEX_POINT('',#35059);
#7405=VERTEX_POINT('',#35063);
#7406=VERTEX_POINT('',#35071);
#7407=VERTEX_POINT('',#35073);
#7408=VERTEX_POINT('',#35077);
#7409=VERTEX_POINT('',#35081);
#7410=VERTEX_POINT('',#35085);
#7411=VERTEX_POINT('',#35219);
#7412=VERTEX_POINT('',#35221);
#7413=VERTEX_POINT('',#36056);
#7414=VERTEX_POINT('',#36060);
#7415=VERTEX_POINT('',#36067);
#7416=VERTEX_POINT('',#36073);
#7417=VERTEX_POINT('',#36074);
#7418=VERTEX_POINT('',#36076);
#7419=VERTEX_POINT('',#36078);
#7420=VERTEX_POINT('',#36080);
#7421=VERTEX_POINT('',#36082);
#7422=VERTEX_POINT('',#36084);
#7423=VERTEX_POINT('',#36086);
#7424=VERTEX_POINT('',#36089);
#7425=VERTEX_POINT('',#36092);
#7426=VERTEX_POINT('',#36094);
#7427=VERTEX_POINT('',#36098);
#7428=VERTEX_POINT('',#36102);
#7429=VERTEX_POINT('',#36106);
#7430=VERTEX_POINT('',#36110);
#7431=VERTEX_POINT('',#36114);
#7432=VERTEX_POINT('',#36118);
#7433=VERTEX_POINT('',#36125);
#7434=VERTEX_POINT('',#36127);
#7435=VERTEX_POINT('',#36129);
#7436=VERTEX_POINT('',#36133);
#7437=VERTEX_POINT('',#36135);
#7438=VERTEX_POINT('',#36137);
#7439=VERTEX_POINT('',#36139);
#7440=VERTEX_POINT('',#36141);
#7441=VERTEX_POINT('',#36143);
#7442=VERTEX_POINT('',#36147);
#7443=VERTEX_POINT('',#36150);
#7444=VERTEX_POINT('',#36154);
#7445=VERTEX_POINT('',#36155);
#7446=VERTEX_POINT('',#36159);
#7447=VERTEX_POINT('',#36160);
#7448=VERTEX_POINT('',#36164);
#7449=VERTEX_POINT('',#36165);
#7450=VERTEX_POINT('',#36169);
#7451=VERTEX_POINT('',#36170);
#7452=VERTEX_POINT('',#36172);
#7453=VERTEX_POINT('',#36178);
#7454=VERTEX_POINT('',#36179);
#7455=VERTEX_POINT('',#36183);
#7456=VERTEX_POINT('',#36193);
#7457=VERTEX_POINT('',#36198);
#7458=VERTEX_POINT('',#36204);
#7459=VERTEX_POINT('',#36210);
#7460=VERTEX_POINT('',#36214);
#7461=VERTEX_POINT('',#36215);
#7462=VERTEX_POINT('',#36217);
#7463=VERTEX_POINT('',#36219);
#7464=VERTEX_POINT('',#36223);
#7465=VERTEX_POINT('',#36229);
#7466=VERTEX_POINT('',#36239);
#7467=VERTEX_POINT('',#36242);
#7468=VERTEX_POINT('',#36249);
#7469=VERTEX_POINT('',#36250);
#7470=VERTEX_POINT('',#36252);
#7471=VERTEX_POINT('',#36256);
#7472=VERTEX_POINT('',#36257);
#7473=VERTEX_POINT('',#36259);
#7474=VERTEX_POINT('',#36263);
#7475=VERTEX_POINT('',#36264);
#7476=VERTEX_POINT('',#36266);
#7477=VERTEX_POINT('',#36273);
#7478=VERTEX_POINT('',#36274);
#7479=VERTEX_POINT('',#36276);
#7480=VERTEX_POINT('',#36280);
#7481=VERTEX_POINT('',#36281);
#7482=VERTEX_POINT('',#36283);
#7483=VERTEX_POINT('',#36287);
#7484=VERTEX_POINT('',#36288);
#7485=VERTEX_POINT('',#36290);
#7486=VERTEX_POINT('',#36300);
#7487=VERTEX_POINT('',#36301);
#7488=VERTEX_POINT('',#36306);
#7489=VERTEX_POINT('',#36307);
#7490=VERTEX_POINT('',#36318);
#7491=VERTEX_POINT('',#36319);
#7492=VERTEX_POINT('',#36324);
#7493=VERTEX_POINT('',#36325);
#7494=VERTEX_POINT('',#36333);
#7495=VERTEX_POINT('',#36334);
#7496=VERTEX_POINT('',#36339);
#7497=VERTEX_POINT('',#36340);
#7498=VERTEX_POINT('',#36351);
#7499=VERTEX_POINT('',#36354);
#7500=VERTEX_POINT('',#36355);
#7501=VERTEX_POINT('',#36358);
#7502=VERTEX_POINT('',#36360);
#7503=VERTEX_POINT('',#36364);
#7504=VERTEX_POINT('',#36366);
#7505=VERTEX_POINT('',#36370);
#7506=VERTEX_POINT('',#36374);
#7507=VERTEX_POINT('',#36379);
#7508=VERTEX_POINT('',#36381);
#7509=VERTEX_POINT('',#36383);
#7510=VERTEX_POINT('',#36387);
#7511=VERTEX_POINT('',#36395);
#7512=VERTEX_POINT('',#36398);
#7513=VERTEX_POINT('',#36400);
#7514=VERTEX_POINT('',#36405);
#7515=VERTEX_POINT('',#36409);
#7516=VERTEX_POINT('',#36412);
#7517=VERTEX_POINT('',#36420);
#7518=VERTEX_POINT('',#36424);
#7519=VERTEX_POINT('',#36430);
#7520=VERTEX_POINT('',#36431);
#7521=VERTEX_POINT('',#36435);
#7522=VERTEX_POINT('',#36437);
#7523=VERTEX_POINT('',#36441);
#7524=VERTEX_POINT('',#36444);
#7525=VERTEX_POINT('',#36448);
#7526=VERTEX_POINT('',#36452);
#7527=VERTEX_POINT('',#36458);
#7528=VERTEX_POINT('',#36460);
#7529=VERTEX_POINT('',#36464);
#7530=VERTEX_POINT('',#36465);
#7531=VERTEX_POINT('',#36467);
#7532=VERTEX_POINT('',#36469);
#7533=VERTEX_POINT('',#36472);
#7534=VERTEX_POINT('',#36474);
#7535=VERTEX_POINT('',#36476);
#7536=VERTEX_POINT('',#36478);
#7537=VERTEX_POINT('',#36480);
#7538=VERTEX_POINT('',#36483);
#7539=VERTEX_POINT('',#36487);
#7540=VERTEX_POINT('',#36491);
#7541=VERTEX_POINT('',#36495);
#7542=VERTEX_POINT('',#36496);
#7543=VERTEX_POINT('',#36498);
#7544=VERTEX_POINT('',#36500);
#7545=VERTEX_POINT('',#36504);
#7546=VERTEX_POINT('',#36506);
#7547=VERTEX_POINT('',#36510);
#7548=VERTEX_POINT('',#36511);
#7549=VERTEX_POINT('',#36516);
#7550=VERTEX_POINT('',#36518);
#7551=VERTEX_POINT('',#36522);
#7552=VERTEX_POINT('',#36523);
#7553=VERTEX_POINT('',#36528);
#7554=VERTEX_POINT('',#36530);
#7555=VERTEX_POINT('',#36534);
#7556=VERTEX_POINT('',#36535);
#7557=VERTEX_POINT('',#36541);
#7558=VERTEX_POINT('',#36545);
#7559=VERTEX_POINT('',#36549);
#7560=VERTEX_POINT('',#36551);
#7561=VERTEX_POINT('',#36555);
#7562=VERTEX_POINT('',#36556);
#7563=VERTEX_POINT('',#36561);
#7564=VERTEX_POINT('',#36563);
#7565=VERTEX_POINT('',#36567);
#7566=VERTEX_POINT('',#36568);
#7567=VERTEX_POINT('',#36573);
#7568=VERTEX_POINT('',#36575);
#7569=VERTEX_POINT('',#36579);
#7570=VERTEX_POINT('',#36580);
#7571=VERTEX_POINT('',#36588);
#7572=VERTEX_POINT('',#36592);
#7573=VERTEX_POINT('',#36596);
#7574=VERTEX_POINT('',#36600);
#7575=VERTEX_POINT('',#36604);
#7576=VERTEX_POINT('',#36608);
#7577=VERTEX_POINT('',#36612);
#7578=VERTEX_POINT('',#36616);
#7579=VERTEX_POINT('',#36619);
#7580=VERTEX_POINT('',#36621);
#7581=VERTEX_POINT('',#36623);
#7582=VERTEX_POINT('',#36625);
#7583=VERTEX_POINT('',#36627);
#7584=VERTEX_POINT('',#36629);
#7585=VERTEX_POINT('',#36633);
#7586=VERTEX_POINT('',#36635);
#7587=VERTEX_POINT('',#36639);
#7588=VERTEX_POINT('',#36641);
#7589=VERTEX_POINT('',#36645);
#7590=VERTEX_POINT('',#36646);
#7591=VERTEX_POINT('',#36651);
#7592=VERTEX_POINT('',#36653);
#7593=VERTEX_POINT('',#36657);
#7594=VERTEX_POINT('',#36658);
#7595=VERTEX_POINT('',#36663);
#7596=VERTEX_POINT('',#36665);
#7597=VERTEX_POINT('',#36669);
#7598=VERTEX_POINT('',#36670);
#7599=VERTEX_POINT('',#36676);
#7600=VERTEX_POINT('',#36680);
#7601=VERTEX_POINT('',#36684);
#7602=VERTEX_POINT('',#36688);
#7603=VERTEX_POINT('',#36692);
#7604=VERTEX_POINT('',#36696);
#7605=VERTEX_POINT('',#36700);
#7606=VERTEX_POINT('',#36704);
#7607=VERTEX_POINT('',#36737);
#7608=VERTEX_POINT('',#36738);
#7609=VERTEX_POINT('',#36740);
#7610=VERTEX_POINT('',#36751);
#7611=VERTEX_POINT('',#36761);
#7612=VERTEX_POINT('',#36762);
#7613=VERTEX_POINT('',#36809);
#7614=VERTEX_POINT('',#36810);
#7615=VERTEX_POINT('',#36857);
#7616=VERTEX_POINT('',#36858);
#7617=VERTEX_POINT('',#36911);
#7618=VERTEX_POINT('',#36912);
#7619=VERTEX_POINT('',#36959);
#7620=VERTEX_POINT('',#36960);
#7621=VERTEX_POINT('',#37007);
#7622=VERTEX_POINT('',#37008);
#7623=VERTEX_POINT('',#37061);
#7624=VERTEX_POINT('',#37062);
#7625=VERTEX_POINT('',#37109);
#7626=VERTEX_POINT('',#37110);
#7627=VERTEX_POINT('',#37163);
#7628=VERTEX_POINT('',#37164);
#7629=VERTEX_POINT('',#37166);
#7630=VERTEX_POINT('',#37210);
#7631=VERTEX_POINT('',#37211);
#7632=VERTEX_POINT('',#37213);
#7633=VERTEX_POINT('',#37221);
#7634=VERTEX_POINT('',#37230);
#7635=VERTEX_POINT('',#37231);
#7636=VERTEX_POINT('',#37255);
#7637=VERTEX_POINT('',#37256);
#7638=VERTEX_POINT('',#37280);
#7639=VERTEX_POINT('',#37281);
#7640=VERTEX_POINT('',#37305);
#7641=VERTEX_POINT('',#37306);
#7642=VERTEX_POINT('',#37330);
#7643=VERTEX_POINT('',#37331);
#7644=VERTEX_POINT('',#37354);
#7645=VERTEX_POINT('',#37355);
#7646=VERTEX_POINT('',#37379);
#7647=VERTEX_POINT('',#37380);
#7648=VERTEX_POINT('',#37404);
#7649=VERTEX_POINT('',#37405);
#7650=VERTEX_POINT('',#37428);
#7651=VERTEX_POINT('',#37429);
#7652=VERTEX_POINT('',#37432);
#7653=VERTEX_POINT('',#37434);
#7654=VERTEX_POINT('',#37438);
#7655=VERTEX_POINT('',#37440);
#7656=VERTEX_POINT('',#37444);
#7657=VERTEX_POINT('',#37448);
#7658=VERTEX_POINT('',#37550);
#7659=VERTEX_POINT('',#37909);
#7660=VERTEX_POINT('',#38017);
#7661=VERTEX_POINT('',#38383);
#7662=VERTEX_POINT('',#38388);
#7663=VERTEX_POINT('',#38394);
#7664=VERTEX_POINT('',#38395);
#7665=VERTEX_POINT('',#38397);
#7666=VERTEX_POINT('',#38408);
#7667=VERTEX_POINT('',#38418);
#7668=VERTEX_POINT('',#38419);
#7669=VERTEX_POINT('',#38466);
#7670=VERTEX_POINT('',#38467);
#7671=VERTEX_POINT('',#38514);
#7672=VERTEX_POINT('',#38515);
#7673=VERTEX_POINT('',#38565);
#7674=VERTEX_POINT('',#38566);
#7675=VERTEX_POINT('',#38616);
#7676=VERTEX_POINT('',#38617);
#7677=VERTEX_POINT('',#38664);
#7678=VERTEX_POINT('',#38665);
#7679=VERTEX_POINT('',#38712);
#7680=VERTEX_POINT('',#38713);
#7681=VERTEX_POINT('',#38766);
#7682=VERTEX_POINT('',#38767);
#7683=VERTEX_POINT('',#38814);
#7684=VERTEX_POINT('',#38815);
#7685=VERTEX_POINT('',#38862);
#7686=VERTEX_POINT('',#38863);
#7687=VERTEX_POINT('',#38916);
#7688=VERTEX_POINT('',#38917);
#7689=VERTEX_POINT('',#38964);
#7690=VERTEX_POINT('',#38965);
#7691=VERTEX_POINT('',#39012);
#7692=VERTEX_POINT('',#39013);
#7693=VERTEX_POINT('',#39060);
#7694=VERTEX_POINT('',#39061);
#7695=VERTEX_POINT('',#39114);
#7696=VERTEX_POINT('',#39115);
#7697=VERTEX_POINT('',#39162);
#7698=VERTEX_POINT('',#39163);
#7699=VERTEX_POINT('',#39210);
#7700=VERTEX_POINT('',#39211);
#7701=VERTEX_POINT('',#39264);
#7702=VERTEX_POINT('',#39265);
#7703=VERTEX_POINT('',#39312);
#7704=VERTEX_POINT('',#39313);
#7705=VERTEX_POINT('',#39360);
#7706=VERTEX_POINT('',#39361);
#7707=VERTEX_POINT('',#39414);
#7708=VERTEX_POINT('',#39415);
#7709=VERTEX_POINT('',#39462);
#7710=VERTEX_POINT('',#39463);
#7711=VERTEX_POINT('',#39510);
#7712=VERTEX_POINT('',#39511);
#7713=VERTEX_POINT('',#39558);
#7714=VERTEX_POINT('',#39559);
#7715=VERTEX_POINT('',#39612);
#7716=VERTEX_POINT('',#39613);
#7717=VERTEX_POINT('',#39660);
#7718=VERTEX_POINT('',#39661);
#7719=VERTEX_POINT('',#39708);
#7720=VERTEX_POINT('',#39709);
#7721=VERTEX_POINT('',#39762);
#7722=VERTEX_POINT('',#39763);
#7723=VERTEX_POINT('',#39810);
#7724=VERTEX_POINT('',#39811);
#7725=VERTEX_POINT('',#39858);
#7726=VERTEX_POINT('',#39859);
#7727=VERTEX_POINT('',#39912);
#7728=VERTEX_POINT('',#39913);
#7729=VERTEX_POINT('',#39960);
#7730=VERTEX_POINT('',#39961);
#7731=VERTEX_POINT('',#40008);
#7732=VERTEX_POINT('',#40009);
#7733=VERTEX_POINT('',#40056);
#7734=VERTEX_POINT('',#40057);
#7735=VERTEX_POINT('',#40110);
#7736=VERTEX_POINT('',#40111);
#7737=VERTEX_POINT('',#40158);
#7738=VERTEX_POINT('',#40159);
#7739=VERTEX_POINT('',#40206);
#7740=VERTEX_POINT('',#40207);
#7741=VERTEX_POINT('',#40260);
#7742=VERTEX_POINT('',#40261);
#7743=VERTEX_POINT('',#40308);
#7744=VERTEX_POINT('',#40309);
#7745=VERTEX_POINT('',#40356);
#7746=VERTEX_POINT('',#40357);
#7747=VERTEX_POINT('',#40410);
#7748=VERTEX_POINT('',#40411);
#7749=VERTEX_POINT('',#40458);
#7750=VERTEX_POINT('',#40459);
#7751=VERTEX_POINT('',#40506);
#7752=VERTEX_POINT('',#40507);
#7753=VERTEX_POINT('',#40554);
#7754=VERTEX_POINT('',#40555);
#7755=VERTEX_POINT('',#40557);
#7756=VERTEX_POINT('',#40564);
#7757=VERTEX_POINT('',#40565);
#7758=VERTEX_POINT('',#40577);
#7759=VERTEX_POINT('',#40589);
#7760=VERTEX_POINT('',#40590);
#7761=VERTEX_POINT('',#40613);
#7762=VERTEX_POINT('',#40614);
#7763=VERTEX_POINT('',#40637);
#7764=VERTEX_POINT('',#40638);
#7765=VERTEX_POINT('',#40662);
#7766=VERTEX_POINT('',#40663);
#7767=VERTEX_POINT('',#40687);
#7768=VERTEX_POINT('',#40688);
#7769=VERTEX_POINT('',#40711);
#7770=VERTEX_POINT('',#40712);
#7771=VERTEX_POINT('',#40736);
#7772=VERTEX_POINT('',#40737);
#7773=VERTEX_POINT('',#40761);
#7774=VERTEX_POINT('',#40762);
#7775=VERTEX_POINT('',#40785);
#7776=VERTEX_POINT('',#40786);
#7777=VERTEX_POINT('',#40810);
#7778=VERTEX_POINT('',#40811);
#7779=VERTEX_POINT('',#40835);
#7780=VERTEX_POINT('',#40836);
#7781=VERTEX_POINT('',#40859);
#7782=VERTEX_POINT('',#40860);
#7783=VERTEX_POINT('',#40883);
#7784=VERTEX_POINT('',#40884);
#7785=VERTEX_POINT('',#40908);
#7786=VERTEX_POINT('',#40909);
#7787=VERTEX_POINT('',#40933);
#7788=VERTEX_POINT('',#40934);
#7789=VERTEX_POINT('',#40957);
#7790=VERTEX_POINT('',#40958);
#7791=VERTEX_POINT('',#40982);
#7792=VERTEX_POINT('',#40983);
#7793=VERTEX_POINT('',#41007);
#7794=VERTEX_POINT('',#41008);
#7795=VERTEX_POINT('',#41031);
#7796=VERTEX_POINT('',#41032);
#7797=VERTEX_POINT('',#41056);
#7798=VERTEX_POINT('',#41057);
#7799=VERTEX_POINT('',#41081);
#7800=VERTEX_POINT('',#41082);
#7801=VERTEX_POINT('',#41105);
#7802=VERTEX_POINT('',#41106);
#7803=VERTEX_POINT('',#41129);
#7804=VERTEX_POINT('',#41130);
#7805=VERTEX_POINT('',#41154);
#7806=VERTEX_POINT('',#41155);
#7807=VERTEX_POINT('',#41179);
#7808=VERTEX_POINT('',#41180);
#7809=VERTEX_POINT('',#41203);
#7810=VERTEX_POINT('',#41204);
#7811=VERTEX_POINT('',#41228);
#7812=VERTEX_POINT('',#41229);
#7813=VERTEX_POINT('',#41253);
#7814=VERTEX_POINT('',#41254);
#7815=VERTEX_POINT('',#41277);
#7816=VERTEX_POINT('',#41278);
#7817=VERTEX_POINT('',#41302);
#7818=VERTEX_POINT('',#41303);
#7819=VERTEX_POINT('',#41327);
#7820=VERTEX_POINT('',#41328);
#7821=VERTEX_POINT('',#41351);
#7822=VERTEX_POINT('',#41352);
#7823=VERTEX_POINT('',#41375);
#7824=VERTEX_POINT('',#41376);
#7825=VERTEX_POINT('',#41400);
#7826=VERTEX_POINT('',#41401);
#7827=VERTEX_POINT('',#41425);
#7828=VERTEX_POINT('',#41426);
#7829=VERTEX_POINT('',#41449);
#7830=VERTEX_POINT('',#41450);
#7831=VERTEX_POINT('',#41474);
#7832=VERTEX_POINT('',#41475);
#7833=VERTEX_POINT('',#41499);
#7834=VERTEX_POINT('',#41500);
#7835=VERTEX_POINT('',#41523);
#7836=VERTEX_POINT('',#41524);
#7837=VERTEX_POINT('',#41548);
#7838=VERTEX_POINT('',#41549);
#7839=VERTEX_POINT('',#41572);
#7840=VERTEX_POINT('',#41573);
#7841=VERTEX_POINT('',#41597);
#7842=VERTEX_POINT('',#41598);
#7843=VERTEX_POINT('',#42740);
#7844=VERTEX_POINT('',#42851);
#7845=VERTEX_POINT('',#42962);
#7846=VERTEX_POINT('',#42965);
#7847=VERTEX_POINT('',#44193);
#7848=VERTEX_POINT('',#44305);
#7849=VERTEX_POINT('',#44306);
#7850=VERTEX_POINT('',#44310);
#7851=VERTEX_POINT('',#44314);
#7852=VERTEX_POINT('',#44318);
#7853=VERTEX_POINT('',#44322);
#7854=VERTEX_POINT('',#44326);
#7855=VERTEX_POINT('',#44329);
#7856=VERTEX_POINT('',#44337);
#7857=VERTEX_POINT('',#44339);
#7858=VERTEX_POINT('',#44343);
#7859=VERTEX_POINT('',#44347);
#7860=VERTEX_POINT('',#44351);
#7861=VERTEX_POINT('',#44353);
#7862=VERTEX_POINT('',#44364);
#7863=VERTEX_POINT('',#44371);
#7864=VERTEX_POINT('',#44372);
#7865=VERTEX_POINT('',#44374);
#7866=VERTEX_POINT('',#44385);
#7867=VERTEX_POINT('',#44395);
#7868=VERTEX_POINT('',#44396);
#7869=VERTEX_POINT('',#44443);
#7870=VERTEX_POINT('',#44444);
#7871=VERTEX_POINT('',#44491);
#7872=VERTEX_POINT('',#44492);
#7873=VERTEX_POINT('',#44539);
#7874=VERTEX_POINT('',#44540);
#7875=VERTEX_POINT('',#44593);
#7876=VERTEX_POINT('',#44594);
#7877=VERTEX_POINT('',#44641);
#7878=VERTEX_POINT('',#44642);
#7879=VERTEX_POINT('',#44689);
#7880=VERTEX_POINT('',#44690);
#7881=VERTEX_POINT('',#44743);
#7882=VERTEX_POINT('',#44744);
#7883=VERTEX_POINT('',#44791);
#7884=VERTEX_POINT('',#44792);
#7885=VERTEX_POINT('',#44839);
#7886=VERTEX_POINT('',#44840);
#7887=VERTEX_POINT('',#44887);
#7888=VERTEX_POINT('',#44888);
#7889=VERTEX_POINT('',#44941);
#7890=VERTEX_POINT('',#44942);
#7891=VERTEX_POINT('',#44989);
#7892=VERTEX_POINT('',#44990);
#7893=VERTEX_POINT('',#45037);
#7894=VERTEX_POINT('',#45038);
#7895=VERTEX_POINT('',#45091);
#7896=VERTEX_POINT('',#45092);
#7897=VERTEX_POINT('',#45139);
#7898=VERTEX_POINT('',#45140);
#7899=VERTEX_POINT('',#45187);
#7900=VERTEX_POINT('',#45188);
#7901=VERTEX_POINT('',#45235);
#7902=VERTEX_POINT('',#45236);
#7903=VERTEX_POINT('',#45289);
#7904=VERTEX_POINT('',#45290);
#7905=VERTEX_POINT('',#45337);
#7906=VERTEX_POINT('',#45338);
#7907=VERTEX_POINT('',#45385);
#7908=VERTEX_POINT('',#45386);
#7909=VERTEX_POINT('',#45439);
#7910=VERTEX_POINT('',#45440);
#7911=VERTEX_POINT('',#45487);
#7912=VERTEX_POINT('',#45488);
#7913=VERTEX_POINT('',#45535);
#7914=VERTEX_POINT('',#45536);
#7915=VERTEX_POINT('',#45583);
#7916=VERTEX_POINT('',#45584);
#7917=VERTEX_POINT('',#45637);
#7918=VERTEX_POINT('',#45638);
#7919=VERTEX_POINT('',#45685);
#7920=VERTEX_POINT('',#45686);
#7921=VERTEX_POINT('',#45733);
#7922=VERTEX_POINT('',#45734);
#7923=VERTEX_POINT('',#45787);
#7924=VERTEX_POINT('',#45788);
#7925=VERTEX_POINT('',#45835);
#7926=VERTEX_POINT('',#45836);
#7927=VERTEX_POINT('',#45883);
#7928=VERTEX_POINT('',#45884);
#7929=VERTEX_POINT('',#45931);
#7930=VERTEX_POINT('',#45932);
#7931=VERTEX_POINT('',#45985);
#7932=VERTEX_POINT('',#45986);
#7933=VERTEX_POINT('',#46033);
#7934=VERTEX_POINT('',#46034);
#7935=VERTEX_POINT('',#46081);
#7936=VERTEX_POINT('',#46082);
#7937=VERTEX_POINT('',#46135);
#7938=VERTEX_POINT('',#46136);
#7939=VERTEX_POINT('',#46183);
#7940=VERTEX_POINT('',#46184);
#7941=VERTEX_POINT('',#46231);
#7942=VERTEX_POINT('',#46232);
#7943=VERTEX_POINT('',#46279);
#7944=VERTEX_POINT('',#46280);
#7945=VERTEX_POINT('',#46333);
#7946=VERTEX_POINT('',#46334);
#7947=VERTEX_POINT('',#46381);
#7948=VERTEX_POINT('',#46382);
#7949=VERTEX_POINT('',#46429);
#7950=VERTEX_POINT('',#46430);
#7951=VERTEX_POINT('',#46483);
#7952=VERTEX_POINT('',#46484);
#7953=VERTEX_POINT('',#46531);
#7954=VERTEX_POINT('',#46532);
#7955=VERTEX_POINT('',#46579);
#7956=VERTEX_POINT('',#46580);
#7957=VERTEX_POINT('',#46627);
#7958=VERTEX_POINT('',#46628);
#7959=VERTEX_POINT('',#46681);
#7960=VERTEX_POINT('',#46682);
#7961=VERTEX_POINT('',#46729);
#7962=VERTEX_POINT('',#46730);
#7963=VERTEX_POINT('',#46777);
#7964=VERTEX_POINT('',#46778);
#7965=VERTEX_POINT('',#46831);
#7966=VERTEX_POINT('',#46832);
#7967=VERTEX_POINT('',#46879);
#7968=VERTEX_POINT('',#46880);
#7969=VERTEX_POINT('',#46927);
#7970=VERTEX_POINT('',#46928);
#7971=VERTEX_POINT('',#46975);
#7972=VERTEX_POINT('',#46976);
#7973=VERTEX_POINT('',#47029);
#7974=VERTEX_POINT('',#47030);
#7975=VERTEX_POINT('',#47077);
#7976=VERTEX_POINT('',#47078);
#7977=VERTEX_POINT('',#47125);
#7978=VERTEX_POINT('',#47126);
#7979=VERTEX_POINT('',#47179);
#7980=VERTEX_POINT('',#47180);
#7981=VERTEX_POINT('',#47227);
#7982=VERTEX_POINT('',#47228);
#7983=VERTEX_POINT('',#47275);
#7984=VERTEX_POINT('',#47276);
#7985=VERTEX_POINT('',#47323);
#7986=VERTEX_POINT('',#47324);
#7987=VERTEX_POINT('',#47377);
#7988=VERTEX_POINT('',#47378);
#7989=VERTEX_POINT('',#47425);
#7990=VERTEX_POINT('',#47426);
#7991=VERTEX_POINT('',#47473);
#7992=VERTEX_POINT('',#47474);
#7993=VERTEX_POINT('',#47527);
#7994=VERTEX_POINT('',#47528);
#7995=VERTEX_POINT('',#47575);
#7996=VERTEX_POINT('',#47576);
#7997=VERTEX_POINT('',#47623);
#7998=VERTEX_POINT('',#47624);
#7999=VERTEX_POINT('',#47671);
#8000=VERTEX_POINT('',#47672);
#8001=VERTEX_POINT('',#47725);
#8002=VERTEX_POINT('',#47726);
#8003=VERTEX_POINT('',#47773);
#8004=VERTEX_POINT('',#47774);
#8005=VERTEX_POINT('',#47821);
#8006=VERTEX_POINT('',#47822);
#8007=VERTEX_POINT('',#47875);
#8008=VERTEX_POINT('',#47876);
#8009=VERTEX_POINT('',#47923);
#8010=VERTEX_POINT('',#47924);
#8011=VERTEX_POINT('',#47971);
#8012=VERTEX_POINT('',#47972);
#8013=VERTEX_POINT('',#48019);
#8014=VERTEX_POINT('',#48020);
#8015=VERTEX_POINT('',#48073);
#8016=VERTEX_POINT('',#48074);
#8017=VERTEX_POINT('',#48121);
#8018=VERTEX_POINT('',#48122);
#8019=VERTEX_POINT('',#48169);
#8020=VERTEX_POINT('',#48170);
#8021=VERTEX_POINT('',#48223);
#8022=VERTEX_POINT('',#48224);
#8023=VERTEX_POINT('',#48271);
#8024=VERTEX_POINT('',#48272);
#8025=VERTEX_POINT('',#48319);
#8026=VERTEX_POINT('',#48320);
#8027=VERTEX_POINT('',#48367);
#8028=VERTEX_POINT('',#48368);
#8029=VERTEX_POINT('',#48421);
#8030=VERTEX_POINT('',#48422);
#8031=VERTEX_POINT('',#48469);
#8032=VERTEX_POINT('',#48470);
#8033=VERTEX_POINT('',#48517);
#8034=VERTEX_POINT('',#48518);
#8035=VERTEX_POINT('',#48571);
#8036=VERTEX_POINT('',#48572);
#8037=VERTEX_POINT('',#48619);
#8038=VERTEX_POINT('',#48620);
#8039=VERTEX_POINT('',#48667);
#8040=VERTEX_POINT('',#48668);
#8041=VERTEX_POINT('',#48715);
#8042=VERTEX_POINT('',#48716);
#8043=VERTEX_POINT('',#48718);
#8044=VERTEX_POINT('',#48725);
#8045=VERTEX_POINT('',#48726);
#8046=VERTEX_POINT('',#48750);
#8047=VERTEX_POINT('',#48762);
#8048=VERTEX_POINT('',#48763);
#8049=VERTEX_POINT('',#48810);
#8050=VERTEX_POINT('',#48811);
#8051=VERTEX_POINT('',#48858);
#8052=VERTEX_POINT('',#48859);
#8053=VERTEX_POINT('',#48883);
#8054=VERTEX_POINT('',#48884);
#8055=VERTEX_POINT('',#48908);
#8056=VERTEX_POINT('',#48909);
#8057=VERTEX_POINT('',#48932);
#8058=VERTEX_POINT('',#48933);
#8059=VERTEX_POINT('',#48957);
#8060=VERTEX_POINT('',#48958);
#8061=VERTEX_POINT('',#48996);
#8062=VERTEX_POINT('',#48997);
#8063=VERTEX_POINT('',#49032);
#8064=VERTEX_POINT('',#49033);
#8065=VERTEX_POINT('',#49056);
#8066=VERTEX_POINT('',#49057);
#8067=VERTEX_POINT('',#49081);
#8068=VERTEX_POINT('',#49082);
#8069=VERTEX_POINT('',#49106);
#8070=VERTEX_POINT('',#49107);
#8071=VERTEX_POINT('',#49130);
#8072=VERTEX_POINT('',#49131);
#8073=VERTEX_POINT('',#49155);
#8074=VERTEX_POINT('',#49156);
#8075=VERTEX_POINT('',#49180);
#8076=VERTEX_POINT('',#49181);
#8077=VERTEX_POINT('',#49216);
#8078=VERTEX_POINT('',#49217);
#8079=VERTEX_POINT('',#49252);
#8080=VERTEX_POINT('',#49253);
#8081=VERTEX_POINT('',#49277);
#8082=VERTEX_POINT('',#49278);
#8083=VERTEX_POINT('',#49302);
#8084=VERTEX_POINT('',#49303);
#8085=VERTEX_POINT('',#49326);
#8086=VERTEX_POINT('',#49327);
#8087=VERTEX_POINT('',#49351);
#8088=VERTEX_POINT('',#49352);
#8089=VERTEX_POINT('',#49376);
#8090=VERTEX_POINT('',#49377);
#8091=VERTEX_POINT('',#49400);
#8092=VERTEX_POINT('',#49401);
#8093=VERTEX_POINT('',#49424);
#8094=VERTEX_POINT('',#49425);
#8095=VERTEX_POINT('',#49449);
#8096=VERTEX_POINT('',#49450);
#8097=VERTEX_POINT('',#49474);
#8098=VERTEX_POINT('',#49475);
#8099=VERTEX_POINT('',#49498);
#8100=VERTEX_POINT('',#49499);
#8101=VERTEX_POINT('',#49523);
#8102=VERTEX_POINT('',#49524);
#8103=VERTEX_POINT('',#49548);
#8104=VERTEX_POINT('',#49549);
#8105=VERTEX_POINT('',#49572);
#8106=VERTEX_POINT('',#49573);
#8107=VERTEX_POINT('',#49596);
#8108=VERTEX_POINT('',#49597);
#8109=VERTEX_POINT('',#49621);
#8110=VERTEX_POINT('',#49622);
#8111=VERTEX_POINT('',#49646);
#8112=VERTEX_POINT('',#49647);
#8113=VERTEX_POINT('',#49670);
#8114=VERTEX_POINT('',#49671);
#8115=VERTEX_POINT('',#49695);
#8116=VERTEX_POINT('',#49696);
#8117=VERTEX_POINT('',#49720);
#8118=VERTEX_POINT('',#49721);
#8119=VERTEX_POINT('',#49744);
#8120=VERTEX_POINT('',#49745);
#8121=VERTEX_POINT('',#49768);
#8122=VERTEX_POINT('',#49769);
#8123=VERTEX_POINT('',#49793);
#8124=VERTEX_POINT('',#49794);
#8125=VERTEX_POINT('',#49818);
#8126=VERTEX_POINT('',#49819);
#8127=VERTEX_POINT('',#49842);
#8128=VERTEX_POINT('',#49843);
#8129=VERTEX_POINT('',#49867);
#8130=VERTEX_POINT('',#49868);
#8131=VERTEX_POINT('',#49892);
#8132=VERTEX_POINT('',#49893);
#8133=VERTEX_POINT('',#49916);
#8134=VERTEX_POINT('',#49917);
#8135=VERTEX_POINT('',#49940);
#8136=VERTEX_POINT('',#49941);
#8137=VERTEX_POINT('',#49965);
#8138=VERTEX_POINT('',#49966);
#8139=VERTEX_POINT('',#49990);
#8140=VERTEX_POINT('',#49991);
#8141=VERTEX_POINT('',#50014);
#8142=VERTEX_POINT('',#50015);
#8143=VERTEX_POINT('',#50039);
#8144=VERTEX_POINT('',#50040);
#8145=VERTEX_POINT('',#50064);
#8146=VERTEX_POINT('',#50065);
#8147=VERTEX_POINT('',#50088);
#8148=VERTEX_POINT('',#50089);
#8149=VERTEX_POINT('',#50112);
#8150=VERTEX_POINT('',#50113);
#8151=VERTEX_POINT('',#50137);
#8152=VERTEX_POINT('',#50138);
#8153=VERTEX_POINT('',#50162);
#8154=VERTEX_POINT('',#50163);
#8155=VERTEX_POINT('',#50186);
#8156=VERTEX_POINT('',#50187);
#8157=VERTEX_POINT('',#50211);
#8158=VERTEX_POINT('',#50212);
#8159=VERTEX_POINT('',#50236);
#8160=VERTEX_POINT('',#50237);
#8161=VERTEX_POINT('',#50260);
#8162=VERTEX_POINT('',#50261);
#8163=VERTEX_POINT('',#50284);
#8164=VERTEX_POINT('',#50285);
#8165=VERTEX_POINT('',#50309);
#8166=VERTEX_POINT('',#50310);
#8167=VERTEX_POINT('',#50334);
#8168=VERTEX_POINT('',#50335);
#8169=VERTEX_POINT('',#50358);
#8170=VERTEX_POINT('',#50359);
#8171=VERTEX_POINT('',#50383);
#8172=VERTEX_POINT('',#50384);
#8173=VERTEX_POINT('',#50408);
#8174=VERTEX_POINT('',#50409);
#8175=VERTEX_POINT('',#50432);
#8176=VERTEX_POINT('',#50433);
#8177=VERTEX_POINT('',#50456);
#8178=VERTEX_POINT('',#50457);
#8179=VERTEX_POINT('',#50481);
#8180=VERTEX_POINT('',#50482);
#8181=VERTEX_POINT('',#50506);
#8182=VERTEX_POINT('',#50507);
#8183=VERTEX_POINT('',#50530);
#8184=VERTEX_POINT('',#50531);
#8185=VERTEX_POINT('',#50555);
#8186=VERTEX_POINT('',#50556);
#8187=VERTEX_POINT('',#50580);
#8188=VERTEX_POINT('',#50581);
#8189=VERTEX_POINT('',#50604);
#8190=VERTEX_POINT('',#50605);
#8191=VERTEX_POINT('',#50628);
#8192=VERTEX_POINT('',#50629);
#8193=VERTEX_POINT('',#50653);
#8194=VERTEX_POINT('',#50654);
#8195=VERTEX_POINT('',#50678);
#8196=VERTEX_POINT('',#50679);
#8197=VERTEX_POINT('',#50702);
#8198=VERTEX_POINT('',#50703);
#8199=VERTEX_POINT('',#50727);
#8200=VERTEX_POINT('',#50728);
#8201=VERTEX_POINT('',#50752);
#8202=VERTEX_POINT('',#50753);
#8203=VERTEX_POINT('',#50776);
#8204=VERTEX_POINT('',#50777);
#8205=VERTEX_POINT('',#50800);
#8206=VERTEX_POINT('',#50801);
#8207=VERTEX_POINT('',#50825);
#8208=VERTEX_POINT('',#50826);
#8209=VERTEX_POINT('',#50850);
#8210=VERTEX_POINT('',#50851);
#8211=VERTEX_POINT('',#50874);
#8212=VERTEX_POINT('',#50875);
#8213=VERTEX_POINT('',#50899);
#8214=VERTEX_POINT('',#50900);
#8215=VERTEX_POINT('',#50924);
#8216=VERTEX_POINT('',#50925);
#8217=VERTEX_POINT('',#50948);
#8218=VERTEX_POINT('',#50949);
#8219=VERTEX_POINT('',#53195);
#8220=VERTEX_POINT('',#53306);
#8221=VERTEX_POINT('',#53414);
#8222=VERTEX_POINT('',#53417);
#8223=VERTEX_POINT('',#55749);
#8224=VERTEX_POINT('',#55858);
#8225=VERTEX_POINT('',#55859);
#8226=VERTEX_POINT('',#55863);
#8227=VERTEX_POINT('',#55867);
#8228=VERTEX_POINT('',#55871);
#8229=VERTEX_POINT('',#55875);
#8230=VERTEX_POINT('',#55879);
#8231=VERTEX_POINT('',#55882);
#8232=VERTEX_POINT('',#55890);
#8233=VERTEX_POINT('',#55892);
#8234=VERTEX_POINT('',#55896);
#8235=VERTEX_POINT('',#55900);
#8236=VERTEX_POINT('',#55904);
#8237=VERTEX_POINT('',#55906);
#8238=VERTEX_POINT('',#55917);
#8239=VERTEX_POINT('',#55924);
#8240=VERTEX_POINT('',#55926);
#8241=VERTEX_POINT('',#55928);
#8242=VERTEX_POINT('',#55948);
#8243=VERTEX_POINT('',#55950);
#8244=VERTEX_POINT('',#55982);
#8245=VERTEX_POINT('',#55984);
#8246=VERTEX_POINT('',#56016);
#8247=VERTEX_POINT('',#56018);
#8248=VERTEX_POINT('',#56050);
#8249=VERTEX_POINT('',#56052);
#8250=VERTEX_POINT('',#56084);
#8251=VERTEX_POINT('',#56086);
#8252=VERTEX_POINT('',#56118);
#8253=VERTEX_POINT('',#56156);
#8254=VERTEX_POINT('',#56161);
#8255=VERTEX_POINT('',#56168);
#8256=VERTEX_POINT('',#56174);
#8257=VERTEX_POINT('',#56205);
#8258=VERTEX_POINT('',#56210);
#8259=VERTEX_POINT('',#56217);
#8260=VERTEX_POINT('',#56240);
#8261=VERTEX_POINT('',#56250);
#8262=VERTEX_POINT('',#56260);
#8263=VERTEX_POINT('',#56294);
#8264=VERTEX_POINT('',#56301);
#8265=VERTEX_POINT('',#56314);
#8266=VERTEX_POINT('',#56319);
#8267=VERTEX_POINT('',#56330);
#8268=VERTEX_POINT('',#56337);
#8269=VERTEX_POINT('',#56346);
#8270=VERTEX_POINT('',#56355);
#8271=VERTEX_POINT('',#56362);
#8272=VERTEX_POINT('',#56396);
#8273=VERTEX_POINT('',#56397);
#8274=VERTEX_POINT('',#56429);
#8275=VERTEX_POINT('',#56430);
#8276=VERTEX_POINT('',#56437);
#8277=VERTEX_POINT('',#56438);
#8278=VERTEX_POINT('',#56470);
#8279=VERTEX_POINT('',#56471);
#8280=VERTEX_POINT('',#56478);
#8281=VERTEX_POINT('',#56479);
#8282=VERTEX_POINT('',#56486);
#8283=VERTEX_POINT('',#56487);
#8284=VERTEX_POINT('',#56506);
#8285=VERTEX_POINT('',#56508);
#8286=VERTEX_POINT('',#56523);
#8287=VERTEX_POINT('',#56525);
#8288=VERTEX_POINT('',#56529);
#8289=EDGE_CURVE('',#6709,#6710,#5809,.F.);
#8290=EDGE_CURVE('',#6710,#6711,#3901,.T.);
#8291=EDGE_CURVE('',#6711,#6712,#3902,.F.);
#8292=EDGE_CURVE('',#6712,#6709,#3903,.T.);
#8293=EDGE_CURVE('',#6713,#6711,#3904,.T.);
#8294=EDGE_CURVE('',#6710,#6714,#5810,.T.);
#8295=EDGE_CURVE('',#6714,#6715,#3905,.T.);
#8296=EDGE_CURVE('',#6715,#6716,#3906,.T.);
#8297=EDGE_CURVE('',#6717,#6716,#1761,.T.);
#8298=EDGE_CURVE('',#6718,#6717,#3907,.T.);
#8299=EDGE_CURVE('',#6718,#6719,#3908,.T.);
#8300=EDGE_CURVE('',#6720,#6719,#5811,.F.);
#8301=EDGE_CURVE('',#6713,#6720,#3909,.T.);
#8302=EDGE_CURVE('',#6720,#6721,#5812,.F.);
#8303=EDGE_CURVE('',#6721,#6722,#3910,.T.);
#8304=EDGE_CURVE('',#6722,#6713,#3911,.F.);
#8305=EDGE_CURVE('',#6723,#6723,#662,.T.);
#8306=EDGE_CURVE('',#6723,#6724,#3912,.T.);
#8307=EDGE_CURVE('',#6709,#6724,#663,.T.);
#8308=EDGE_CURVE('',#6712,#6722,#664,.T.);
#8309=EDGE_CURVE('',#6724,#6721,#665,.T.);
#8310=EDGE_CURVE('',#6725,#6726,#5813,.F.);
#8311=EDGE_CURVE('',#6726,#6727,#3913,.T.);
#8312=EDGE_CURVE('',#6727,#6728,#3914,.F.);
#8313=EDGE_CURVE('',#6728,#6725,#3915,.T.);
#8314=EDGE_CURVE('',#6729,#6727,#3916,.T.);
#8315=EDGE_CURVE('',#6726,#6730,#5814,.T.);
#8316=EDGE_CURVE('',#6730,#6731,#3917,.T.);
#8317=EDGE_CURVE('',#6731,#6732,#3918,.T.);
#8318=EDGE_CURVE('',#6733,#6732,#1762,.T.);
#8319=EDGE_CURVE('',#6734,#6733,#3919,.T.);
#8320=EDGE_CURVE('',#6734,#6735,#3920,.T.);
#8321=EDGE_CURVE('',#6736,#6735,#5815,.F.);
#8322=EDGE_CURVE('',#6729,#6736,#3921,.T.);
#8323=EDGE_CURVE('',#6736,#6737,#5816,.F.);
#8324=EDGE_CURVE('',#6737,#6738,#3922,.T.);
#8325=EDGE_CURVE('',#6738,#6729,#3923,.F.);
#8326=EDGE_CURVE('',#6739,#6739,#666,.T.);
#8327=EDGE_CURVE('',#6739,#6740,#3924,.T.);
#8328=EDGE_CURVE('',#6725,#6740,#667,.T.);
#8329=EDGE_CURVE('',#6728,#6738,#668,.T.);
#8330=EDGE_CURVE('',#6740,#6737,#669,.T.);
#8331=EDGE_CURVE('',#6741,#6741,#670,.T.);
#8332=EDGE_CURVE('',#6741,#6723,#3925,.T.);
#8333=EDGE_CURVE('',#6742,#6743,#671,.T.);
#8334=EDGE_CURVE('',#6744,#6742,#3926,.T.);
#8335=EDGE_CURVE('',#6745,#6744,#672,.T.);
#8336=EDGE_CURVE('',#6746,#6745,#3927,.T.);
#8337=EDGE_CURVE('',#6747,#6746,#673,.T.);
#8338=EDGE_CURVE('',#6748,#6747,#3928,.T.);
#8339=EDGE_CURVE('',#6749,#6748,#674,.T.);
#8340=EDGE_CURVE('',#6743,#6749,#3929,.T.);
#8341=EDGE_CURVE('',#6750,#6750,#675,.T.);
#8342=EDGE_CURVE('',#6751,#6751,#676,.T.);
#8343=EDGE_CURVE('',#6750,#6739,#3930,.T.);
#8344=EDGE_CURVE('',#6752,#6752,#677,.T.);
#8345=EDGE_CURVE('',#6752,#6753,#3931,.T.);
#8346=EDGE_CURVE('',#6753,#6753,#678,.T.);
#8347=EDGE_CURVE('',#6754,#6755,#3932,.T.);
#8348=EDGE_CURVE('',#6756,#6754,#679,.T.);
#8349=EDGE_CURVE('',#6757,#6756,#3933,.T.);
#8350=EDGE_CURVE('',#6758,#6757,#680,.T.);
#8351=EDGE_CURVE('',#6759,#6758,#3934,.T.);
#8352=EDGE_CURVE('',#6760,#6759,#681,.T.);
#8353=EDGE_CURVE('',#6761,#6760,#3935,.T.);
#8354=EDGE_CURVE('',#6755,#6761,#682,.T.);
#8355=EDGE_CURVE('',#6762,#6762,#683,.T.);
#8356=EDGE_CURVE('',#6763,#6763,#684,.T.);
#8357=EDGE_CURVE('',#6753,#6764,#3936,.T.);
#8358=EDGE_CURVE('',#6764,#6764,#685,.T.);
#8359=EDGE_CURVE('',#6762,#6765,#3937,.T.);
#8360=EDGE_CURVE('',#6765,#6765,#686,.T.);
#8361=EDGE_CURVE('',#6765,#6766,#3938,.T.);
#8362=EDGE_CURVE('',#6766,#6766,#687,.T.);
#8363=EDGE_CURVE('',#6767,#6768,#5817,.F.);
#8364=EDGE_CURVE('',#6768,#6769,#688,.T.);
#8365=EDGE_CURVE('',#6769,#6770,#5818,.F.);
#8366=EDGE_CURVE('',#6770,#6767,#689,.T.);
#8367=EDGE_CURVE('',#6768,#6717,#5819,.T.);
#8368=EDGE_CURVE('',#6716,#6771,#5820,.T.);
#8369=EDGE_CURVE('',#6771,#6772,#690,.T.);
#8370=EDGE_CURVE('',#6772,#6773,#5821,.T.);
#8371=EDGE_CURVE('',#6773,#6774,#1763,.T.);
#8372=EDGE_CURVE('',#6774,#6769,#5822,.T.);
#8373=EDGE_CURVE('',#6775,#6776,#5823,.F.);
#8374=EDGE_CURVE('',#6776,#6777,#691,.T.);
#8375=EDGE_CURVE('',#6777,#6778,#5824,.F.);
#8376=EDGE_CURVE('',#6778,#6779,#692,.T.);
#8377=EDGE_CURVE('',#6779,#6775,#693,.T.);
#8378=EDGE_CURVE('',#6776,#6780,#5825,.T.);
#8379=EDGE_CURVE('',#6780,#6781,#1764,.T.);
#8380=EDGE_CURVE('',#6781,#6782,#5826,.T.);
#8381=EDGE_CURVE('',#6782,#6783,#694,.T.);
#8382=EDGE_CURVE('',#6783,#6733,#5827,.T.);
#8383=EDGE_CURVE('',#6732,#6777,#5828,.T.);
#8384=EDGE_CURVE('',#6784,#6784,#695,.T.);
#8385=EDGE_CURVE('',#6784,#6785,#696,.T.);
#8386=EDGE_CURVE('',#6785,#6786,#697,.T.);
#8387=EDGE_CURVE('',#6786,#6785,#698,.T.);
#8388=EDGE_CURVE('',#6786,#6779,#3939,.T.);
#8389=EDGE_CURVE('',#6778,#6787,#5829,.T.);
#8390=EDGE_CURVE('',#6787,#6788,#699,.T.);
#8391=EDGE_CURVE('',#6788,#6767,#5830,.T.);
#8392=EDGE_CURVE('',#6770,#6789,#5831,.T.);
#8393=EDGE_CURVE('',#6789,#6790,#700,.T.);
#8394=EDGE_CURVE('',#6790,#6775,#5832,.T.);
#8395=EDGE_CURVE('',#6791,#6792,#3940,.T.);
#8396=EDGE_CURVE('',#6792,#6793,#3941,.T.);
#8397=EDGE_CURVE('',#6793,#6794,#3942,.T.);
#8398=EDGE_CURVE('',#6794,#6791,#3943,.T.);
#8399=EDGE_CURVE('',#6795,#6796,#3944,.T.);
#8400=EDGE_CURVE('',#6796,#6797,#3945,.T.);
#8401=EDGE_CURVE('',#6797,#6798,#3946,.T.);
#8402=EDGE_CURVE('',#6798,#6795,#3947,.T.);
#8403=EDGE_CURVE('',#6799,#6800,#3948,.T.);
#8404=EDGE_CURVE('',#6800,#6801,#3949,.T.);
#8405=EDGE_CURVE('',#6801,#6802,#3950,.T.);
#8406=EDGE_CURVE('',#6802,#6799,#3951,.T.);
#8407=EDGE_CURVE('',#6803,#6804,#3952,.T.);
#8408=EDGE_CURVE('',#6804,#6805,#3953,.T.);
#8409=EDGE_CURVE('',#6805,#6806,#3954,.T.);
#8410=EDGE_CURVE('',#6806,#6803,#3955,.T.);
#8411=EDGE_CURVE('',#6807,#6808,#3956,.T.);
#8412=EDGE_CURVE('',#6808,#6809,#3957,.T.);
#8413=EDGE_CURVE('',#6809,#6810,#3958,.T.);
#8414=EDGE_CURVE('',#6810,#6807,#3959,.T.);
#8415=EDGE_CURVE('',#6811,#6812,#3960,.T.);
#8416=EDGE_CURVE('',#6812,#6813,#3961,.T.);
#8417=EDGE_CURVE('',#6813,#6814,#3962,.T.);
#8418=EDGE_CURVE('',#6814,#6811,#3963,.T.);
#8419=EDGE_CURVE('',#6815,#6816,#5833,.F.);
#8420=EDGE_CURVE('',#6817,#6816,#701,.T.);
#8421=EDGE_CURVE('',#6817,#6818,#5834,.F.);
#8422=EDGE_CURVE('',#6819,#6818,#5835,.T.);
#8423=EDGE_CURVE('',#6819,#6815,#702,.T.);
#8424=EDGE_CURVE('',#6820,#6819,#5836,.F.);
#8425=EDGE_CURVE('',#6820,#6821,#3964,.T.);
#8426=EDGE_CURVE('',#6821,#6783,#3965,.T.);
#8427=EDGE_CURVE('',#6782,#6822,#3966,.T.);
#8428=EDGE_CURVE('',#6822,#6823,#3967,.T.);
#8429=EDGE_CURVE('',#6815,#6823,#5837,.F.);
#8430=EDGE_CURVE('',#6824,#6824,#703,.T.);
#8431=EDGE_CURVE('',#6825,#6825,#704,.T.);
#8432=EDGE_CURVE('',#6826,#6826,#705,.T.);
#8433=EDGE_CURVE('',#6816,#6827,#5838,.F.);
#8434=EDGE_CURVE('',#6827,#6828,#706,.T.);
#8435=EDGE_CURVE('',#6828,#6829,#707,.T.);
#8436=EDGE_CURVE('',#6829,#6817,#5839,.F.);
#8437=EDGE_CURVE('',#6830,#6827,#5840,.F.);
#8438=EDGE_CURVE('',#6830,#6831,#5841,.T.);
#8439=EDGE_CURVE('',#6831,#6832,#708,.T.);
#8440=EDGE_CURVE('',#6832,#6833,#5842,.T.);
#8441=EDGE_CURVE('',#6833,#6834,#5843,.T.);
#8442=EDGE_CURVE('',#6835,#6834,#709,.T.);
#8443=EDGE_CURVE('',#6835,#6836,#5844,.T.);
#8444=EDGE_CURVE('',#6836,#6837,#710,.T.);
#8445=EDGE_CURVE('',#6837,#6829,#5845,.T.);
#8446=EDGE_CURVE('',#6828,#6838,#3968,.T.);
#8447=EDGE_CURVE('',#6838,#6838,#711,.T.);
#8448=EDGE_CURVE('',#6839,#6840,#5846,.T.);
#8449=EDGE_CURVE('',#6841,#6839,#712,.T.);
#8450=EDGE_CURVE('',#6842,#6841,#5847,.T.);
#8451=EDGE_CURVE('',#6842,#6843,#713,.T.);
#8452=EDGE_CURVE('',#6843,#6840,#5848,.F.);
#8453=EDGE_CURVE('',#6842,#6844,#5849,.T.);
#8454=EDGE_CURVE('',#6844,#6845,#3969,.T.);
#8455=EDGE_CURVE('',#6845,#6772,#3970,.T.);
#8456=EDGE_CURVE('',#6771,#6846,#3971,.T.);
#8457=EDGE_CURVE('',#6846,#6847,#3972,.T.);
#8458=EDGE_CURVE('',#6847,#6843,#5850,.T.);
#8459=EDGE_CURVE('',#6848,#6848,#714,.T.);
#8460=EDGE_CURVE('',#6849,#6849,#715,.T.);
#8461=EDGE_CURVE('',#6850,#6850,#716,.T.);
#8462=EDGE_CURVE('',#6834,#6841,#5851,.F.);
#8463=EDGE_CURVE('',#6839,#6835,#5852,.F.);
#8464=EDGE_CURVE('',#6838,#6851,#717,.T.);
#8465=EDGE_CURVE('',#6851,#6851,#718,.T.);
#8466=EDGE_CURVE('',#6852,#6852,#719,.T.);
#8467=EDGE_CURVE('',#6853,#6853,#720,.T.);
#8468=EDGE_CURVE('',#6854,#6854,#721,.T.);
#8469=EDGE_CURVE('',#6855,#6855,#722,.T.);
#8470=EDGE_CURVE('',#6856,#6856,#723,.T.);
#8471=EDGE_CURVE('',#6857,#6857,#724,.T.);
#8472=EDGE_CURVE('',#6858,#6858,#725,.T.);
#8473=EDGE_CURVE('',#6823,#6859,#726,.T.);
#8474=EDGE_CURVE('',#6859,#6860,#727,.T.);
#8475=EDGE_CURVE('',#6860,#6830,#728,.T.);
#8476=EDGE_CURVE('',#6861,#6862,#729,.T.);
#8477=EDGE_CURVE('',#6862,#6860,#3973,.T.);
#8478=EDGE_CURVE('',#6859,#6861,#3974,.T.);
#8479=EDGE_CURVE('',#6863,#6864,#730,.T.);
#8480=EDGE_CURVE('',#6864,#6862,#731,.T.);
#8481=EDGE_CURVE('',#6861,#6863,#732,.T.);
#8482=EDGE_CURVE('',#6865,#6866,#5853,.F.);
#8483=EDGE_CURVE('',#6866,#6864,#3975,.T.);
#8484=EDGE_CURVE('',#6863,#6865,#3976,.T.);
#8485=EDGE_CURVE('',#6790,#6866,#3977,.T.);
#8486=EDGE_CURVE('',#6789,#6867,#3978,.T.);
#8487=EDGE_CURVE('',#6868,#6867,#3979,.T.);
#8488=EDGE_CURVE('',#6868,#6869,#3980,.T.);
#8489=EDGE_CURVE('',#6870,#6869,#3981,.T.);
#8490=EDGE_CURVE('',#6864,#6870,#3982,.T.);
#8491=EDGE_CURVE('',#6871,#6822,#733,.T.);
#8492=EDGE_CURVE('',#6872,#6871,#3983,.T.);
#8493=EDGE_CURVE('',#6865,#6872,#734,.T.);
#8494=EDGE_CURVE('',#6755,#6870,#735,.T.);
#8495=EDGE_CURVE('',#6869,#6754,#736,.T.);
#8496=EDGE_CURVE('',#6873,#6756,#737,.T.);
#8497=EDGE_CURVE('',#6869,#6873,#738,.T.);
#8498=EDGE_CURVE('',#6874,#6757,#739,.T.);
#8499=EDGE_CURVE('',#6873,#6874,#3984,.T.);
#8500=EDGE_CURVE('',#6875,#6758,#740,.T.);
#8501=EDGE_CURVE('',#6874,#6875,#741,.T.);
#8502=EDGE_CURVE('',#6876,#6759,#742,.T.);
#8503=EDGE_CURVE('',#6875,#6876,#3985,.T.);
#8504=EDGE_CURVE('',#6877,#6760,#743,.T.);
#8505=EDGE_CURVE('',#6876,#6877,#744,.T.);
#8506=EDGE_CURVE('',#6878,#6761,#745,.T.);
#8507=EDGE_CURVE('',#6877,#6878,#3986,.T.);
#8508=EDGE_CURVE('',#6878,#6870,#746,.T.);
#8509=EDGE_CURVE('',#6879,#6874,#3987,.T.);
#8510=EDGE_CURVE('',#6833,#6879,#747,.T.);
#8511=EDGE_CURVE('',#6832,#6875,#3988,.T.);
#8512=EDGE_CURVE('',#6880,#6873,#3989,.T.);
#8513=EDGE_CURVE('',#6879,#6880,#3990,.T.);
#8514=EDGE_CURVE('',#6880,#6868,#748,.T.);
#8515=EDGE_CURVE('',#6881,#6868,#749,.T.);
#8516=EDGE_CURVE('',#6867,#6882,#5854,.F.);
#8517=EDGE_CURVE('',#6882,#6881,#3991,.T.);
#8518=EDGE_CURVE('',#6880,#6883,#750,.T.);
#8519=EDGE_CURVE('',#6883,#6884,#3992,.T.);
#8520=EDGE_CURVE('',#6884,#6879,#751,.T.);
#8521=EDGE_CURVE('',#6884,#6844,#752,.T.);
#8522=EDGE_CURVE('',#6881,#6883,#753,.T.);
#8523=EDGE_CURVE('',#6885,#6882,#754,.T.);
#8524=EDGE_CURVE('',#6886,#6885,#3993,.T.);
#8525=EDGE_CURVE('',#6845,#6886,#755,.T.);
#8526=EDGE_CURVE('',#6858,#6887,#756,.T.);
#8527=EDGE_CURVE('',#6887,#6888,#757,.T.);
#8528=EDGE_CURVE('',#6888,#6887,#758,.T.);
#8529=EDGE_CURVE('',#6888,#6889,#3994,.T.);
#8530=EDGE_CURVE('',#6889,#6889,#759,.T.);
#8531=EDGE_CURVE('',#6890,#6891,#5855,.T.);
#8532=EDGE_CURVE('',#6891,#6892,#5856,.T.);
#8533=EDGE_CURVE('',#6892,#6893,#5857,.T.);
#8534=EDGE_CURVE('',#6893,#6894,#5858,.T.);
#8535=EDGE_CURVE('',#6894,#6895,#5859,.T.);
#8536=EDGE_CURVE('',#6895,#6896,#5860,.T.);
#8537=EDGE_CURVE('',#6896,#6890,#5861,.T.);
#8538=EDGE_CURVE('',#6897,#6893,#3995,.T.);
#8539=EDGE_CURVE('',#6892,#6898,#5862,.T.);
#8540=EDGE_CURVE('',#6898,#6899,#3996,.T.);
#8541=EDGE_CURVE('',#6899,#6900,#5863,.T.);
#8542=EDGE_CURVE('',#6897,#6900,#5864,.T.);
#8543=EDGE_CURVE('',#6901,#6902,#3997,.T.);
#8544=EDGE_CURVE('',#6902,#6896,#5865,.T.);
#8545=EDGE_CURVE('',#6895,#6903,#3998,.T.);
#8546=EDGE_CURVE('',#6903,#6904,#5866,.T.);
#8547=EDGE_CURVE('',#6904,#6901,#5867,.T.);
#8548=EDGE_CURVE('',#6905,#6906,#5868,.T.);
#8549=EDGE_CURVE('',#6904,#6906,#5869,.T.);
#8550=EDGE_CURVE('',#6903,#6907,#5870,.T.);
#8551=EDGE_CURVE('',#6907,#6897,#5871,.T.);
#8552=EDGE_CURVE('',#6900,#6905,#5872,.T.);
#8553=EDGE_CURVE('',#6908,#6898,#760,.T.);
#8554=EDGE_CURVE('',#6899,#6908,#761,.T.);
#8555=EDGE_CURVE('',#6909,#6909,#762,.T.);
#8556=EDGE_CURVE('',#6909,#6894,#3999,.T.);
#8557=EDGE_CURVE('',#6907,#6910,#4000,.T.);
#8558=EDGE_CURVE('',#6910,#6910,#763,.T.);
#8559=EDGE_CURVE('',#6818,#6911,#764,.T.);
#8560=EDGE_CURVE('',#6911,#6912,#765,.T.);
#8561=EDGE_CURVE('',#6912,#6820,#766,.T.);
#8562=EDGE_CURVE('',#6913,#6914,#5873,.T.);
#8563=EDGE_CURVE('',#6914,#6912,#4001,.T.);
#8564=EDGE_CURVE('',#6911,#6915,#4002,.T.);
#8565=EDGE_CURVE('',#6915,#6916,#767,.T.);
#8566=EDGE_CURVE('',#6916,#6913,#4003,.T.);
#8567=EDGE_CURVE('',#6917,#6918,#768,.T.);
#8568=EDGE_CURVE('',#6918,#6916,#769,.T.);
#8569=EDGE_CURVE('',#6915,#6917,#770,.T.);
#8570=EDGE_CURVE('',#6919,#6920,#5874,.F.);
#8571=EDGE_CURVE('',#6920,#6918,#4004,.T.);
#8572=EDGE_CURVE('',#6917,#6919,#4005,.T.);
#8573=EDGE_CURVE('',#6921,#6911,#4006,.T.);
#8574=EDGE_CURVE('',#6922,#6921,#4007,.T.);
#8575=EDGE_CURVE('',#6922,#6915,#4008,.T.);
#8576=EDGE_CURVE('',#6923,#6837,#4009,.T.);
#8577=EDGE_CURVE('',#6921,#6923,#771,.T.);
#8578=EDGE_CURVE('',#6735,#6914,#772,.T.);
#8579=EDGE_CURVE('',#6821,#6734,#773,.T.);
#8580=EDGE_CURVE('',#6913,#6730,#774,.T.);
#8581=EDGE_CURVE('',#6924,#6742,#775,.T.);
#8582=EDGE_CURVE('',#6743,#6925,#776,.T.);
#8583=EDGE_CURVE('',#6925,#6924,#777,.T.);
#8584=EDGE_CURVE('',#6749,#6926,#778,.T.);
#8585=EDGE_CURVE('',#6926,#6925,#4010,.T.);
#8586=EDGE_CURVE('',#6748,#6927,#779,.T.);
#8587=EDGE_CURVE('',#6927,#6926,#780,.T.);
#8588=EDGE_CURVE('',#6747,#6923,#781,.T.);
#8589=EDGE_CURVE('',#6923,#6927,#4011,.T.);
#8590=EDGE_CURVE('',#6746,#6921,#782,.T.);
#8591=EDGE_CURVE('',#6745,#6922,#783,.T.);
#8592=EDGE_CURVE('',#6744,#6928,#784,.T.);
#8593=EDGE_CURVE('',#6928,#6922,#785,.T.);
#8594=EDGE_CURVE('',#6924,#6928,#4012,.T.);
#8595=EDGE_CURVE('',#6928,#6917,#4013,.T.);
#8596=EDGE_CURVE('',#6924,#6929,#4014,.T.);
#8597=EDGE_CURVE('',#6930,#6929,#4015,.T.);
#8598=EDGE_CURVE('',#6930,#6788,#4016,.T.);
#8599=EDGE_CURVE('',#6919,#6787,#4017,.T.);
#8600=EDGE_CURVE('',#6925,#6931,#4018,.T.);
#8601=EDGE_CURVE('',#6929,#6931,#786,.T.);
#8602=EDGE_CURVE('',#6929,#6932,#787,.T.);
#8603=EDGE_CURVE('',#6932,#6933,#4019,.T.);
#8604=EDGE_CURVE('',#6933,#6930,#5875,.F.);
#8605=EDGE_CURVE('',#6931,#6934,#788,.T.);
#8606=EDGE_CURVE('',#6934,#6932,#789,.T.);
#8607=EDGE_CURVE('',#6935,#6936,#5876,.T.);
#8608=EDGE_CURVE('',#6936,#6934,#4020,.T.);
#8609=EDGE_CURVE('',#6931,#6937,#4021,.T.);
#8610=EDGE_CURVE('',#6937,#6938,#790,.T.);
#8611=EDGE_CURVE('',#6938,#6935,#4022,.T.);
#8612=EDGE_CURVE('',#6847,#6938,#791,.T.);
#8613=EDGE_CURVE('',#6937,#6840,#792,.T.);
#8614=EDGE_CURVE('',#6715,#6846,#793,.T.);
#8615=EDGE_CURVE('',#6935,#6714,#794,.T.);
#8616=EDGE_CURVE('',#6719,#6936,#795,.T.);
#8617=EDGE_CURVE('',#6933,#6718,#796,.T.);
#8618=EDGE_CURVE('',#6791,#6794,#797,.T.);
#8619=EDGE_CURVE('',#6793,#6792,#798,.T.);
#8620=EDGE_CURVE('',#6795,#6798,#799,.T.);
#8621=EDGE_CURVE('',#6797,#6796,#800,.T.);
#8622=EDGE_CURVE('',#6799,#6802,#801,.T.);
#8623=EDGE_CURVE('',#6801,#6800,#802,.T.);
#8624=EDGE_CURVE('',#6803,#6806,#803,.T.);
#8625=EDGE_CURVE('',#6805,#6804,#804,.T.);
#8626=EDGE_CURVE('',#6807,#6810,#805,.T.);
#8627=EDGE_CURVE('',#6809,#6808,#806,.T.);
#8628=EDGE_CURVE('',#6811,#6814,#807,.T.);
#8629=EDGE_CURVE('',#6813,#6812,#808,.T.);
#8630=EDGE_CURVE('',#6731,#6920,#809,.T.);
#8631=EDGE_CURVE('',#6852,#6826,#4023,.T.);
#8632=EDGE_CURVE('',#6853,#6850,#4024,.T.);
#8633=EDGE_CURVE('',#6854,#6849,#4025,.T.);
#8634=EDGE_CURVE('',#6855,#6825,#4026,.T.);
#8635=EDGE_CURVE('',#6856,#6824,#4027,.T.);
#8636=EDGE_CURVE('',#6857,#6848,#4028,.T.);
#8637=EDGE_CURVE('',#6751,#6939,#4029,.T.);
#8638=EDGE_CURVE('',#6939,#6939,#810,.T.);
#8639=EDGE_CURVE('',#6940,#6940,#811,.T.);
#8640=EDGE_CURVE('',#6940,#6941,#4030,.T.);
#8641=EDGE_CURVE('',#6941,#6941,#812,.T.);
#8642=EDGE_CURVE('',#6942,#6942,#813,.T.);
#8643=EDGE_CURVE('',#6942,#6763,#4031,.T.);
#8644=EDGE_CURVE('',#6889,#6908,#4032,.T.);
#8645=EDGE_CURVE('',#6902,#6901,#814,.T.);
#8646=EDGE_CURVE('',#6862,#6878,#4033,.T.);
#8647=EDGE_CURVE('',#6860,#6877,#4034,.T.);
#8648=EDGE_CURVE('',#6831,#6876,#4035,.T.);
#8649=EDGE_CURVE('',#6927,#6836,#4036,.T.);
#8650=EDGE_CURVE('',#6926,#6937,#4037,.T.);
#8651=EDGE_CURVE('',#6781,#6871,#4038,.T.);
#8652=EDGE_CURVE('',#6780,#6872,#4039,.T.);
#8653=EDGE_CURVE('',#6773,#6886,#4040,.T.);
#8654=EDGE_CURVE('',#6774,#6885,#4041,.T.);
#8655=EDGE_CURVE('',#6943,#6943,#815,.T.);
#8656=EDGE_CURVE('',#6943,#6944,#4042,.T.);
#8657=EDGE_CURVE('',#6944,#6944,#816,.T.);
#8658=EDGE_CURVE('',#6943,#6945,#4043,.T.);
#8659=EDGE_CURVE('',#6945,#6945,#817,.T.);
#8660=EDGE_CURVE('',#6946,#6946,#818,.T.);
#8661=EDGE_CURVE('',#6945,#6947,#4044,.T.);
#8662=EDGE_CURVE('',#6947,#6947,#819,.T.);
#8663=EDGE_CURVE('',#6947,#6948,#4045,.T.);
#8664=EDGE_CURVE('',#6949,#6948,#5877,.T.);
#8665=EDGE_CURVE('',#6948,#6949,#5878,.T.);
#8666=EDGE_CURVE('',#6950,#6950,#820,.T.);
#8667=EDGE_CURVE('',#6950,#6951,#4046,.T.);
#8668=EDGE_CURVE('',#6951,#6952,#821,.T.);
#8669=EDGE_CURVE('',#6952,#6951,#822,.T.);
#8670=EDGE_CURVE('',#6952,#6953,#4047,.T.);
#8671=EDGE_CURVE('',#6953,#6953,#823,.T.);
#8672=EDGE_CURVE('',#6954,#6954,#824,.T.);
#8673=EDGE_CURVE('',#6955,#6955,#825,.T.);
#8674=EDGE_CURVE('',#6956,#6956,#826,.T.);
#8675=EDGE_CURVE('',#6957,#6957,#827,.T.);
#8676=EDGE_CURVE('',#6958,#6958,#828,.T.);
#8677=EDGE_CURVE('',#6959,#6959,#829,.T.);
#8678=EDGE_CURVE('',#6960,#6960,#830,.T.);
#8679=EDGE_CURVE('',#6946,#6961,#4048,.T.);
#8680=EDGE_CURVE('',#6961,#6961,#831,.T.);
#8681=EDGE_CURVE('',#6954,#6962,#4049,.T.);
#8682=EDGE_CURVE('',#6962,#6962,#832,.T.);
#8683=EDGE_CURVE('',#6955,#6963,#4050,.T.);
#8684=EDGE_CURVE('',#6963,#6963,#833,.T.);
#8685=EDGE_CURVE('',#6956,#6964,#4051,.T.);
#8686=EDGE_CURVE('',#6964,#6964,#834,.T.);
#8687=EDGE_CURVE('',#6957,#6965,#4052,.T.);
#8688=EDGE_CURVE('',#6965,#6965,#835,.T.);
#8689=EDGE_CURVE('',#6958,#6966,#4053,.T.);
#8690=EDGE_CURVE('',#6966,#6966,#836,.T.);
#8691=EDGE_CURVE('',#6959,#6967,#4054,.T.);
#8692=EDGE_CURVE('',#6967,#6967,#837,.T.);
#8693=EDGE_CURVE('',#6968,#6968,#838,.T.);
#8694=EDGE_CURVE('',#6969,#6969,#839,.T.);
#8695=EDGE_CURVE('',#6968,#6970,#4055,.T.);
#8696=EDGE_CURVE('',#6970,#6970,#840,.T.);
#8697=EDGE_CURVE('',#6970,#6971,#4056,.T.);
#8698=EDGE_CURVE('',#6971,#6971,#841,.T.);
#8699=EDGE_CURVE('',#6972,#6972,#842,.T.);
#8700=EDGE_CURVE('',#6953,#6972,#4057,.T.);
#8701=EDGE_CURVE('',#6960,#6969,#4058,.T.);
#8702=EDGE_CURVE('',#6973,#6973,#843,.T.);
#8703=EDGE_CURVE('',#6973,#6974,#4059,.T.);
#8704=EDGE_CURVE('',#6974,#6974,#844,.T.);
#8705=EDGE_CURVE('',#6973,#6975,#4060,.T.);
#8706=EDGE_CURVE('',#6975,#6975,#845,.T.);
#8707=EDGE_CURVE('',#6976,#6976,#846,.T.);
#8708=EDGE_CURVE('',#6975,#6977,#4061,.T.);
#8709=EDGE_CURVE('',#6977,#6978,#847,.T.);
#8710=EDGE_CURVE('',#6979,#6978,#5879,.T.);
#8711=EDGE_CURVE('',#6979,#6977,#848,.T.);
#8712=EDGE_CURVE('',#6980,#6981,#849,.T.);
#8713=EDGE_CURVE('',#6981,#6980,#850,.T.);
#8714=EDGE_CURVE('',#6980,#6982,#4062,.T.);
#8715=EDGE_CURVE('',#6982,#6982,#851,.T.);
#8716=EDGE_CURVE('',#6983,#6983,#852,.T.);
#8717=EDGE_CURVE('',#6984,#6984,#853,.T.);
#8718=EDGE_CURVE('',#6985,#6985,#854,.T.);
#8719=EDGE_CURVE('',#6986,#6986,#855,.T.);
#8720=EDGE_CURVE('',#6987,#6987,#856,.T.);
#8721=EDGE_CURVE('',#6988,#6988,#857,.T.);
#8722=EDGE_CURVE('',#6989,#6989,#858,.T.);
#8723=EDGE_CURVE('',#6990,#6990,#859,.T.);
#8724=EDGE_CURVE('',#6990,#6981,#4063,.T.);
#8725=EDGE_CURVE('',#6978,#6979,#5880,.T.);
#8726=EDGE_CURVE('',#6976,#6991,#4064,.T.);
#8727=EDGE_CURVE('',#6991,#6991,#860,.T.);
#8728=EDGE_CURVE('',#6983,#6992,#4065,.T.);
#8729=EDGE_CURVE('',#6992,#6992,#861,.T.);
#8730=EDGE_CURVE('',#6984,#6993,#4066,.T.);
#8731=EDGE_CURVE('',#6993,#6993,#862,.T.);
#8732=EDGE_CURVE('',#6985,#6994,#4067,.T.);
#8733=EDGE_CURVE('',#6994,#6994,#863,.T.);
#8734=EDGE_CURVE('',#6986,#6995,#4068,.T.);
#8735=EDGE_CURVE('',#6995,#6995,#864,.T.);
#8736=EDGE_CURVE('',#6987,#6996,#4069,.T.);
#8737=EDGE_CURVE('',#6996,#6996,#865,.T.);
#8738=EDGE_CURVE('',#6988,#6997,#4070,.T.);
#8739=EDGE_CURVE('',#6997,#6997,#866,.T.);
#8740=EDGE_CURVE('',#6998,#6998,#867,.T.);
#8741=EDGE_CURVE('',#6998,#6989,#4071,.T.);
#8742=EDGE_CURVE('',#6999,#6999,#868,.T.);
#8743=EDGE_CURVE('',#6999,#6990,#4072,.T.);
#8744=EDGE_CURVE('',#7000,#7000,#869,.T.);
#8745=EDGE_CURVE('',#7000,#7001,#4073,.T.);
#8746=EDGE_CURVE('',#7001,#7001,#870,.T.);
#8747=EDGE_CURVE('',#7001,#7002,#4074,.T.);
#8748=EDGE_CURVE('',#7002,#7002,#871,.T.);
#8749=EDGE_CURVE('',#7003,#7003,#872,.T.);
#8750=EDGE_CURVE('',#7003,#7004,#4075,.T.);
#8751=EDGE_CURVE('',#7004,#7004,#873,.T.);
#8752=EDGE_CURVE('',#7005,#7005,#874,.T.);
#8753=EDGE_CURVE('',#7005,#7006,#4076,.T.);
#8754=EDGE_CURVE('',#7006,#7006,#875,.T.);
#8755=EDGE_CURVE('',#7007,#7007,#876,.T.);
#8756=EDGE_CURVE('',#7007,#7008,#4077,.T.);
#8757=EDGE_CURVE('',#7008,#7008,#877,.T.);
#8758=EDGE_CURVE('',#7009,#7009,#878,.T.);
#8759=EDGE_CURVE('',#7009,#7010,#4078,.T.);
#8760=EDGE_CURVE('',#7010,#7010,#879,.T.);
#8761=EDGE_CURVE('',#7011,#7011,#880,.T.);
#8762=EDGE_CURVE('',#7011,#7012,#4079,.T.);
#8763=EDGE_CURVE('',#7012,#7012,#881,.T.);
#8764=EDGE_CURVE('',#7013,#7013,#882,.T.);
#8765=EDGE_CURVE('',#7013,#7014,#4080,.T.);
#8766=EDGE_CURVE('',#7014,#7014,#883,.T.);
#8767=EDGE_CURVE('',#7015,#7015,#884,.T.);
#8768=EDGE_CURVE('',#7015,#7016,#4081,.T.);
#8769=EDGE_CURVE('',#7016,#7016,#885,.T.);
#8770=EDGE_CURVE('',#7017,#7017,#886,.T.);
#8771=EDGE_CURVE('',#7018,#7018,#887,.T.);
#8772=EDGE_CURVE('',#7018,#7017,#4082,.T.);
#8773=EDGE_CURVE('',#7019,#7019,#888,.T.);
#8774=EDGE_CURVE('',#7019,#7020,#4083,.T.);
#8775=EDGE_CURVE('',#7020,#7020,#889,.T.);
#8776=EDGE_CURVE('',#7021,#7021,#890,.T.);
#8777=EDGE_CURVE('',#7021,#7022,#4084,.T.);
#8778=EDGE_CURVE('',#7022,#7022,#891,.T.);
#8779=EDGE_CURVE('',#7023,#7023,#892,.T.);
#8780=EDGE_CURVE('',#7023,#7024,#4085,.T.);
#8781=EDGE_CURVE('',#7024,#7024,#893,.T.);
#8782=EDGE_CURVE('',#7025,#7025,#894,.T.);
#8783=EDGE_CURVE('',#7025,#7026,#4086,.T.);
#8784=EDGE_CURVE('',#7026,#7026,#895,.T.);
#8785=EDGE_CURVE('',#7027,#7027,#896,.T.);
#8786=EDGE_CURVE('',#7027,#7028,#4087,.T.);
#8787=EDGE_CURVE('',#7028,#7028,#897,.T.);
#8788=EDGE_CURVE('',#7029,#7029,#898,.T.);
#8789=EDGE_CURVE('',#7029,#7030,#4088,.T.);
#8790=EDGE_CURVE('',#7030,#7030,#899,.T.);
#8791=EDGE_CURVE('',#7031,#7031,#900,.T.);
#8792=EDGE_CURVE('',#7031,#7032,#4089,.T.);
#8793=EDGE_CURVE('',#7032,#7032,#901,.T.);
#8794=EDGE_CURVE('',#7033,#7033,#902,.T.);
#8795=EDGE_CURVE('',#7033,#7034,#4090,.T.);
#8796=EDGE_CURVE('',#7034,#7034,#903,.T.);
#8797=EDGE_CURVE('',#7035,#7035,#904,.T.);
#8798=EDGE_CURVE('',#7036,#7036,#905,.T.);
#8799=EDGE_CURVE('',#7036,#7035,#4091,.T.);
#8800=EDGE_CURVE('',#7037,#7037,#906,.T.);
#8801=EDGE_CURVE('',#7037,#7038,#4092,.T.);
#8802=EDGE_CURVE('',#7038,#7038,#907,.T.);
#8803=EDGE_CURVE('',#7039,#7040,#908,.T.);
#8804=EDGE_CURVE('',#7040,#7039,#909,.T.);
#8805=EDGE_CURVE('',#7039,#7041,#4093,.T.);
#8806=EDGE_CURVE('',#7041,#7041,#910,.T.);
#8807=EDGE_CURVE('',#7042,#7042,#911,.T.);
#8808=EDGE_CURVE('',#7043,#7043,#912,.T.);
#8809=EDGE_CURVE('',#7043,#7040,#4094,.T.);
#8810=EDGE_CURVE('',#7044,#7044,#913,.T.);
#8811=EDGE_CURVE('',#7044,#7042,#4095,.T.);
#8812=EDGE_CURVE('',#7045,#7045,#914,.T.);
#8813=EDGE_CURVE('',#7045,#7043,#4096,.T.);
#8814=EDGE_CURVE('',#7046,#7046,#915,.T.);
#8815=EDGE_CURVE('',#7046,#7047,#4097,.T.);
#8816=EDGE_CURVE('',#7047,#7048,#916,.T.);
#8817=EDGE_CURVE('',#7048,#7047,#917,.T.);
#8818=EDGE_CURVE('',#7049,#7049,#918,.T.);
#8819=EDGE_CURVE('',#7048,#7050,#4098,.T.);
#8820=EDGE_CURVE('',#7050,#7050,#919,.T.);
#8821=EDGE_CURVE('',#7051,#7051,#920,.T.);
#8822=EDGE_CURVE('',#7051,#7052,#4099,.T.);
#8823=EDGE_CURVE('',#7052,#7053,#921,.T.);
#8824=EDGE_CURVE('',#7053,#7052,#922,.T.);
#8825=EDGE_CURVE('',#7054,#7055,#923,.T.);
#8826=EDGE_CURVE('',#7055,#7054,#924,.T.);
#8827=EDGE_CURVE('',#7055,#7053,#4100,.T.);
#8828=EDGE_CURVE('',#7056,#7056,#925,.T.);
#8829=EDGE_CURVE('',#7054,#7049,#4101,.T.);
#8830=EDGE_CURVE('',#7050,#7056,#4102,.T.);
#8831=EDGE_CURVE('',#7057,#7058,#4103,.T.);
#8832=EDGE_CURVE('',#7057,#7059,#5881,.T.);
#8833=EDGE_CURVE('',#7059,#7060,#926,.T.);
#8834=EDGE_CURVE('',#7060,#7058,#5882,.T.);
#8835=EDGE_CURVE('',#7061,#7062,#4104,.T.);
#8836=EDGE_CURVE('',#7061,#7057,#5883,.T.);
#8837=EDGE_CURVE('',#7058,#7062,#5884,.T.);
#8838=EDGE_CURVE('',#7063,#7064,#4105,.T.);
#8839=EDGE_CURVE('',#7063,#7061,#5885,.T.);
#8840=EDGE_CURVE('',#7062,#7064,#5886,.T.);
#8841=EDGE_CURVE('',#7065,#7066,#4106,.T.);
#8842=EDGE_CURVE('',#7065,#7063,#5887,.T.);
#8843=EDGE_CURVE('',#7064,#7066,#5888,.T.);
#8844=EDGE_CURVE('',#7067,#7068,#4107,.T.);
#8845=EDGE_CURVE('',#7067,#7065,#5889,.T.);
#8846=EDGE_CURVE('',#7066,#7068,#5890,.T.);
#8847=EDGE_CURVE('',#7069,#7070,#4108,.T.);
#8848=EDGE_CURVE('',#7069,#7067,#5891,.T.);
#8849=EDGE_CURVE('',#7068,#7070,#5892,.T.);
#8850=EDGE_CURVE('',#7071,#7072,#4109,.T.);
#8851=EDGE_CURVE('',#7071,#7069,#5893,.T.);
#8852=EDGE_CURVE('',#7070,#7072,#5894,.T.);
#8853=EDGE_CURVE('',#7073,#7074,#4110,.T.);
#8854=EDGE_CURVE('',#7073,#7071,#5895,.T.);
#8855=EDGE_CURVE('',#7072,#7074,#5896,.T.);
#8856=EDGE_CURVE('',#7075,#7076,#4111,.T.);
#8857=EDGE_CURVE('',#7075,#7073,#5897,.T.);
#8858=EDGE_CURVE('',#7074,#7076,#5898,.T.);
#8859=EDGE_CURVE('',#7077,#7078,#4112,.T.);
#8860=EDGE_CURVE('',#7077,#7075,#5899,.T.);
#8861=EDGE_CURVE('',#7076,#7078,#5900,.T.);
#8862=EDGE_CURVE('',#7079,#7080,#4113,.T.);
#8863=EDGE_CURVE('',#7079,#7077,#5901,.T.);
#8864=EDGE_CURVE('',#7078,#7080,#5902,.T.);
#8865=EDGE_CURVE('',#7081,#7082,#4114,.T.);
#8866=EDGE_CURVE('',#7081,#7079,#5903,.T.);
#8867=EDGE_CURVE('',#7080,#7082,#5904,.T.);
#8868=EDGE_CURVE('',#7083,#7084,#4115,.T.);
#8869=EDGE_CURVE('',#7083,#7081,#5905,.T.);
#8870=EDGE_CURVE('',#7082,#7084,#5906,.T.);
#8871=EDGE_CURVE('',#7085,#7086,#4116,.T.);
#8872=EDGE_CURVE('',#7085,#7083,#5907,.T.);
#8873=EDGE_CURVE('',#7084,#7086,#5908,.T.);
#8874=EDGE_CURVE('',#7087,#7088,#4117,.T.);
#8875=EDGE_CURVE('',#7087,#7085,#5909,.T.);
#8876=EDGE_CURVE('',#7086,#7088,#5910,.T.);
#8877=EDGE_CURVE('',#7089,#7090,#4118,.T.);
#8878=EDGE_CURVE('',#7089,#7091,#5911,.T.);
#8879=EDGE_CURVE('',#7092,#7091,#927,.T.);
#8880=EDGE_CURVE('',#7090,#7092,#5912,.T.);
#8881=EDGE_CURVE('',#7093,#7094,#4119,.T.);
#8882=EDGE_CURVE('',#7093,#7089,#5913,.T.);
#8883=EDGE_CURVE('',#7094,#7090,#5914,.T.);
#8884=EDGE_CURVE('',#7095,#7096,#4120,.T.);
#8885=EDGE_CURVE('',#7095,#7093,#5915,.T.);
#8886=EDGE_CURVE('',#7096,#7094,#5916,.T.);
#8887=EDGE_CURVE('',#7097,#7098,#4121,.T.);
#8888=EDGE_CURVE('',#7097,#7095,#5917,.T.);
#8889=EDGE_CURVE('',#7098,#7096,#5918,.T.);
#8890=EDGE_CURVE('',#7099,#7100,#4122,.T.);
#8891=EDGE_CURVE('',#7099,#7097,#5919,.T.);
#8892=EDGE_CURVE('',#7100,#7098,#5920,.T.);
#8893=EDGE_CURVE('',#7101,#7102,#4123,.T.);
#8894=EDGE_CURVE('',#7101,#7099,#5921,.T.);
#8895=EDGE_CURVE('',#7102,#7100,#5922,.T.);
#8896=EDGE_CURVE('',#7103,#7104,#4124,.T.);
#8897=EDGE_CURVE('',#7103,#7101,#5923,.T.);
#8898=EDGE_CURVE('',#7104,#7102,#5924,.T.);
#8899=EDGE_CURVE('',#7105,#7106,#4125,.T.);
#8900=EDGE_CURVE('',#7105,#7103,#5925,.T.);
#8901=EDGE_CURVE('',#7106,#7104,#5926,.T.);
#8902=EDGE_CURVE('',#7107,#7108,#4126,.T.);
#8903=EDGE_CURVE('',#7107,#7105,#5927,.T.);
#8904=EDGE_CURVE('',#7108,#7106,#5928,.T.);
#8905=EDGE_CURVE('',#7109,#7110,#4127,.T.);
#8906=EDGE_CURVE('',#7109,#7107,#5929,.T.);
#8907=EDGE_CURVE('',#7110,#7108,#5930,.T.);
#8908=EDGE_CURVE('',#7111,#7112,#4128,.T.);
#8909=EDGE_CURVE('',#7111,#7109,#5931,.T.);
#8910=EDGE_CURVE('',#7112,#7110,#5932,.T.);
#8911=EDGE_CURVE('',#7113,#7114,#4129,.T.);
#8912=EDGE_CURVE('',#7113,#7111,#5933,.T.);
#8913=EDGE_CURVE('',#7114,#7112,#5934,.T.);
#8914=EDGE_CURVE('',#7115,#7116,#4130,.T.);
#8915=EDGE_CURVE('',#7115,#7113,#5935,.T.);
#8916=EDGE_CURVE('',#7116,#7114,#5936,.T.);
#8917=EDGE_CURVE('',#7117,#7118,#4131,.T.);
#8918=EDGE_CURVE('',#7117,#7115,#5937,.T.);
#8919=EDGE_CURVE('',#7118,#7116,#5938,.T.);
#8920=EDGE_CURVE('',#7119,#7120,#4132,.T.);
#8921=EDGE_CURVE('',#7119,#7117,#5939,.T.);
#8922=EDGE_CURVE('',#7120,#7118,#5940,.T.);
#8923=EDGE_CURVE('',#7121,#7122,#4133,.T.);
#8924=EDGE_CURVE('',#7121,#7123,#5941,.T.);
#8925=EDGE_CURVE('',#7123,#7124,#928,.F.);
#8926=EDGE_CURVE('',#7124,#7122,#5942,.T.);
#8927=EDGE_CURVE('',#7125,#7126,#4134,.T.);
#8928=EDGE_CURVE('',#7125,#7121,#5943,.T.);
#8929=EDGE_CURVE('',#7122,#7126,#5944,.T.);
#8930=EDGE_CURVE('',#7127,#7128,#4135,.T.);
#8931=EDGE_CURVE('',#7127,#7125,#5945,.T.);
#8932=EDGE_CURVE('',#7126,#7128,#5946,.T.);
#8933=EDGE_CURVE('',#7129,#7130,#4136,.T.);
#8934=EDGE_CURVE('',#7129,#7127,#5947,.T.);
#8935=EDGE_CURVE('',#7128,#7130,#5948,.T.);
#8936=EDGE_CURVE('',#7131,#7132,#4137,.T.);
#8937=EDGE_CURVE('',#7131,#7129,#5949,.T.);
#8938=EDGE_CURVE('',#7130,#7132,#5950,.T.);
#8939=EDGE_CURVE('',#7133,#7134,#4138,.T.);
#8940=EDGE_CURVE('',#7133,#7131,#5951,.T.);
#8941=EDGE_CURVE('',#7132,#7134,#5952,.T.);
#8942=EDGE_CURVE('',#7135,#7136,#4139,.T.);
#8943=EDGE_CURVE('',#7135,#7133,#5953,.T.);
#8944=EDGE_CURVE('',#7134,#7136,#5954,.T.);
#8945=EDGE_CURVE('',#7137,#7138,#4140,.T.);
#8946=EDGE_CURVE('',#7137,#7135,#5955,.T.);
#8947=EDGE_CURVE('',#7136,#7138,#5956,.T.);
#8948=EDGE_CURVE('',#7139,#7140,#4141,.T.);
#8949=EDGE_CURVE('',#7139,#7137,#5957,.T.);
#8950=EDGE_CURVE('',#7138,#7140,#5958,.T.);
#8951=EDGE_CURVE('',#7141,#7142,#4142,.T.);
#8952=EDGE_CURVE('',#7141,#7139,#5959,.T.);
#8953=EDGE_CURVE('',#7140,#7142,#5960,.T.);
#8954=EDGE_CURVE('',#7143,#7144,#4143,.T.);
#8955=EDGE_CURVE('',#7143,#7141,#5961,.T.);
#8956=EDGE_CURVE('',#7142,#7144,#5962,.T.);
#8957=EDGE_CURVE('',#7145,#7146,#4144,.T.);
#8958=EDGE_CURVE('',#7145,#7143,#5963,.T.);
#8959=EDGE_CURVE('',#7144,#7146,#5964,.T.);
#8960=EDGE_CURVE('',#7147,#7148,#4145,.T.);
#8961=EDGE_CURVE('',#7147,#7145,#5965,.T.);
#8962=EDGE_CURVE('',#7146,#7148,#5966,.T.);
#8963=EDGE_CURVE('',#7149,#7150,#4146,.T.);
#8964=EDGE_CURVE('',#7149,#7147,#5967,.T.);
#8965=EDGE_CURVE('',#7148,#7150,#5968,.T.);
#8966=EDGE_CURVE('',#7151,#7152,#4147,.T.);
#8967=EDGE_CURVE('',#7151,#7149,#5969,.T.);
#8968=EDGE_CURVE('',#7150,#7152,#5970,.T.);
#8969=EDGE_CURVE('',#7153,#7154,#4148,.T.);
#8970=EDGE_CURVE('',#7153,#7155,#5971,.T.);
#8971=EDGE_CURVE('',#7156,#7155,#929,.T.);
#8972=EDGE_CURVE('',#7154,#7156,#5972,.T.);
#8973=EDGE_CURVE('',#7157,#7158,#4149,.T.);
#8974=EDGE_CURVE('',#7157,#7153,#5973,.T.);
#8975=EDGE_CURVE('',#7158,#7154,#5974,.T.);
#8976=EDGE_CURVE('',#7159,#7160,#4150,.T.);
#8977=EDGE_CURVE('',#7159,#7157,#5975,.T.);
#8978=EDGE_CURVE('',#7160,#7158,#5976,.T.);
#8979=EDGE_CURVE('',#7161,#7162,#4151,.T.);
#8980=EDGE_CURVE('',#7161,#7159,#5977,.T.);
#8981=EDGE_CURVE('',#7162,#7160,#5978,.T.);
#8982=EDGE_CURVE('',#7163,#7164,#4152,.T.);
#8983=EDGE_CURVE('',#7163,#7161,#5979,.T.);
#8984=EDGE_CURVE('',#7164,#7162,#5980,.T.);
#8985=EDGE_CURVE('',#7165,#7166,#4153,.T.);
#8986=EDGE_CURVE('',#7165,#7163,#5981,.T.);
#8987=EDGE_CURVE('',#7166,#7164,#5982,.T.);
#8988=EDGE_CURVE('',#7167,#7168,#4154,.T.);
#8989=EDGE_CURVE('',#7167,#7165,#5983,.T.);
#8990=EDGE_CURVE('',#7168,#7166,#5984,.T.);
#8991=EDGE_CURVE('',#7169,#7170,#4155,.T.);
#8992=EDGE_CURVE('',#7169,#7167,#5985,.T.);
#8993=EDGE_CURVE('',#7170,#7168,#5986,.T.);
#8994=EDGE_CURVE('',#7171,#7172,#4156,.T.);
#8995=EDGE_CURVE('',#7171,#7169,#5987,.T.);
#8996=EDGE_CURVE('',#7172,#7170,#5988,.T.);
#8997=EDGE_CURVE('',#7173,#7174,#4157,.T.);
#8998=EDGE_CURVE('',#7173,#7171,#5989,.T.);
#8999=EDGE_CURVE('',#7174,#7172,#5990,.T.);
#9000=EDGE_CURVE('',#7175,#7176,#4158,.T.);
#9001=EDGE_CURVE('',#7175,#7173,#5991,.T.);
#9002=EDGE_CURVE('',#7176,#7174,#5992,.T.);
#9003=EDGE_CURVE('',#7177,#7178,#4159,.T.);
#9004=EDGE_CURVE('',#7177,#7175,#5993,.T.);
#9005=EDGE_CURVE('',#7178,#7176,#5994,.T.);
#9006=EDGE_CURVE('',#7179,#7180,#4160,.T.);
#9007=EDGE_CURVE('',#7179,#7177,#5995,.T.);
#9008=EDGE_CURVE('',#7180,#7178,#5996,.T.);
#9009=EDGE_CURVE('',#7181,#7182,#4161,.T.);
#9010=EDGE_CURVE('',#7181,#7179,#5997,.T.);
#9011=EDGE_CURVE('',#7182,#7180,#5998,.T.);
#9012=EDGE_CURVE('',#7183,#7184,#4162,.T.);
#9013=EDGE_CURVE('',#7183,#7181,#5999,.T.);
#9014=EDGE_CURVE('',#7184,#7182,#6000,.T.);
#9015=EDGE_CURVE('',#7155,#7185,#6001,.T.);
#9016=EDGE_CURVE('',#7186,#7185,#930,.F.);
#9017=EDGE_CURVE('',#7187,#7186,#931,.F.);
#9018=EDGE_CURVE('',#7187,#7156,#6002,.T.);
#9019=EDGE_CURVE('',#7152,#7187,#6003,.T.);
#9020=EDGE_CURVE('',#7188,#7124,#6004,.T.);
#9021=EDGE_CURVE('',#7188,#7184,#6005,.T.);
#9022=EDGE_CURVE('',#7189,#7188,#932,.T.);
#9023=EDGE_CURVE('',#7189,#7183,#6006,.T.);
#9024=EDGE_CURVE('',#7123,#7189,#6007,.T.);
#9025=EDGE_CURVE('',#7185,#7151,#6008,.T.);
#9026=EDGE_CURVE('',#7185,#7187,#933,.F.);
#9027=EDGE_CURVE('',#7190,#7092,#6009,.T.);
#9028=EDGE_CURVE('',#7088,#7190,#6010,.T.);
#9029=EDGE_CURVE('',#7191,#7060,#6011,.T.);
#9030=EDGE_CURVE('',#7191,#7120,#6012,.T.);
#9031=EDGE_CURVE('',#7060,#7192,#934,.T.);
#9032=EDGE_CURVE('',#7192,#7059,#935,.T.);
#9033=EDGE_CURVE('',#7059,#7193,#6013,.T.);
#9034=EDGE_CURVE('',#7193,#7191,#936,.T.);
#9035=EDGE_CURVE('',#7193,#7119,#6014,.T.);
#9036=EDGE_CURVE('',#7091,#7194,#6015,.T.);
#9037=EDGE_CURVE('',#7194,#7087,#6016,.T.);
#9038=EDGE_CURVE('',#7195,#7195,#937,.T.);
#9039=EDGE_CURVE('',#7192,#7195,#4163,.T.);
#9040=EDGE_CURVE('',#7194,#7190,#938,.T.);
#9041=EDGE_CURVE('',#7196,#7196,#939,.T.);
#9042=EDGE_CURVE('',#7197,#7197,#940,.T.);
#9043=EDGE_CURVE('',#7197,#7196,#4164,.T.);
#9044=EDGE_CURVE('',#7198,#7198,#941,.T.);
#9045=EDGE_CURVE('',#7198,#7186,#4165,.T.);
#9046=EDGE_CURVE('',#7199,#7199,#942,.T.);
#9047=EDGE_CURVE('',#7199,#7200,#4166,.T.);
#9048=EDGE_CURVE('',#7200,#7201,#6017,.T.);
#9049=EDGE_CURVE('',#7201,#7202,#943,.T.);
#9050=EDGE_CURVE('',#7202,#7203,#6018,.T.);
#9051=EDGE_CURVE('',#7203,#7204,#944,.T.);
#9052=EDGE_CURVE('',#7204,#7205,#6019,.T.);
#9053=EDGE_CURVE('',#7205,#7206,#945,.T.);
#9054=EDGE_CURVE('',#7206,#7207,#6020,.T.);
#9055=EDGE_CURVE('',#7207,#7208,#946,.T.);
#9056=EDGE_CURVE('',#7208,#7209,#6021,.T.);
#9057=EDGE_CURVE('',#7209,#7210,#947,.T.);
#9058=EDGE_CURVE('',#7210,#7211,#6022,.T.);
#9059=EDGE_CURVE('',#7211,#7212,#948,.T.);
#9060=EDGE_CURVE('',#7212,#7200,#6023,.T.);
#9061=EDGE_CURVE('',#7208,#7213,#6024,.T.);
#9062=EDGE_CURVE('',#7213,#7214,#6025,.F.);
#9063=EDGE_CURVE('',#7214,#7215,#6026,.T.);
#9064=EDGE_CURVE('',#7215,#7216,#6027,.F.);
#9065=EDGE_CURVE('',#7216,#7209,#6028,.T.);
#9066=EDGE_CURVE('',#7206,#7217,#6029,.T.);
#9067=EDGE_CURVE('',#7217,#7218,#6030,.F.);
#9068=EDGE_CURVE('',#7218,#7219,#6031,.T.);
#9069=EDGE_CURVE('',#7219,#7213,#6032,.F.);
#9070=EDGE_CURVE('',#7213,#7207,#6033,.T.);
#9071=EDGE_CURVE('',#7217,#7205,#6034,.T.);
#9072=EDGE_CURVE('',#7220,#7203,#6035,.T.);
#9073=EDGE_CURVE('',#7204,#7220,#6036,.T.);
#9074=EDGE_CURVE('',#7221,#7201,#6037,.T.);
#9075=EDGE_CURVE('',#7202,#7221,#6038,.T.);
#9076=EDGE_CURVE('',#7222,#7211,#6039,.T.);
#9077=EDGE_CURVE('',#7212,#7222,#6040,.T.);
#9078=EDGE_CURVE('',#7210,#7216,#6041,.T.);
#9079=EDGE_CURVE('',#7220,#7223,#6042,.F.);
#9080=EDGE_CURVE('',#7223,#7224,#6043,.T.);
#9081=EDGE_CURVE('',#7224,#7217,#6044,.F.);
#9082=EDGE_CURVE('',#7225,#7225,#949,.T.);
#9083=EDGE_CURVE('',#7218,#7224,#4167,.T.);
#9084=EDGE_CURVE('',#7226,#7220,#6045,.F.);
#9085=EDGE_CURVE('',#7223,#7226,#4168,.T.);
#9086=EDGE_CURVE('',#7214,#7219,#4169,.T.);
#9087=EDGE_CURVE('',#7221,#7227,#6046,.F.);
#9088=EDGE_CURVE('',#7228,#7221,#6047,.F.);
#9089=EDGE_CURVE('',#7227,#7228,#4170,.T.);
#9090=EDGE_CURVE('',#7229,#7215,#4171,.T.);
#9091=EDGE_CURVE('',#7216,#7229,#6048,.F.);
#9092=EDGE_CURVE('',#7222,#7230,#6049,.F.);
#9093=EDGE_CURVE('',#7231,#7222,#6050,.F.);
#9094=EDGE_CURVE('',#7230,#7231,#4172,.T.);
#9095=EDGE_CURVE('',#7229,#7231,#6051,.T.);
#9096=EDGE_CURVE('',#7232,#7233,#1765,.T.);
#9097=EDGE_CURVE('',#7233,#7230,#4173,.T.);
#9098=EDGE_CURVE('',#7231,#7232,#4174,.T.);
#9099=EDGE_CURVE('',#7230,#7228,#6052,.T.);
#9100=EDGE_CURVE('',#7234,#7235,#1766,.T.);
#9101=EDGE_CURVE('',#7235,#7229,#4175,.T.);
#9102=EDGE_CURVE('',#7215,#7234,#4176,.T.);
#9103=EDGE_CURVE('',#7236,#7237,#1767,.T.);
#9104=EDGE_CURVE('',#7237,#7227,#4177,.T.);
#9105=EDGE_CURVE('',#7228,#7236,#4178,.T.);
#9106=EDGE_CURVE('',#7227,#7226,#6053,.T.);
#9107=EDGE_CURVE('',#7238,#7239,#1768,.T.);
#9108=EDGE_CURVE('',#7239,#7214,#4179,.T.);
#9109=EDGE_CURVE('',#7219,#7238,#4180,.T.);
#9110=EDGE_CURVE('',#7240,#7241,#1769,.T.);
#9111=EDGE_CURVE('',#7241,#7223,#4181,.T.);
#9112=EDGE_CURVE('',#7226,#7240,#4182,.T.);
#9113=EDGE_CURVE('',#7242,#7243,#1770,.T.);
#9114=EDGE_CURVE('',#7243,#7218,#4183,.T.);
#9115=EDGE_CURVE('',#7224,#7242,#4184,.T.);
#9116=EDGE_CURVE('',#7239,#7234,#1771,.T.);
#9117=EDGE_CURVE('',#7243,#7238,#1772,.T.);
#9118=EDGE_CURVE('',#7241,#7242,#1773,.T.);
#9119=EDGE_CURVE('',#7244,#7244,#950,.T.);
#9120=EDGE_CURVE('',#7244,#7245,#4185,.T.);
#9121=EDGE_CURVE('',#7233,#7245,#1774,.T.);
#9122=EDGE_CURVE('',#7235,#7232,#1775,.T.);
#9123=EDGE_CURVE('',#7237,#7240,#1776,.T.);
#9124=EDGE_CURVE('',#7245,#7236,#1777,.T.);
#9125=EDGE_CURVE('',#7246,#7246,#951,.T.);
#9126=EDGE_CURVE('',#7246,#7247,#4186,.T.);
#9127=EDGE_CURVE('',#7247,#7247,#952,.T.);
#9128=EDGE_CURVE('',#7247,#7248,#4187,.T.);
#9129=EDGE_CURVE('',#7248,#7248,#953,.T.);
#9130=EDGE_CURVE('',#7248,#7225,#4188,.T.);
#9131=EDGE_CURVE('',#7249,#7249,#954,.T.);
#9132=EDGE_CURVE('',#7249,#7250,#4189,.T.);
#9133=EDGE_CURVE('',#7250,#7251,#955,.T.);
#9134=EDGE_CURVE('',#7251,#7250,#956,.T.);
#9135=EDGE_CURVE('',#7252,#7252,#957,.T.);
#9136=EDGE_CURVE('',#7251,#7253,#4190,.T.);
#9137=EDGE_CURVE('',#7253,#7254,#4191,.T.);
#9138=EDGE_CURVE('',#7254,#7255,#4192,.T.);
#9139=EDGE_CURVE('',#7255,#7255,#958,.T.);
#9140=EDGE_CURVE('',#7256,#7254,#244,.T.);
#9141=EDGE_CURVE('',#7254,#7256,#245,.T.);
#9142=EDGE_CURVE('',#7257,#7253,#246,.T.);
#9143=EDGE_CURVE('',#7253,#7257,#247,.T.);
#9144=EDGE_CURVE('',#7258,#7258,#959,.T.);
#9145=EDGE_CURVE('',#7258,#7259,#4193,.T.);
#9146=EDGE_CURVE('',#7259,#7259,#960,.T.);
#9147=EDGE_CURVE('',#7260,#7260,#961,.T.);
#9148=EDGE_CURVE('',#7261,#7261,#962,.T.);
#9149=EDGE_CURVE('',#7261,#7259,#4194,.T.);
#9150=EDGE_CURVE('',#7262,#7262,#963,.T.);
#9151=EDGE_CURVE('',#7262,#7260,#964,.T.);
#9152=EDGE_CURVE('',#7262,#7263,#4195,.T.);
#9153=EDGE_CURVE('',#7264,#7263,#965,.T.);
#9154=EDGE_CURVE('',#7263,#7264,#966,.T.);
#9155=EDGE_CURVE('',#7264,#7265,#967,.T.);
#9156=EDGE_CURVE('',#7265,#7265,#968,.T.);
#9157=EDGE_CURVE('',#7266,#7266,#969,.T.);
#9158=EDGE_CURVE('',#7267,#7267,#970,.T.);
#9159=EDGE_CURVE('',#7267,#7268,#971,.T.);
#9160=EDGE_CURVE('',#7268,#7269,#972,.T.);
#9161=EDGE_CURVE('',#7269,#7268,#973,.T.);
#9162=EDGE_CURVE('',#7269,#7270,#4196,.T.);
#9163=EDGE_CURVE('',#7270,#7270,#974,.T.);
#9164=EDGE_CURVE('',#7271,#7271,#975,.T.);
#9165=EDGE_CURVE('',#7270,#7272,#976,.T.);
#9166=EDGE_CURVE('',#7272,#7272,#977,.T.);
#9167=EDGE_CURVE('',#7273,#7273,#978,.T.);
#9168=EDGE_CURVE('',#7274,#7275,#979,.T.);
#9169=EDGE_CURVE('',#7275,#7276,#4197,.T.);
#9170=EDGE_CURVE('',#7276,#7277,#980,.T.);
#9171=EDGE_CURVE('',#7277,#7274,#4198,.T.);
#9172=EDGE_CURVE('',#7278,#7279,#981,.T.);
#9173=EDGE_CURVE('',#7279,#7277,#982,.T.);
#9174=EDGE_CURVE('',#7276,#7278,#983,.T.);
#9175=EDGE_CURVE('',#7280,#7281,#984,.T.);
#9176=EDGE_CURVE('',#7281,#7279,#4199,.T.);
#9177=EDGE_CURVE('',#7278,#7280,#4200,.T.);
#9178=EDGE_CURVE('',#7282,#7283,#985,.T.);
#9179=EDGE_CURVE('',#7283,#7281,#986,.T.);
#9180=EDGE_CURVE('',#7280,#7282,#987,.T.);
#9181=EDGE_CURVE('',#7284,#7285,#988,.T.);
#9182=EDGE_CURVE('',#7285,#7283,#4201,.T.);
#9183=EDGE_CURVE('',#7282,#7284,#4202,.T.);
#9184=EDGE_CURVE('',#7286,#7287,#989,.T.);
#9185=EDGE_CURVE('',#7287,#7285,#990,.T.);
#9186=EDGE_CURVE('',#7284,#7286,#991,.T.);
#9187=EDGE_CURVE('',#7288,#7289,#992,.T.);
#9188=EDGE_CURVE('',#7289,#7287,#4203,.T.);
#9189=EDGE_CURVE('',#7286,#7288,#4204,.T.);
#9190=EDGE_CURVE('',#7274,#7289,#993,.T.);
#9191=EDGE_CURVE('',#7288,#7275,#994,.T.);
#9192=EDGE_CURVE('',#7290,#7280,#4205,.T.);
#9193=EDGE_CURVE('',#7291,#7290,#995,.T.);
#9194=EDGE_CURVE('',#7291,#7282,#4206,.T.);
#9195=EDGE_CURVE('',#7292,#7278,#4207,.T.);
#9196=EDGE_CURVE('',#7290,#7292,#4208,.T.);
#9197=EDGE_CURVE('',#7293,#7276,#4209,.T.);
#9198=EDGE_CURVE('',#7292,#7293,#996,.T.);
#9199=EDGE_CURVE('',#7294,#7275,#4210,.T.);
#9200=EDGE_CURVE('',#7293,#7294,#4211,.T.);
#9201=EDGE_CURVE('',#7295,#7295,#997,.T.);
#9202=EDGE_CURVE('',#7296,#7296,#998,.T.);
#9203=EDGE_CURVE('',#7297,#7297,#999,.T.);
#9204=EDGE_CURVE('',#7298,#7298,#1000,.T.);
#9205=EDGE_CURVE('',#7294,#7299,#1001,.T.);
#9206=EDGE_CURVE('',#7299,#7300,#4212,.T.);
#9207=EDGE_CURVE('',#7300,#7293,#1002,.T.);
#9208=EDGE_CURVE('',#7301,#7292,#1003,.T.);
#9209=EDGE_CURVE('',#7300,#7301,#1004,.T.);
#9210=EDGE_CURVE('',#7302,#7290,#1005,.T.);
#9211=EDGE_CURVE('',#7301,#7302,#4213,.T.);
#9212=EDGE_CURVE('',#7303,#7291,#1006,.T.);
#9213=EDGE_CURVE('',#7302,#7303,#1007,.T.);
#9214=EDGE_CURVE('',#7304,#7305,#1008,.T.);
#9215=EDGE_CURVE('',#7305,#7291,#4214,.T.);
#9216=EDGE_CURVE('',#7303,#7304,#4215,.T.);
#9217=EDGE_CURVE('',#7306,#7307,#1009,.T.);
#9218=EDGE_CURVE('',#7307,#7305,#1010,.T.);
#9219=EDGE_CURVE('',#7304,#7306,#1011,.T.);
#9220=EDGE_CURVE('',#7308,#7309,#1012,.T.);
#9221=EDGE_CURVE('',#7309,#7307,#4216,.T.);
#9222=EDGE_CURVE('',#7306,#7308,#4217,.T.);
#9223=EDGE_CURVE('',#7294,#7309,#1013,.T.);
#9224=EDGE_CURVE('',#7308,#7299,#1014,.T.);
#9225=EDGE_CURVE('',#7305,#7284,#4218,.T.);
#9226=EDGE_CURVE('',#7307,#7286,#4219,.T.);
#9227=EDGE_CURVE('',#7309,#7288,#4220,.T.);
#9228=EDGE_CURVE('',#7310,#7310,#1015,.T.);
#9229=EDGE_CURVE('',#7311,#7311,#1016,.T.);
#9230=EDGE_CURVE('',#7312,#7313,#1017,.T.);
#9231=EDGE_CURVE('',#7313,#7314,#4221,.T.);
#9232=EDGE_CURVE('',#7314,#7315,#1018,.T.);
#9233=EDGE_CURVE('',#7315,#7312,#4222,.T.);
#9234=EDGE_CURVE('',#7316,#7317,#1019,.T.);
#9235=EDGE_CURVE('',#7317,#7315,#1020,.T.);
#9236=EDGE_CURVE('',#7314,#7316,#1021,.T.);
#9237=EDGE_CURVE('',#7318,#7319,#1022,.T.);
#9238=EDGE_CURVE('',#7319,#7317,#4223,.T.);
#9239=EDGE_CURVE('',#7316,#7318,#4224,.T.);
#9240=EDGE_CURVE('',#7320,#7321,#1023,.T.);
#9241=EDGE_CURVE('',#7321,#7319,#1024,.T.);
#9242=EDGE_CURVE('',#7318,#7320,#1025,.T.);
#9243=EDGE_CURVE('',#7322,#7323,#1026,.T.);
#9244=EDGE_CURVE('',#7323,#7321,#4225,.T.);
#9245=EDGE_CURVE('',#7320,#7322,#4226,.T.);
#9246=EDGE_CURVE('',#7324,#7325,#1027,.T.);
#9247=EDGE_CURVE('',#7325,#7323,#1028,.T.);
#9248=EDGE_CURVE('',#7322,#7324,#1029,.T.);
#9249=EDGE_CURVE('',#7326,#7327,#1030,.T.);
#9250=EDGE_CURVE('',#7327,#7325,#4227,.T.);
#9251=EDGE_CURVE('',#7324,#7326,#4228,.T.);
#9252=EDGE_CURVE('',#7312,#7327,#1031,.T.);
#9253=EDGE_CURVE('',#7326,#7313,#1032,.T.);
#9254=EDGE_CURVE('',#7328,#7318,#4229,.T.);
#9255=EDGE_CURVE('',#7329,#7328,#1033,.T.);
#9256=EDGE_CURVE('',#7329,#7320,#4230,.T.);
#9257=EDGE_CURVE('',#7330,#7316,#4231,.T.);
#9258=EDGE_CURVE('',#7328,#7330,#4232,.T.);
#9259=EDGE_CURVE('',#7331,#7314,#4233,.T.);
#9260=EDGE_CURVE('',#7330,#7331,#1034,.T.);
#9261=EDGE_CURVE('',#7332,#7313,#4234,.T.);
#9262=EDGE_CURVE('',#7331,#7332,#4235,.T.);
#9263=EDGE_CURVE('',#7333,#7333,#1035,.T.);
#9264=EDGE_CURVE('',#7334,#7334,#1036,.T.);
#9265=EDGE_CURVE('',#7335,#7335,#1037,.T.);
#9266=EDGE_CURVE('',#7336,#7336,#1038,.T.);
#9267=EDGE_CURVE('',#7332,#7337,#1039,.T.);
#9268=EDGE_CURVE('',#7337,#7338,#4236,.T.);
#9269=EDGE_CURVE('',#7338,#7331,#1040,.T.);
#9270=EDGE_CURVE('',#7339,#7330,#1041,.T.);
#9271=EDGE_CURVE('',#7338,#7339,#1042,.T.);
#9272=EDGE_CURVE('',#7340,#7328,#1043,.T.);
#9273=EDGE_CURVE('',#7339,#7340,#4237,.T.);
#9274=EDGE_CURVE('',#7341,#7329,#1044,.T.);
#9275=EDGE_CURVE('',#7340,#7341,#1045,.T.);
#9276=EDGE_CURVE('',#7342,#7343,#1046,.T.);
#9277=EDGE_CURVE('',#7343,#7329,#4238,.T.);
#9278=EDGE_CURVE('',#7341,#7342,#4239,.T.);
#9279=EDGE_CURVE('',#7344,#7345,#1047,.T.);
#9280=EDGE_CURVE('',#7345,#7343,#1048,.T.);
#9281=EDGE_CURVE('',#7342,#7344,#1049,.T.);
#9282=EDGE_CURVE('',#7346,#7347,#1050,.T.);
#9283=EDGE_CURVE('',#7347,#7345,#4240,.T.);
#9284=EDGE_CURVE('',#7344,#7346,#4241,.T.);
#9285=EDGE_CURVE('',#7332,#7347,#1051,.T.);
#9286=EDGE_CURVE('',#7346,#7337,#1052,.T.);
#9287=EDGE_CURVE('',#7343,#7322,#4242,.T.);
#9288=EDGE_CURVE('',#7345,#7324,#4243,.T.);
#9289=EDGE_CURVE('',#7347,#7326,#4244,.T.);
#9290=EDGE_CURVE('',#7348,#7348,#1053,.T.);
#9291=EDGE_CURVE('',#7349,#7349,#1054,.T.);
#9292=EDGE_CURVE('',#7256,#7350,#248,.T.);
#9293=EDGE_CURVE('',#7350,#7254,#249,.T.);
#9294=EDGE_CURVE('',#7254,#7256,#250,.T.);
#9295=EDGE_CURVE('',#7257,#7351,#251,.T.);
#9296=EDGE_CURVE('',#7351,#7253,#252,.T.);
#9297=EDGE_CURVE('',#7253,#7257,#253,.T.);
#9298=EDGE_CURVE('',#7336,#7349,#4245,.T.);
#9299=EDGE_CURVE('',#7298,#7311,#4246,.T.);
#9300=EDGE_CURVE('',#7297,#7310,#4247,.T.);
#9301=EDGE_CURVE('',#7335,#7348,#4248,.T.);
#9302=EDGE_CURVE('',#7296,#7351,#4249,.T.);
#9303=EDGE_CURVE('',#7334,#7350,#4250,.T.);
#9304=EDGE_CURVE('',#7273,#7252,#4251,.T.);
#9305=EDGE_CURVE('',#7352,#7352,#1055,.T.);
#9306=EDGE_CURVE('',#7266,#7352,#4252,.T.);
#9307=EDGE_CURVE('',#7353,#7353,#1056,.T.);
#9308=EDGE_CURVE('',#7333,#7353,#4253,.T.);
#9309=EDGE_CURVE('',#7295,#7271,#4254,.T.);
#9310=EDGE_CURVE('',#7354,#7355,#4255,.T.);
#9311=EDGE_CURVE('',#7354,#7356,#6054,.T.);
#9312=EDGE_CURVE('',#7356,#7357,#1057,.F.);
#9313=EDGE_CURVE('',#7357,#7355,#6055,.T.);
#9314=EDGE_CURVE('',#7358,#7359,#4256,.T.);
#9315=EDGE_CURVE('',#7358,#7354,#6056,.T.);
#9316=EDGE_CURVE('',#7355,#7359,#6057,.T.);
#9317=EDGE_CURVE('',#7360,#7361,#4257,.T.);
#9318=EDGE_CURVE('',#7360,#7358,#6058,.T.);
#9319=EDGE_CURVE('',#7359,#7361,#6059,.T.);
#9320=EDGE_CURVE('',#7362,#7363,#4258,.T.);
#9321=EDGE_CURVE('',#7362,#7360,#6060,.T.);
#9322=EDGE_CURVE('',#7361,#7363,#6061,.T.);
#9323=EDGE_CURVE('',#7364,#7365,#4259,.T.);
#9324=EDGE_CURVE('',#7364,#7362,#6062,.T.);
#9325=EDGE_CURVE('',#7363,#7365,#6063,.T.);
#9326=EDGE_CURVE('',#7366,#7367,#4260,.T.);
#9327=EDGE_CURVE('',#7366,#7364,#6064,.T.);
#9328=EDGE_CURVE('',#7365,#7367,#6065,.T.);
#9329=EDGE_CURVE('',#7368,#7369,#4261,.T.);
#9330=EDGE_CURVE('',#7368,#7370,#6066,.T.);
#9331=EDGE_CURVE('',#7369,#7370,#1058,.T.);
#9332=EDGE_CURVE('',#7371,#7372,#4262,.T.);
#9333=EDGE_CURVE('',#7371,#7368,#6067,.T.);
#9334=EDGE_CURVE('',#7373,#7369,#1059,.T.);
#9335=EDGE_CURVE('',#7372,#7373,#6068,.T.);
#9336=EDGE_CURVE('',#7374,#7375,#4263,.T.);
#9337=EDGE_CURVE('',#7374,#7371,#6069,.T.);
#9338=EDGE_CURVE('',#7375,#7372,#6070,.T.);
#9339=EDGE_CURVE('',#7376,#7377,#4264,.T.);
#9340=EDGE_CURVE('',#7376,#7374,#6071,.T.);
#9341=EDGE_CURVE('',#7377,#7375,#6072,.T.);
#9342=EDGE_CURVE('',#7378,#7379,#4265,.T.);
#9343=EDGE_CURVE('',#7378,#7376,#6073,.T.);
#9344=EDGE_CURVE('',#7379,#7377,#6074,.T.);
#9345=EDGE_CURVE('',#7380,#7381,#4266,.T.);
#9346=EDGE_CURVE('',#7380,#7378,#6075,.T.);
#9347=EDGE_CURVE('',#7381,#7379,#6076,.T.);
#9348=EDGE_CURVE('',#7382,#7382,#1060,.T.);
#9349=EDGE_CURVE('',#7382,#7383,#4267,.T.);
#9350=EDGE_CURVE('',#7383,#7384,#1061,.T.);
#9351=EDGE_CURVE('',#7384,#7383,#1062,.T.);
#9352=EDGE_CURVE('',#7384,#7385,#4268,.T.);
#9353=EDGE_CURVE('',#7386,#7385,#1063,.T.);
#9354=EDGE_CURVE('',#7385,#7386,#1064,.T.);
#9355=EDGE_CURVE('',#7356,#7387,#6077,.T.);
#9356=EDGE_CURVE('',#7387,#7388,#1065,.T.);
#9357=EDGE_CURVE('',#7388,#7357,#6078,.T.);
#9358=EDGE_CURVE('',#7386,#7389,#4269,.T.);
#9359=EDGE_CURVE('',#7389,#7390,#1066,.T.);
#9360=EDGE_CURVE('',#7390,#7389,#1067,.T.);
#9361=EDGE_CURVE('',#7390,#7391,#4270,.T.);
#9362=EDGE_CURVE('',#7392,#7391,#1068,.T.);
#9363=EDGE_CURVE('',#7391,#7392,#1069,.T.);
#9364=EDGE_CURVE('',#7392,#7393,#4271,.T.);
#9365=EDGE_CURVE('',#7393,#7393,#1070,.T.);
#9366=EDGE_CURVE('',#7394,#7395,#4272,.T.);
#9367=EDGE_CURVE('',#7396,#7394,#4273,.T.);
#9368=EDGE_CURVE('',#7397,#7396,#4274,.T.);
#9369=EDGE_CURVE('',#7398,#7397,#4275,.T.);
#9370=EDGE_CURVE('',#7399,#7398,#4276,.T.);
#9371=EDGE_CURVE('',#7395,#7399,#4277,.T.);
#9372=EDGE_CURVE('',#7397,#7400,#4278,.T.);
#9373=EDGE_CURVE('',#7400,#7401,#4279,.T.);
#9374=EDGE_CURVE('',#7398,#7401,#4280,.T.);
#9375=EDGE_CURVE('',#7396,#7402,#4281,.T.);
#9376=EDGE_CURVE('',#7402,#7400,#4282,.T.);
#9377=EDGE_CURVE('',#7395,#7403,#4283,.T.);
#9378=EDGE_CURVE('',#7403,#7404,#4284,.T.);
#9379=EDGE_CURVE('',#7404,#7394,#4285,.T.);
#9380=EDGE_CURVE('',#7405,#7403,#4286,.T.);
#9381=EDGE_CURVE('',#7399,#7405,#4287,.T.);
#9382=EDGE_CURVE('',#7404,#7402,#4288,.T.);
#9383=EDGE_CURVE('',#7401,#7405,#4289,.T.);
#9384=EDGE_CURVE('',#7402,#7406,#4290,.T.);
#9385=EDGE_CURVE('',#7406,#7407,#4291,.T.);
#9386=EDGE_CURVE('',#7400,#7407,#4292,.T.);
#9387=EDGE_CURVE('',#7404,#7408,#4293,.T.);
#9388=EDGE_CURVE('',#7408,#7406,#4294,.T.);
#9389=EDGE_CURVE('',#7403,#7409,#4295,.T.);
#9390=EDGE_CURVE('',#7409,#7408,#4296,.T.);
#9391=EDGE_CURVE('',#7370,#7410,#6079,.T.);
#9392=EDGE_CURVE('',#7411,#7410,#1071,.F.);
#9393=EDGE_CURVE('',#7412,#7411,#1072,.F.);
#9394=EDGE_CURVE('',#7412,#7373,#6080,.T.);
#9395=EDGE_CURVE('',#7367,#7412,#6081,.T.);
#9396=EDGE_CURVE('',#7388,#7381,#6082,.T.);
#9397=EDGE_CURVE('',#7387,#7380,#6083,.T.);
#9398=EDGE_CURVE('',#7410,#7366,#6084,.T.);
#9399=EDGE_CURVE('',#7410,#7412,#1073,.F.);
#9400=EDGE_CURVE('',#7405,#7413,#4297,.T.);
#9401=EDGE_CURVE('',#7413,#7409,#4298,.T.);
#9402=EDGE_CURVE('',#7401,#7414,#4299,.T.);
#9403=EDGE_CURVE('',#7414,#7413,#4300,.T.);
#9404=EDGE_CURVE('',#7407,#7414,#4301,.T.);
#9405=EDGE_CURVE('',#7415,#7415,#1074,.T.);
#9406=EDGE_CURVE('',#7415,#7411,#4302,.T.);
#9407=EDGE_CURVE('',#7416,#7417,#1075,.T.);
#9408=EDGE_CURVE('',#7418,#7416,#4303,.T.);
#9409=EDGE_CURVE('',#7419,#7418,#1076,.T.);
#9410=EDGE_CURVE('',#7420,#7419,#4304,.T.);
#9411=EDGE_CURVE('',#7421,#7420,#1077,.T.);
#9412=EDGE_CURVE('',#7422,#7421,#4305,.T.);
#9413=EDGE_CURVE('',#7423,#7422,#1078,.T.);
#9414=EDGE_CURVE('',#7417,#7423,#4306,.T.);
#9415=EDGE_CURVE('',#7424,#7424,#1079,.T.);
#9416=EDGE_CURVE('',#7416,#7425,#4307,.T.);
#9417=EDGE_CURVE('',#7426,#7425,#4308,.T.);
#9418=EDGE_CURVE('',#7418,#7426,#4309,.T.);
#9419=EDGE_CURVE('',#7427,#7426,#1080,.T.);
#9420=EDGE_CURVE('',#7419,#7427,#4310,.T.);
#9421=EDGE_CURVE('',#7428,#7427,#4311,.T.);
#9422=EDGE_CURVE('',#7420,#7428,#4312,.T.);
#9423=EDGE_CURVE('',#7429,#7428,#1081,.T.);
#9424=EDGE_CURVE('',#7421,#7429,#4313,.T.);
#9425=EDGE_CURVE('',#7430,#7429,#4314,.T.);
#9426=EDGE_CURVE('',#7422,#7430,#4315,.T.);
#9427=EDGE_CURVE('',#7431,#7430,#1082,.T.);
#9428=EDGE_CURVE('',#7423,#7431,#4316,.T.);
#9429=EDGE_CURVE('',#7432,#7431,#4317,.T.);
#9430=EDGE_CURVE('',#7417,#7432,#4318,.T.);
#9431=EDGE_CURVE('',#7425,#7432,#1083,.T.);
#9432=EDGE_CURVE('',#7424,#7433,#4319,.T.);
#9433=EDGE_CURVE('',#7434,#7433,#254,.T.);
#9434=EDGE_CURVE('',#7435,#7434,#255,.T.);
#9435=EDGE_CURVE('',#7433,#7435,#256,.T.);
#9436=EDGE_CURVE('',#7434,#7436,#4320,.T.);
#9437=EDGE_CURVE('',#7437,#7436,#4321,.T.);
#9438=EDGE_CURVE('',#7438,#7437,#4322,.T.);
#9439=EDGE_CURVE('',#7439,#7438,#4323,.T.);
#9440=EDGE_CURVE('',#7440,#7439,#4324,.T.);
#9441=EDGE_CURVE('',#7440,#7441,#4325,.T.);
#9442=EDGE_CURVE('',#7441,#7435,#4326,.T.);
#9443=EDGE_CURVE('',#7442,#7442,#1084,.T.);
#9444=EDGE_CURVE('',#7442,#7443,#4327,.T.);
#9445=EDGE_CURVE('',#7443,#7443,#1085,.T.);
#9446=EDGE_CURVE('',#7444,#7445,#4328,.T.);
#9447=EDGE_CURVE('',#7444,#7445,#1086,.T.);
#9448=EDGE_CURVE('',#7446,#7447,#4329,.T.);
#9449=EDGE_CURVE('',#7446,#7447,#1087,.T.);
#9450=EDGE_CURVE('',#7448,#7449,#4330,.T.);
#9451=EDGE_CURVE('',#7448,#7449,#1088,.T.);
#9452=EDGE_CURVE('',#7450,#7451,#4331,.T.);
#9453=EDGE_CURVE('',#7452,#7451,#1089,.T.);
#9454=EDGE_CURVE('',#7450,#7452,#1090,.T.);
#9455=EDGE_CURVE('',#7438,#7437,#1091,.T.);
#9456=EDGE_CURVE('',#7453,#7454,#4332,.T.);
#9457=EDGE_CURVE('',#7453,#7454,#1092,.T.);
#9458=EDGE_CURVE('',#7455,#7455,#1093,.T.);
#9459=EDGE_CURVE('',#7455,#7452,#4333,.T.);
#9460=EDGE_CURVE('',#7446,#7451,#1094,.T.);
#9461=EDGE_CURVE('',#7444,#7447,#1095,.T.);
#9462=EDGE_CURVE('',#7448,#7445,#1096,.T.);
#9463=EDGE_CURVE('',#7438,#7449,#1097,.T.);
#9464=EDGE_CURVE('',#7453,#7437,#1098,.T.);
#9465=EDGE_CURVE('',#7450,#7454,#1099,.T.);
#9466=EDGE_CURVE('',#7456,#7456,#1100,.T.);
#9467=EDGE_CURVE('',#7456,#7455,#4334,.T.);
#9468=EDGE_CURVE('',#7445,#7457,#4335,.T.);
#9469=EDGE_CURVE('',#7457,#7448,#4336,.T.);
#9470=EDGE_CURVE('',#7449,#7439,#4337,.T.);
#9471=EDGE_CURVE('',#7447,#7458,#4338,.T.);
#9472=EDGE_CURVE('',#7458,#7444,#4339,.T.);
#9473=EDGE_CURVE('',#7436,#7453,#4340,.T.);
#9474=EDGE_CURVE('',#7451,#7459,#4341,.T.);
#9475=EDGE_CURVE('',#7459,#7446,#4342,.T.);
#9476=EDGE_CURVE('',#7460,#7461,#4343,.T.);
#9477=EDGE_CURVE('',#7462,#7460,#4344,.T.);
#9478=EDGE_CURVE('',#7463,#7462,#4345,.T.);
#9479=EDGE_CURVE('',#7441,#7463,#4346,.T.);
#9480=EDGE_CURVE('',#7461,#7440,#4347,.T.);
#9481=EDGE_CURVE('',#7464,#7464,#1101,.T.);
#9482=EDGE_CURVE('',#7460,#7458,#4348,.T.);
#9483=EDGE_CURVE('',#7462,#7459,#4349,.T.);
#9484=EDGE_CURVE('',#7465,#7450,#4350,.T.);
#9485=EDGE_CURVE('',#7463,#7465,#4351,.T.);
#9486=EDGE_CURVE('',#7454,#7465,#4352,.T.);
#9487=EDGE_CURVE('',#7461,#7457,#4353,.T.);
#9488=EDGE_CURVE('',#7466,#7466,#1102,.T.);
#9489=EDGE_CURVE('',#7467,#7467,#1103,.T.);
#9490=EDGE_CURVE('',#7467,#7466,#4354,.T.);
#9491=EDGE_CURVE('',#7464,#7467,#4355,.T.);
#9492=EDGE_CURVE('',#7468,#7469,#4356,.T.);
#9493=EDGE_CURVE('',#7470,#7468,#4357,.T.);
#9494=EDGE_CURVE('',#7469,#7470,#4358,.T.);
#9495=EDGE_CURVE('',#7471,#7472,#4359,.T.);
#9496=EDGE_CURVE('',#7473,#7471,#4360,.T.);
#9497=EDGE_CURVE('',#7472,#7473,#4361,.T.);
#9498=EDGE_CURVE('',#7474,#7475,#4362,.T.);
#9499=EDGE_CURVE('',#7476,#7474,#4363,.T.);
#9500=EDGE_CURVE('',#7475,#7476,#4364,.T.);
#9501=EDGE_CURVE('',#7470,#7476,#4365,.T.);
#9502=EDGE_CURVE('',#7474,#7469,#4366,.T.);
#9503=EDGE_CURVE('',#7477,#7478,#4367,.T.);
#9504=EDGE_CURVE('',#7479,#7477,#4368,.T.);
#9505=EDGE_CURVE('',#7478,#7479,#4369,.T.);
#9506=EDGE_CURVE('',#7480,#7481,#4370,.T.);
#9507=EDGE_CURVE('',#7482,#7480,#4371,.T.);
#9508=EDGE_CURVE('',#7481,#7482,#4372,.T.);
#9509=EDGE_CURVE('',#7483,#7484,#4373,.T.);
#9510=EDGE_CURVE('',#7485,#7483,#4374,.T.);
#9511=EDGE_CURVE('',#7484,#7485,#4375,.T.);
#9512=EDGE_CURVE('',#7480,#7485,#4376,.T.);
#9513=EDGE_CURVE('',#7483,#7482,#4377,.T.);
#9514=EDGE_CURVE('',#7485,#7479,#4378,.T.);
#9515=EDGE_CURVE('',#7477,#7484,#4379,.T.);
#9516=EDGE_CURVE('',#7486,#7487,#4380,.F.);
#9517=EDGE_CURVE('',#7487,#7483,#4381,.T.);
#9518=EDGE_CURVE('',#7484,#7486,#4382,.T.);
#9519=EDGE_CURVE('',#7488,#7489,#4383,.F.);
#9520=EDGE_CURVE('',#7489,#7481,#4384,.T.);
#9521=EDGE_CURVE('',#7482,#7488,#4385,.T.);
#9522=EDGE_CURVE('',#7476,#7480,#4386,.T.);
#9523=EDGE_CURVE('',#7481,#7475,#4387,.T.);
#9524=EDGE_CURVE('',#7479,#7473,#4388,.T.);
#9525=EDGE_CURVE('',#7471,#7478,#4389,.T.);
#9526=EDGE_CURVE('',#7490,#7491,#4390,.F.);
#9527=EDGE_CURVE('',#7491,#7477,#4391,.T.);
#9528=EDGE_CURVE('',#7478,#7490,#4392,.T.);
#9529=EDGE_CURVE('',#7492,#7493,#4393,.F.);
#9530=EDGE_CURVE('',#7493,#7474,#4394,.T.);
#9531=EDGE_CURVE('',#7475,#7492,#4395,.T.);
#9532=EDGE_CURVE('',#7473,#7470,#4396,.T.);
#9533=EDGE_CURVE('',#7468,#7472,#4397,.T.);
#9534=EDGE_CURVE('',#7494,#7495,#4398,.F.);
#9535=EDGE_CURVE('',#7495,#7471,#4399,.T.);
#9536=EDGE_CURVE('',#7472,#7494,#4400,.T.);
#9537=EDGE_CURVE('',#7496,#7497,#4401,.F.);
#9538=EDGE_CURVE('',#7497,#7468,#4402,.T.);
#9539=EDGE_CURVE('',#7469,#7496,#4403,.T.);
#9540=EDGE_CURVE('',#7486,#7491,#4404,.T.);
#9541=EDGE_CURVE('',#7490,#7495,#4405,.T.);
#9542=EDGE_CURVE('',#7494,#7497,#4406,.T.);
#9543=EDGE_CURVE('',#7498,#7498,#1104,.T.);
#9544=EDGE_CURVE('',#7499,#7500,#1105,.T.);
#9545=EDGE_CURVE('',#7500,#7499,#1106,.T.);
#9546=EDGE_CURVE('',#7499,#7501,#4407,.T.);
#9547=EDGE_CURVE('',#7501,#7502,#1107,.T.);
#9548=EDGE_CURVE('',#7502,#7501,#1108,.T.);
#9549=EDGE_CURVE('',#7502,#7503,#4408,.T.);
#9550=EDGE_CURVE('',#7504,#7503,#1109,.T.);
#9551=EDGE_CURVE('',#7503,#7504,#1110,.T.);
#9552=EDGE_CURVE('',#7505,#7505,#1111,.T.);
#9553=EDGE_CURVE('',#7505,#7500,#4409,.T.);
#9554=EDGE_CURVE('',#7504,#7506,#4410,.T.);
#9555=EDGE_CURVE('',#7506,#7506,#1112,.T.);
#9556=EDGE_CURVE('',#7507,#7507,#1113,.T.);
#9557=EDGE_CURVE('',#7507,#7508,#4411,.T.);
#9558=EDGE_CURVE('',#7508,#7509,#1114,.T.);
#9559=EDGE_CURVE('',#7509,#7508,#1115,.T.);
#9560=EDGE_CURVE('',#7509,#7510,#4412,.T.);
#9561=EDGE_CURVE('',#7510,#7510,#1116,.T.);
#9562=EDGE_CURVE('',#7492,#7489,#4413,.T.);
#9563=EDGE_CURVE('',#7488,#7487,#4414,.T.);
#9564=EDGE_CURVE('',#7496,#7493,#4415,.T.);
#9565=EDGE_CURVE('',#7511,#7511,#1117,.T.);
#9566=EDGE_CURVE('',#7512,#7512,#1118,.T.);
#9567=EDGE_CURVE('',#7513,#7513,#1119,.T.);
#9568=EDGE_CURVE('',#7511,#7513,#4416,.T.);
#9569=EDGE_CURVE('',#7514,#7514,#1120,.T.);
#9570=EDGE_CURVE('',#7514,#7512,#4417,.T.);
#9571=EDGE_CURVE('',#7515,#7515,#1121,.T.);
#9572=EDGE_CURVE('',#7516,#7516,#1122,.T.);
#9573=EDGE_CURVE('',#7515,#7516,#4418,.T.);
#9574=EDGE_CURVE('',#7517,#7517,#1123,.T.);
#9575=EDGE_CURVE('',#7517,#7498,#4419,.T.);
#9576=EDGE_CURVE('',#7518,#7518,#1124,.T.);
#9577=EDGE_CURVE('',#7518,#7517,#4420,.T.);
#9578=EDGE_CURVE('',#7519,#7520,#1125,.T.);
#9579=EDGE_CURVE('',#7521,#7521,#1126,.T.);
#9580=EDGE_CURVE('',#7521,#7522,#4421,.T.);
#9581=EDGE_CURVE('',#7522,#7522,#1127,.T.);
#9582=EDGE_CURVE('',#7523,#7523,#1128,.T.);
#9583=EDGE_CURVE('',#7524,#7524,#1129,.T.);
#9584=EDGE_CURVE('',#7524,#7523,#4422,.T.);
#9585=EDGE_CURVE('',#7525,#7525,#1130,.T.);
#9586=EDGE_CURVE('',#7525,#7524,#4423,.T.);
#9587=EDGE_CURVE('',#7526,#7526,#1131,.T.);
#9588=EDGE_CURVE('',#7526,#7525,#4424,.T.);
#9589=EDGE_CURVE('',#7527,#7527,#1132,.T.);
#9590=EDGE_CURVE('',#7527,#7528,#4425,.T.);
#9591=EDGE_CURVE('',#7528,#7528,#1133,.T.);
#9592=EDGE_CURVE('',#7529,#7530,#4426,.T.);
#9593=EDGE_CURVE('',#7531,#7529,#4427,.T.);
#9594=EDGE_CURVE('',#7532,#7531,#4428,.T.);
#9595=EDGE_CURVE('',#7530,#7532,#4429,.T.);
#9596=EDGE_CURVE('',#7533,#7533,#1134,.T.);
#9597=EDGE_CURVE('',#7534,#7534,#1135,.T.);
#9598=EDGE_CURVE('',#7535,#7535,#1136,.T.);
#9599=EDGE_CURVE('',#7536,#7536,#1137,.T.);
#9600=EDGE_CURVE('',#7537,#7537,#1138,.T.);
#9601=EDGE_CURVE('',#7538,#7538,#1139,.T.);
#9602=EDGE_CURVE('',#7538,#7528,#4430,.T.);
#9603=EDGE_CURVE('',#7533,#7539,#4431,.T.);
#9604=EDGE_CURVE('',#7539,#7539,#1140,.T.);
#9605=EDGE_CURVE('',#7540,#7540,#1141,.T.);
#9606=EDGE_CURVE('',#7540,#7539,#4432,.T.);
#9607=EDGE_CURVE('',#7541,#7542,#4433,.T.);
#9608=EDGE_CURVE('',#7542,#7543,#4434,.T.);
#9609=EDGE_CURVE('',#7543,#7544,#4435,.T.);
#9610=EDGE_CURVE('',#7544,#7541,#4436,.T.);
#9611=EDGE_CURVE('',#7541,#7545,#1142,.T.);
#9612=EDGE_CURVE('',#7545,#7546,#4437,.T.);
#9613=EDGE_CURVE('',#7546,#7542,#1143,.T.);
#9614=EDGE_CURVE('',#7547,#7548,#4438,.T.);
#9615=EDGE_CURVE('',#7548,#7546,#4439,.T.);
#9616=EDGE_CURVE('',#7545,#7547,#4440,.T.);
#9617=EDGE_CURVE('',#7547,#7549,#1144,.T.);
#9618=EDGE_CURVE('',#7549,#7550,#4441,.T.);
#9619=EDGE_CURVE('',#7550,#7548,#1145,.T.);
#9620=EDGE_CURVE('',#7551,#7552,#4442,.T.);
#9621=EDGE_CURVE('',#7552,#7550,#4443,.T.);
#9622=EDGE_CURVE('',#7549,#7551,#4444,.T.);
#9623=EDGE_CURVE('',#7551,#7553,#1146,.T.);
#9624=EDGE_CURVE('',#7553,#7554,#4445,.T.);
#9625=EDGE_CURVE('',#7554,#7552,#1147,.T.);
#9626=EDGE_CURVE('',#7555,#7556,#4446,.T.);
#9627=EDGE_CURVE('',#7556,#7554,#4447,.T.);
#9628=EDGE_CURVE('',#7553,#7555,#4448,.T.);
#9629=EDGE_CURVE('',#7555,#7529,#1148,.T.);
#9630=EDGE_CURVE('',#7529,#7557,#4449,.T.);
#9631=EDGE_CURVE('',#7557,#7556,#1149,.T.);
#9632=EDGE_CURVE('',#7530,#7558,#4450,.T.);
#9633=EDGE_CURVE('',#7558,#7557,#4451,.T.);
#9634=EDGE_CURVE('',#7530,#7559,#1150,.T.);
#9635=EDGE_CURVE('',#7559,#7560,#4452,.T.);
#9636=EDGE_CURVE('',#7560,#7558,#1151,.T.);
#9637=EDGE_CURVE('',#7561,#7562,#4453,.T.);
#9638=EDGE_CURVE('',#7562,#7560,#4454,.T.);
#9639=EDGE_CURVE('',#7559,#7561,#4455,.T.);
#9640=EDGE_CURVE('',#7561,#7563,#1152,.T.);
#9641=EDGE_CURVE('',#7563,#7564,#4456,.T.);
#9642=EDGE_CURVE('',#7564,#7562,#1153,.T.);
#9643=EDGE_CURVE('',#7565,#7566,#4457,.T.);
#9644=EDGE_CURVE('',#7566,#7564,#4458,.T.);
#9645=EDGE_CURVE('',#7563,#7565,#4459,.T.);
#9646=EDGE_CURVE('',#7565,#7567,#1154,.T.);
#9647=EDGE_CURVE('',#7567,#7568,#4460,.T.);
#9648=EDGE_CURVE('',#7568,#7566,#1155,.T.);
#9649=EDGE_CURVE('',#7569,#7570,#4461,.T.);
#9650=EDGE_CURVE('',#7570,#7568,#4462,.T.);
#9651=EDGE_CURVE('',#7567,#7569,#4463,.T.);
#9652=EDGE_CURVE('',#7569,#7544,#1156,.T.);
#9653=EDGE_CURVE('',#7543,#7570,#1157,.T.);
#9654=EDGE_CURVE('',#7555,#7571,#4464,.T.);
#9655=EDGE_CURVE('',#7531,#7571,#1158,.T.);
#9656=EDGE_CURVE('',#7572,#7553,#4465,.T.);
#9657=EDGE_CURVE('',#7571,#7572,#4466,.T.);
#9658=EDGE_CURVE('',#7551,#7573,#4467,.T.);
#9659=EDGE_CURVE('',#7572,#7573,#1159,.T.);
#9660=EDGE_CURVE('',#7574,#7549,#4468,.T.);
#9661=EDGE_CURVE('',#7573,#7574,#4469,.T.);
#9662=EDGE_CURVE('',#7547,#7575,#4470,.T.);
#9663=EDGE_CURVE('',#7574,#7575,#1160,.T.);
#9664=EDGE_CURVE('',#7576,#7545,#4471,.T.);
#9665=EDGE_CURVE('',#7575,#7576,#4472,.T.);
#9666=EDGE_CURVE('',#7541,#7577,#4473,.T.);
#9667=EDGE_CURVE('',#7576,#7577,#1161,.T.);
#9668=EDGE_CURVE('',#7578,#7544,#4474,.T.);
#9669=EDGE_CURVE('',#7577,#7578,#4475,.T.);
#9670=EDGE_CURVE('',#7579,#7579,#1162,.T.);
#9671=EDGE_CURVE('',#7580,#7580,#1163,.T.);
#9672=EDGE_CURVE('',#7581,#7581,#1164,.T.);
#9673=EDGE_CURVE('',#7582,#7582,#1165,.T.);
#9674=EDGE_CURVE('',#7583,#7583,#1166,.T.);
#9675=EDGE_CURVE('',#7584,#7584,#1167,.T.);
#9676=EDGE_CURVE('',#7578,#7585,#4476,.T.);
#9677=EDGE_CURVE('',#7585,#7586,#4477,.T.);
#9678=EDGE_CURVE('',#7586,#7577,#4478,.T.);
#9679=EDGE_CURVE('',#7578,#7587,#1168,.T.);
#9680=EDGE_CURVE('',#7587,#7588,#4479,.T.);
#9681=EDGE_CURVE('',#7588,#7585,#1169,.T.);
#9682=EDGE_CURVE('',#7589,#7590,#4480,.T.);
#9683=EDGE_CURVE('',#7590,#7588,#4481,.T.);
#9684=EDGE_CURVE('',#7587,#7589,#4482,.T.);
#9685=EDGE_CURVE('',#7589,#7591,#1170,.T.);
#9686=EDGE_CURVE('',#7591,#7592,#4483,.T.);
#9687=EDGE_CURVE('',#7592,#7590,#1171,.T.);
#9688=EDGE_CURVE('',#7593,#7594,#4484,.T.);
#9689=EDGE_CURVE('',#7594,#7592,#4485,.T.);
#9690=EDGE_CURVE('',#7591,#7593,#4486,.T.);
#9691=EDGE_CURVE('',#7593,#7595,#1172,.T.);
#9692=EDGE_CURVE('',#7595,#7596,#4487,.T.);
#9693=EDGE_CURVE('',#7596,#7594,#1173,.T.);
#9694=EDGE_CURVE('',#7597,#7598,#4488,.T.);
#9695=EDGE_CURVE('',#7598,#7596,#4489,.T.);
#9696=EDGE_CURVE('',#7595,#7597,#4490,.T.);
#9697=EDGE_CURVE('',#7597,#7532,#1174,.T.);
#9698=EDGE_CURVE('',#7532,#7599,#4491,.T.);
#9699=EDGE_CURVE('',#7599,#7598,#1175,.T.);
#9700=EDGE_CURVE('',#7531,#7600,#4492,.T.);
#9701=EDGE_CURVE('',#7600,#7599,#4493,.T.);
#9702=EDGE_CURVE('',#7571,#7601,#4494,.T.);
#9703=EDGE_CURVE('',#7601,#7600,#1176,.T.);
#9704=EDGE_CURVE('',#7572,#7602,#4495,.T.);
#9705=EDGE_CURVE('',#7602,#7601,#4496,.T.);
#9706=EDGE_CURVE('',#7573,#7603,#4497,.T.);
#9707=EDGE_CURVE('',#7603,#7602,#1177,.T.);
#9708=EDGE_CURVE('',#7574,#7604,#4498,.T.);
#9709=EDGE_CURVE('',#7604,#7603,#4499,.T.);
#9710=EDGE_CURVE('',#7575,#7605,#4500,.T.);
#9711=EDGE_CURVE('',#7605,#7604,#1178,.T.);
#9712=EDGE_CURVE('',#7576,#7606,#4501,.T.);
#9713=EDGE_CURVE('',#7606,#7605,#4502,.T.);
#9714=EDGE_CURVE('',#7586,#7606,#1179,.T.);
#9715=EDGE_CURVE('',#7597,#7559,#4503,.T.);
#9716=EDGE_CURVE('',#7561,#7595,#4504,.T.);
#9717=EDGE_CURVE('',#7593,#7563,#4505,.T.);
#9718=EDGE_CURVE('',#7565,#7591,#4506,.T.);
#9719=EDGE_CURVE('',#7589,#7567,#4507,.T.);
#9720=EDGE_CURVE('',#7569,#7587,#4508,.T.);
#9721=EDGE_CURVE('',#7584,#7540,#4509,.T.);
#9722=EDGE_CURVE('',#7579,#7538,#4510,.T.);
#9723=EDGE_CURVE('',#7580,#7537,#4511,.T.);
#9724=EDGE_CURVE('',#7581,#7536,#4512,.T.);
#9725=EDGE_CURVE('',#7582,#7535,#4513,.T.);
#9726=EDGE_CURVE('',#7583,#7534,#4514,.T.);
#9727=EDGE_CURVE('',#7607,#7608,#4515,.T.);
#9728=EDGE_CURVE('',#7607,#7609,#6085,.T.);
#9729=EDGE_CURVE('',#7609,#7610,#1180,.F.);
#9730=EDGE_CURVE('',#7610,#7608,#6086,.T.);
#9731=EDGE_CURVE('',#7611,#7612,#4516,.T.);
#9732=EDGE_CURVE('',#7611,#7607,#6087,.T.);
#9733=EDGE_CURVE('',#7608,#7612,#6088,.T.);
#9734=EDGE_CURVE('',#7613,#7614,#4517,.T.);
#9735=EDGE_CURVE('',#7613,#7611,#6089,.T.);
#9736=EDGE_CURVE('',#7612,#7614,#6090,.T.);
#9737=EDGE_CURVE('',#7615,#7616,#4518,.T.);
#9738=EDGE_CURVE('',#7615,#7613,#6091,.T.);
#9739=EDGE_CURVE('',#7614,#7616,#6092,.T.);
#9740=EDGE_CURVE('',#7617,#7618,#4519,.T.);
#9741=EDGE_CURVE('',#7617,#7615,#6093,.T.);
#9742=EDGE_CURVE('',#7616,#7618,#6094,.T.);
#9743=EDGE_CURVE('',#7619,#7620,#4520,.T.);
#9744=EDGE_CURVE('',#7619,#7617,#6095,.T.);
#9745=EDGE_CURVE('',#7618,#7620,#6096,.T.);
#9746=EDGE_CURVE('',#7621,#7622,#4521,.T.);
#9747=EDGE_CURVE('',#7621,#7619,#6097,.T.);
#9748=EDGE_CURVE('',#7620,#7622,#6098,.T.);
#9749=EDGE_CURVE('',#7623,#7624,#4522,.T.);
#9750=EDGE_CURVE('',#7623,#7621,#6099,.T.);
#9751=EDGE_CURVE('',#7622,#7624,#6100,.T.);
#9752=EDGE_CURVE('',#7625,#7626,#4523,.T.);
#9753=EDGE_CURVE('',#7625,#7623,#6101,.T.);
#9754=EDGE_CURVE('',#7624,#7626,#6102,.T.);
#9755=EDGE_CURVE('',#7627,#7628,#4524,.T.);
#9756=EDGE_CURVE('',#7629,#7627,#1181,.F.);
#9757=EDGE_CURVE('',#7629,#7625,#6103,.T.);
#9758=EDGE_CURVE('',#7626,#7628,#6104,.T.);
#9759=EDGE_CURVE('',#7630,#7631,#4525,.T.);
#9760=EDGE_CURVE('',#7630,#7632,#6105,.T.);
#9761=EDGE_CURVE('',#7633,#7632,#1182,.T.);
#9762=EDGE_CURVE('',#7631,#7633,#6106,.T.);
#9763=EDGE_CURVE('',#7634,#7635,#4526,.T.);
#9764=EDGE_CURVE('',#7634,#7630,#6107,.T.);
#9765=EDGE_CURVE('',#7635,#7631,#6108,.T.);
#9766=EDGE_CURVE('',#7636,#7637,#4527,.T.);
#9767=EDGE_CURVE('',#7636,#7634,#6109,.T.);
#9768=EDGE_CURVE('',#7637,#7635,#6110,.T.);
#9769=EDGE_CURVE('',#7638,#7639,#4528,.T.);
#9770=EDGE_CURVE('',#7638,#7636,#6111,.T.);
#9771=EDGE_CURVE('',#7639,#7637,#6112,.T.);
#9772=EDGE_CURVE('',#7640,#7641,#4529,.T.);
#9773=EDGE_CURVE('',#7640,#7638,#6113,.T.);
#9774=EDGE_CURVE('',#7641,#7639,#6114,.T.);
#9775=EDGE_CURVE('',#7642,#7643,#4530,.T.);
#9776=EDGE_CURVE('',#7642,#7640,#6115,.T.);
#9777=EDGE_CURVE('',#7643,#7641,#6116,.T.);
#9778=EDGE_CURVE('',#7644,#7645,#4531,.T.);
#9779=EDGE_CURVE('',#7644,#7642,#6117,.T.);
#9780=EDGE_CURVE('',#7645,#7643,#6118,.T.);
#9781=EDGE_CURVE('',#7646,#7647,#4532,.T.);
#9782=EDGE_CURVE('',#7646,#7644,#6119,.T.);
#9783=EDGE_CURVE('',#7647,#7645,#6120,.T.);
#9784=EDGE_CURVE('',#7648,#7649,#4533,.T.);
#9785=EDGE_CURVE('',#7648,#7646,#6121,.T.);
#9786=EDGE_CURVE('',#7649,#7647,#6122,.T.);
#9787=EDGE_CURVE('',#7650,#7651,#1183,.T.);
#9788=EDGE_CURVE('',#7651,#7650,#1184,.T.);
#9789=EDGE_CURVE('',#7650,#7652,#4534,.T.);
#9790=EDGE_CURVE('',#7652,#7653,#1185,.T.);
#9791=EDGE_CURVE('',#7653,#7652,#1186,.T.);
#9792=EDGE_CURVE('',#7653,#7654,#4535,.T.);
#9793=EDGE_CURVE('',#7655,#7654,#1187,.T.);
#9794=EDGE_CURVE('',#7654,#7655,#1188,.T.);
#9795=EDGE_CURVE('',#7656,#7656,#1189,.T.);
#9796=EDGE_CURVE('',#7656,#7651,#4536,.T.);
#9797=EDGE_CURVE('',#7655,#7657,#4537,.T.);
#9798=EDGE_CURVE('',#7657,#7657,#1190,.T.);
#9799=EDGE_CURVE('',#7632,#7629,#6123,.T.);
#9800=EDGE_CURVE('',#7658,#7629,#1191,.F.);
#9801=EDGE_CURVE('',#7658,#7633,#6124,.T.);
#9802=EDGE_CURVE('',#7628,#7658,#6125,.T.);
#9803=EDGE_CURVE('',#7659,#7610,#6126,.T.);
#9804=EDGE_CURVE('',#7659,#7649,#6127,.T.);
#9805=EDGE_CURVE('',#7660,#7659,#1192,.T.);
#9806=EDGE_CURVE('',#7660,#7648,#6128,.T.);
#9807=EDGE_CURVE('',#7609,#7660,#6129,.T.);
#9808=EDGE_CURVE('',#7627,#7658,#1193,.F.);
#9809=EDGE_CURVE('',#7661,#7661,#1194,.T.);
#9810=EDGE_CURVE('',#7661,#7656,#4538,.T.);
#9811=EDGE_CURVE('',#7662,#7662,#1195,.T.);
#9812=EDGE_CURVE('',#7662,#7627,#4539,.T.);
#9813=EDGE_CURVE('',#7663,#7664,#4540,.T.);
#9814=EDGE_CURVE('',#7663,#7665,#6130,.T.);
#9815=EDGE_CURVE('',#7665,#7666,#1196,.T.);
#9816=EDGE_CURVE('',#7666,#7664,#6131,.T.);
#9817=EDGE_CURVE('',#7667,#7668,#4541,.T.);
#9818=EDGE_CURVE('',#7667,#7663,#6132,.T.);
#9819=EDGE_CURVE('',#7664,#7668,#6133,.T.);
#9820=EDGE_CURVE('',#7669,#7670,#4542,.T.);
#9821=EDGE_CURVE('',#7669,#7667,#6134,.T.);
#9822=EDGE_CURVE('',#7668,#7670,#6135,.T.);
#9823=EDGE_CURVE('',#7671,#7672,#4543,.T.);
#9824=EDGE_CURVE('',#7671,#7669,#6136,.T.);
#9825=EDGE_CURVE('',#7670,#7672,#6137,.T.);
#9826=EDGE_CURVE('',#7673,#7674,#4544,.T.);
#9827=EDGE_CURVE('',#7673,#7671,#6138,.T.);
#9828=EDGE_CURVE('',#7672,#7674,#6139,.T.);
#9829=EDGE_CURVE('',#7675,#7676,#4545,.T.);
#9830=EDGE_CURVE('',#7675,#7673,#6140,.T.);
#9831=EDGE_CURVE('',#7674,#7676,#6141,.T.);
#9832=EDGE_CURVE('',#7677,#7678,#4546,.T.);
#9833=EDGE_CURVE('',#7677,#7675,#6142,.T.);
#9834=EDGE_CURVE('',#7676,#7678,#6143,.T.);
#9835=EDGE_CURVE('',#7679,#7680,#4547,.T.);
#9836=EDGE_CURVE('',#7679,#7677,#6144,.T.);
#9837=EDGE_CURVE('',#7678,#7680,#6145,.T.);
#9838=EDGE_CURVE('',#7681,#7682,#4548,.T.);
#9839=EDGE_CURVE('',#7681,#7679,#6146,.T.);
#9840=EDGE_CURVE('',#7680,#7682,#6147,.T.);
#9841=EDGE_CURVE('',#7683,#7684,#4549,.T.);
#9842=EDGE_CURVE('',#7683,#7681,#6148,.T.);
#9843=EDGE_CURVE('',#7682,#7684,#6149,.T.);
#9844=EDGE_CURVE('',#7685,#7686,#4550,.T.);
#9845=EDGE_CURVE('',#7685,#7683,#6150,.T.);
#9846=EDGE_CURVE('',#7684,#7686,#6151,.T.);
#9847=EDGE_CURVE('',#7687,#7688,#4551,.T.);
#9848=EDGE_CURVE('',#7687,#7685,#6152,.T.);
#9849=EDGE_CURVE('',#7686,#7688,#6153,.T.);
#9850=EDGE_CURVE('',#7689,#7690,#4552,.T.);
#9851=EDGE_CURVE('',#7689,#7687,#6154,.T.);
#9852=EDGE_CURVE('',#7688,#7690,#6155,.T.);
#9853=EDGE_CURVE('',#7691,#7692,#4553,.T.);
#9854=EDGE_CURVE('',#7691,#7689,#6156,.T.);
#9855=EDGE_CURVE('',#7690,#7692,#6157,.T.);
#9856=EDGE_CURVE('',#7693,#7694,#4554,.T.);
#9857=EDGE_CURVE('',#7693,#7691,#6158,.T.);
#9858=EDGE_CURVE('',#7692,#7694,#6159,.T.);
#9859=EDGE_CURVE('',#7695,#7696,#4555,.T.);
#9860=EDGE_CURVE('',#7695,#7693,#6160,.T.);
#9861=EDGE_CURVE('',#7694,#7696,#6161,.T.);
#9862=EDGE_CURVE('',#7697,#7698,#4556,.T.);
#9863=EDGE_CURVE('',#7697,#7695,#6162,.T.);
#9864=EDGE_CURVE('',#7696,#7698,#6163,.T.);
#9865=EDGE_CURVE('',#7699,#7700,#4557,.T.);
#9866=EDGE_CURVE('',#7699,#7697,#6164,.T.);
#9867=EDGE_CURVE('',#7698,#7700,#6165,.T.);
#9868=EDGE_CURVE('',#7701,#7702,#4558,.T.);
#9869=EDGE_CURVE('',#7701,#7699,#6166,.T.);
#9870=EDGE_CURVE('',#7700,#7702,#6167,.T.);
#9871=EDGE_CURVE('',#7703,#7704,#4559,.T.);
#9872=EDGE_CURVE('',#7703,#7701,#6168,.T.);
#9873=EDGE_CURVE('',#7702,#7704,#6169,.T.);
#9874=EDGE_CURVE('',#7705,#7706,#4560,.T.);
#9875=EDGE_CURVE('',#7705,#7703,#6170,.T.);
#9876=EDGE_CURVE('',#7704,#7706,#6171,.T.);
#9877=EDGE_CURVE('',#7707,#7708,#4561,.T.);
#9878=EDGE_CURVE('',#7707,#7705,#6172,.T.);
#9879=EDGE_CURVE('',#7706,#7708,#6173,.T.);
#9880=EDGE_CURVE('',#7709,#7710,#4562,.T.);
#9881=EDGE_CURVE('',#7709,#7707,#6174,.T.);
#9882=EDGE_CURVE('',#7708,#7710,#6175,.T.);
#9883=EDGE_CURVE('',#7711,#7712,#4563,.T.);
#9884=EDGE_CURVE('',#7711,#7709,#6176,.T.);
#9885=EDGE_CURVE('',#7710,#7712,#6177,.T.);
#9886=EDGE_CURVE('',#7713,#7714,#4564,.T.);
#9887=EDGE_CURVE('',#7713,#7711,#6178,.T.);
#9888=EDGE_CURVE('',#7712,#7714,#6179,.T.);
#9889=EDGE_CURVE('',#7715,#7716,#4565,.T.);
#9890=EDGE_CURVE('',#7715,#7713,#6180,.T.);
#9891=EDGE_CURVE('',#7714,#7716,#6181,.T.);
#9892=EDGE_CURVE('',#7717,#7718,#4566,.T.);
#9893=EDGE_CURVE('',#7717,#7715,#6182,.T.);
#9894=EDGE_CURVE('',#7716,#7718,#6183,.T.);
#9895=EDGE_CURVE('',#7719,#7720,#4567,.T.);
#9896=EDGE_CURVE('',#7719,#7717,#6184,.T.);
#9897=EDGE_CURVE('',#7718,#7720,#6185,.T.);
#9898=EDGE_CURVE('',#7721,#7722,#4568,.T.);
#9899=EDGE_CURVE('',#7721,#7719,#6186,.T.);
#9900=EDGE_CURVE('',#7720,#7722,#6187,.T.);
#9901=EDGE_CURVE('',#7723,#7724,#4569,.T.);
#9902=EDGE_CURVE('',#7723,#7721,#6188,.T.);
#9903=EDGE_CURVE('',#7722,#7724,#6189,.T.);
#9904=EDGE_CURVE('',#7725,#7726,#4570,.T.);
#9905=EDGE_CURVE('',#7725,#7723,#6190,.T.);
#9906=EDGE_CURVE('',#7724,#7726,#6191,.T.);
#9907=EDGE_CURVE('',#7727,#7728,#4571,.T.);
#9908=EDGE_CURVE('',#7727,#7725,#6192,.T.);
#9909=EDGE_CURVE('',#7726,#7728,#6193,.T.);
#9910=EDGE_CURVE('',#7729,#7730,#4572,.T.);
#9911=EDGE_CURVE('',#7729,#7727,#6194,.T.);
#9912=EDGE_CURVE('',#7728,#7730,#6195,.T.);
#9913=EDGE_CURVE('',#7731,#7732,#4573,.T.);
#9914=EDGE_CURVE('',#7731,#7729,#6196,.T.);
#9915=EDGE_CURVE('',#7730,#7732,#6197,.T.);
#9916=EDGE_CURVE('',#7733,#7734,#4574,.T.);
#9917=EDGE_CURVE('',#7733,#7731,#6198,.T.);
#9918=EDGE_CURVE('',#7732,#7734,#6199,.T.);
#9919=EDGE_CURVE('',#7735,#7736,#4575,.T.);
#9920=EDGE_CURVE('',#7735,#7733,#6200,.T.);
#9921=EDGE_CURVE('',#7734,#7736,#6201,.T.);
#9922=EDGE_CURVE('',#7737,#7738,#4576,.T.);
#9923=EDGE_CURVE('',#7737,#7735,#6202,.T.);
#9924=EDGE_CURVE('',#7736,#7738,#6203,.T.);
#9925=EDGE_CURVE('',#7739,#7740,#4577,.T.);
#9926=EDGE_CURVE('',#7739,#7737,#6204,.T.);
#9927=EDGE_CURVE('',#7738,#7740,#6205,.T.);
#9928=EDGE_CURVE('',#7741,#7742,#4578,.T.);
#9929=EDGE_CURVE('',#7741,#7739,#6206,.T.);
#9930=EDGE_CURVE('',#7740,#7742,#6207,.T.);
#9931=EDGE_CURVE('',#7743,#7744,#4579,.T.);
#9932=EDGE_CURVE('',#7743,#7741,#6208,.T.);
#9933=EDGE_CURVE('',#7742,#7744,#6209,.T.);
#9934=EDGE_CURVE('',#7745,#7746,#4580,.T.);
#9935=EDGE_CURVE('',#7745,#7743,#6210,.T.);
#9936=EDGE_CURVE('',#7744,#7746,#6211,.T.);
#9937=EDGE_CURVE('',#7747,#7748,#4581,.T.);
#9938=EDGE_CURVE('',#7747,#7745,#6212,.T.);
#9939=EDGE_CURVE('',#7746,#7748,#6213,.T.);
#9940=EDGE_CURVE('',#7749,#7750,#4582,.T.);
#9941=EDGE_CURVE('',#7749,#7747,#6214,.T.);
#9942=EDGE_CURVE('',#7748,#7750,#6215,.T.);
#9943=EDGE_CURVE('',#7751,#7752,#4583,.T.);
#9944=EDGE_CURVE('',#7751,#7749,#6216,.T.);
#9945=EDGE_CURVE('',#7750,#7752,#6217,.T.);
#9946=EDGE_CURVE('',#7753,#7754,#4584,.T.);
#9947=EDGE_CURVE('',#7753,#7755,#6218,.T.);
#9948=EDGE_CURVE('',#7754,#7755,#1197,.T.);
#9949=EDGE_CURVE('',#7756,#7757,#4585,.T.);
#9950=EDGE_CURVE('',#7756,#7753,#6219,.T.);
#9951=EDGE_CURVE('',#7758,#7754,#1198,.T.);
#9952=EDGE_CURVE('',#7757,#7758,#6220,.T.);
#9953=EDGE_CURVE('',#7759,#7760,#4586,.T.);
#9954=EDGE_CURVE('',#7759,#7756,#6221,.T.);
#9955=EDGE_CURVE('',#7760,#7757,#6222,.T.);
#9956=EDGE_CURVE('',#7761,#7762,#4587,.T.);
#9957=EDGE_CURVE('',#7761,#7759,#6223,.T.);
#9958=EDGE_CURVE('',#7762,#7760,#6224,.T.);
#9959=EDGE_CURVE('',#7763,#7764,#4588,.T.);
#9960=EDGE_CURVE('',#7763,#7761,#6225,.T.);
#9961=EDGE_CURVE('',#7764,#7762,#6226,.T.);
#9962=EDGE_CURVE('',#7765,#7766,#4589,.T.);
#9963=EDGE_CURVE('',#7765,#7763,#6227,.T.);
#9964=EDGE_CURVE('',#7766,#7764,#6228,.T.);
#9965=EDGE_CURVE('',#7767,#7768,#4590,.T.);
#9966=EDGE_CURVE('',#7767,#7765,#6229,.T.);
#9967=EDGE_CURVE('',#7768,#7766,#6230,.T.);
#9968=EDGE_CURVE('',#7769,#7770,#4591,.T.);
#9969=EDGE_CURVE('',#7769,#7767,#6231,.T.);
#9970=EDGE_CURVE('',#7770,#7768,#6232,.T.);
#9971=EDGE_CURVE('',#7771,#7772,#4592,.T.);
#9972=EDGE_CURVE('',#7771,#7769,#6233,.T.);
#9973=EDGE_CURVE('',#7772,#7770,#6234,.T.);
#9974=EDGE_CURVE('',#7773,#7774,#4593,.T.);
#9975=EDGE_CURVE('',#7773,#7771,#6235,.T.);
#9976=EDGE_CURVE('',#7774,#7772,#6236,.T.);
#9977=EDGE_CURVE('',#7775,#7776,#4594,.T.);
#9978=EDGE_CURVE('',#7775,#7773,#6237,.T.);
#9979=EDGE_CURVE('',#7776,#7774,#6238,.T.);
#9980=EDGE_CURVE('',#7777,#7778,#4595,.T.);
#9981=EDGE_CURVE('',#7777,#7775,#6239,.T.);
#9982=EDGE_CURVE('',#7778,#7776,#6240,.T.);
#9983=EDGE_CURVE('',#7779,#7780,#4596,.T.);
#9984=EDGE_CURVE('',#7779,#7777,#6241,.T.);
#9985=EDGE_CURVE('',#7780,#7778,#6242,.T.);
#9986=EDGE_CURVE('',#7781,#7782,#4597,.T.);
#9987=EDGE_CURVE('',#7781,#7779,#6243,.T.);
#9988=EDGE_CURVE('',#7782,#7780,#6244,.T.);
#9989=EDGE_CURVE('',#7783,#7784,#4598,.T.);
#9990=EDGE_CURVE('',#7783,#7781,#6245,.T.);
#9991=EDGE_CURVE('',#7784,#7782,#6246,.T.);
#9992=EDGE_CURVE('',#7785,#7786,#4599,.T.);
#9993=EDGE_CURVE('',#7785,#7783,#6247,.T.);
#9994=EDGE_CURVE('',#7786,#7784,#6248,.T.);
#9995=EDGE_CURVE('',#7787,#7788,#4600,.T.);
#9996=EDGE_CURVE('',#7787,#7785,#6249,.T.);
#9997=EDGE_CURVE('',#7788,#7786,#6250,.T.);
#9998=EDGE_CURVE('',#7789,#7790,#4601,.T.);
#9999=EDGE_CURVE('',#7789,#7787,#6251,.T.);
#10000=EDGE_CURVE('',#7790,#7788,#6252,.T.);
#10001=EDGE_CURVE('',#7791,#7792,#4602,.T.);
#10002=EDGE_CURVE('',#7791,#7789,#6253,.T.);
#10003=EDGE_CURVE('',#7792,#7790,#6254,.T.);
#10004=EDGE_CURVE('',#7793,#7794,#4603,.T.);
#10005=EDGE_CURVE('',#7793,#7791,#6255,.T.);
#10006=EDGE_CURVE('',#7794,#7792,#6256,.T.);
#10007=EDGE_CURVE('',#7795,#7796,#4604,.T.);
#10008=EDGE_CURVE('',#7795,#7793,#6257,.T.);
#10009=EDGE_CURVE('',#7796,#7794,#6258,.T.);
#10010=EDGE_CURVE('',#7797,#7798,#4605,.T.);
#10011=EDGE_CURVE('',#7797,#7795,#6259,.T.);
#10012=EDGE_CURVE('',#7798,#7796,#6260,.T.);
#10013=EDGE_CURVE('',#7799,#7800,#4606,.T.);
#10014=EDGE_CURVE('',#7799,#7797,#6261,.T.);
#10015=EDGE_CURVE('',#7800,#7798,#6262,.T.);
#10016=EDGE_CURVE('',#7801,#7802,#4607,.T.);
#10017=EDGE_CURVE('',#7801,#7799,#6263,.T.);
#10018=EDGE_CURVE('',#7802,#7800,#6264,.T.);
#10019=EDGE_CURVE('',#7803,#7804,#4608,.T.);
#10020=EDGE_CURVE('',#7803,#7801,#6265,.T.);
#10021=EDGE_CURVE('',#7804,#7802,#6266,.T.);
#10022=EDGE_CURVE('',#7805,#7806,#4609,.T.);
#10023=EDGE_CURVE('',#7805,#7803,#6267,.T.);
#10024=EDGE_CURVE('',#7806,#7804,#6268,.T.);
#10025=EDGE_CURVE('',#7807,#7808,#4610,.T.);
#10026=EDGE_CURVE('',#7807,#7805,#6269,.T.);
#10027=EDGE_CURVE('',#7808,#7806,#6270,.T.);
#10028=EDGE_CURVE('',#7809,#7810,#4611,.T.);
#10029=EDGE_CURVE('',#7809,#7807,#6271,.T.);
#10030=EDGE_CURVE('',#7810,#7808,#6272,.T.);
#10031=EDGE_CURVE('',#7811,#7812,#4612,.T.);
#10032=EDGE_CURVE('',#7811,#7809,#6273,.T.);
#10033=EDGE_CURVE('',#7812,#7810,#6274,.T.);
#10034=EDGE_CURVE('',#7813,#7814,#4613,.T.);
#10035=EDGE_CURVE('',#7813,#7811,#6275,.T.);
#10036=EDGE_CURVE('',#7814,#7812,#6276,.T.);
#10037=EDGE_CURVE('',#7815,#7816,#4614,.T.);
#10038=EDGE_CURVE('',#7815,#7813,#6277,.T.);
#10039=EDGE_CURVE('',#7816,#7814,#6278,.T.);
#10040=EDGE_CURVE('',#7817,#7818,#4615,.T.);
#10041=EDGE_CURVE('',#7817,#7815,#6279,.T.);
#10042=EDGE_CURVE('',#7818,#7816,#6280,.T.);
#10043=EDGE_CURVE('',#7819,#7820,#4616,.T.);
#10044=EDGE_CURVE('',#7819,#7817,#6281,.T.);
#10045=EDGE_CURVE('',#7820,#7818,#6282,.T.);
#10046=EDGE_CURVE('',#7821,#7822,#4617,.T.);
#10047=EDGE_CURVE('',#7821,#7819,#6283,.T.);
#10048=EDGE_CURVE('',#7822,#7820,#6284,.T.);
#10049=EDGE_CURVE('',#7823,#7824,#4618,.T.);
#10050=EDGE_CURVE('',#7823,#7821,#6285,.T.);
#10051=EDGE_CURVE('',#7824,#7822,#6286,.T.);
#10052=EDGE_CURVE('',#7825,#7826,#4619,.T.);
#10053=EDGE_CURVE('',#7825,#7823,#6287,.T.);
#10054=EDGE_CURVE('',#7826,#7824,#6288,.T.);
#10055=EDGE_CURVE('',#7827,#7828,#4620,.T.);
#10056=EDGE_CURVE('',#7827,#7825,#6289,.T.);
#10057=EDGE_CURVE('',#7828,#7826,#6290,.T.);
#10058=EDGE_CURVE('',#7829,#7830,#4621,.T.);
#10059=EDGE_CURVE('',#7829,#7827,#6291,.T.);
#10060=EDGE_CURVE('',#7830,#7828,#6292,.T.);
#10061=EDGE_CURVE('',#7831,#7832,#4622,.T.);
#10062=EDGE_CURVE('',#7831,#7829,#6293,.T.);
#10063=EDGE_CURVE('',#7832,#7830,#6294,.T.);
#10064=EDGE_CURVE('',#7833,#7834,#4623,.T.);
#10065=EDGE_CURVE('',#7833,#7831,#6295,.T.);
#10066=EDGE_CURVE('',#7834,#7832,#6296,.T.);
#10067=EDGE_CURVE('',#7835,#7836,#4624,.T.);
#10068=EDGE_CURVE('',#7835,#7833,#6297,.T.);
#10069=EDGE_CURVE('',#7836,#7834,#6298,.T.);
#10070=EDGE_CURVE('',#7837,#7838,#4625,.T.);
#10071=EDGE_CURVE('',#7837,#7835,#6299,.T.);
#10072=EDGE_CURVE('',#7838,#7836,#6300,.T.);
#10073=EDGE_CURVE('',#7839,#7840,#4626,.T.);
#10074=EDGE_CURVE('',#7839,#7837,#6301,.T.);
#10075=EDGE_CURVE('',#7840,#7838,#6302,.T.);
#10076=EDGE_CURVE('',#7841,#7842,#4627,.T.);
#10077=EDGE_CURVE('',#7841,#7839,#6303,.T.);
#10078=EDGE_CURVE('',#7842,#7840,#6304,.T.);
#10079=EDGE_CURVE('',#7843,#7758,#6305,.T.);
#10080=EDGE_CURVE('',#7752,#7843,#6306,.T.);
#10081=EDGE_CURVE('',#7844,#7666,#6307,.T.);
#10082=EDGE_CURVE('',#7844,#7842,#6308,.T.);
#10083=EDGE_CURVE('',#7666,#7845,#1199,.T.);
#10084=EDGE_CURVE('',#7845,#7665,#1200,.T.);
#10085=EDGE_CURVE('',#7665,#7846,#6309,.T.);
#10086=EDGE_CURVE('',#7846,#7844,#1201,.T.);
#10087=EDGE_CURVE('',#7846,#7841,#6310,.T.);
#10088=EDGE_CURVE('',#7755,#7847,#6311,.T.);
#10089=EDGE_CURVE('',#7847,#7751,#6312,.T.);
#10090=EDGE_CURVE('',#7848,#7849,#1778,.T.);
#10091=EDGE_CURVE('',#7850,#7848,#1779,.T.);
#10092=EDGE_CURVE('',#7851,#7850,#1780,.T.);
#10093=EDGE_CURVE('',#7852,#7851,#1781,.T.);
#10094=EDGE_CURVE('',#7853,#7852,#1782,.T.);
#10095=EDGE_CURVE('',#7853,#7854,#4628,.T.);
#10096=EDGE_CURVE('',#7854,#7854,#1202,.T.);
#10097=EDGE_CURVE('',#7855,#7853,#1783,.T.);
#10098=EDGE_CURVE('',#7849,#7855,#1784,.T.);
#10099=EDGE_CURVE('',#7856,#7851,#4629,.T.);
#10100=EDGE_CURVE('',#7856,#7857,#4630,.T.);
#10101=EDGE_CURVE('',#7857,#7852,#4631,.T.);
#10102=EDGE_CURVE('',#7858,#7850,#4632,.T.);
#10103=EDGE_CURVE('',#7858,#7856,#4633,.T.);
#10104=EDGE_CURVE('',#7859,#7848,#4634,.T.);
#10105=EDGE_CURVE('',#7859,#7858,#4635,.T.);
#10106=EDGE_CURVE('',#7860,#7859,#4636,.T.);
#10107=EDGE_CURVE('',#7861,#7860,#4637,.T.);
#10108=EDGE_CURVE('',#7857,#7861,#4638,.T.);
#10109=EDGE_CURVE('',#7847,#7843,#1203,.F.);
#10110=EDGE_CURVE('',#7860,#7849,#4639,.T.);
#10111=EDGE_CURVE('',#7861,#7855,#4640,.T.);
#10112=EDGE_CURVE('',#7862,#7862,#1204,.T.);
#10113=EDGE_CURVE('',#7845,#7862,#4641,.T.);
#10114=EDGE_CURVE('',#7863,#7864,#4642,.T.);
#10115=EDGE_CURVE('',#7863,#7865,#6313,.T.);
#10116=EDGE_CURVE('',#7865,#7866,#1205,.T.);
#10117=EDGE_CURVE('',#7866,#7864,#6314,.T.);
#10118=EDGE_CURVE('',#7867,#7868,#4643,.T.);
#10119=EDGE_CURVE('',#7867,#7863,#6315,.T.);
#10120=EDGE_CURVE('',#7864,#7868,#6316,.T.);
#10121=EDGE_CURVE('',#7869,#7870,#4644,.T.);
#10122=EDGE_CURVE('',#7869,#7867,#6317,.T.);
#10123=EDGE_CURVE('',#7868,#7870,#6318,.T.);
#10124=EDGE_CURVE('',#7871,#7872,#4645,.T.);
#10125=EDGE_CURVE('',#7871,#7869,#6319,.T.);
#10126=EDGE_CURVE('',#7870,#7872,#6320,.T.);
#10127=EDGE_CURVE('',#7873,#7874,#4646,.T.);
#10128=EDGE_CURVE('',#7873,#7871,#6321,.T.);
#10129=EDGE_CURVE('',#7872,#7874,#6322,.T.);
#10130=EDGE_CURVE('',#7875,#7876,#4647,.T.);
#10131=EDGE_CURVE('',#7875,#7873,#6323,.T.);
#10132=EDGE_CURVE('',#7874,#7876,#6324,.T.);
#10133=EDGE_CURVE('',#7877,#7878,#4648,.T.);
#10134=EDGE_CURVE('',#7877,#7875,#6325,.T.);
#10135=EDGE_CURVE('',#7876,#7878,#6326,.T.);
#10136=EDGE_CURVE('',#7879,#7880,#4649,.T.);
#10137=EDGE_CURVE('',#7879,#7877,#6327,.T.);
#10138=EDGE_CURVE('',#7878,#7880,#6328,.T.);
#10139=EDGE_CURVE('',#7881,#7882,#4650,.T.);
#10140=EDGE_CURVE('',#7881,#7879,#6329,.T.);
#10141=EDGE_CURVE('',#7880,#7882,#6330,.T.);
#10142=EDGE_CURVE('',#7883,#7884,#4651,.T.);
#10143=EDGE_CURVE('',#7883,#7881,#6331,.T.);
#10144=EDGE_CURVE('',#7882,#7884,#6332,.T.);
#10145=EDGE_CURVE('',#7885,#7886,#4652,.T.);
#10146=EDGE_CURVE('',#7885,#7883,#6333,.T.);
#10147=EDGE_CURVE('',#7884,#7886,#6334,.T.);
#10148=EDGE_CURVE('',#7887,#7888,#4653,.T.);
#10149=EDGE_CURVE('',#7887,#7885,#6335,.T.);
#10150=EDGE_CURVE('',#7886,#7888,#6336,.T.);
#10151=EDGE_CURVE('',#7889,#7890,#4654,.T.);
#10152=EDGE_CURVE('',#7889,#7887,#6337,.T.);
#10153=EDGE_CURVE('',#7888,#7890,#6338,.T.);
#10154=EDGE_CURVE('',#7891,#7892,#4655,.T.);
#10155=EDGE_CURVE('',#7891,#7889,#6339,.T.);
#10156=EDGE_CURVE('',#7890,#7892,#6340,.T.);
#10157=EDGE_CURVE('',#7893,#7894,#4656,.T.);
#10158=EDGE_CURVE('',#7893,#7891,#6341,.T.);
#10159=EDGE_CURVE('',#7892,#7894,#6342,.T.);
#10160=EDGE_CURVE('',#7895,#7896,#4657,.T.);
#10161=EDGE_CURVE('',#7895,#7893,#6343,.T.);
#10162=EDGE_CURVE('',#7894,#7896,#6344,.T.);
#10163=EDGE_CURVE('',#7897,#7898,#4658,.T.);
#10164=EDGE_CURVE('',#7897,#7895,#6345,.T.);
#10165=EDGE_CURVE('',#7896,#7898,#6346,.T.);
#10166=EDGE_CURVE('',#7899,#7900,#4659,.T.);
#10167=EDGE_CURVE('',#7899,#7897,#6347,.T.);
#10168=EDGE_CURVE('',#7898,#7900,#6348,.T.);
#10169=EDGE_CURVE('',#7901,#7902,#4660,.T.);
#10170=EDGE_CURVE('',#7901,#7899,#6349,.T.);
#10171=EDGE_CURVE('',#7900,#7902,#6350,.T.);
#10172=EDGE_CURVE('',#7903,#7904,#4661,.T.);
#10173=EDGE_CURVE('',#7903,#7901,#6351,.T.);
#10174=EDGE_CURVE('',#7902,#7904,#6352,.T.);
#10175=EDGE_CURVE('',#7905,#7906,#4662,.T.);
#10176=EDGE_CURVE('',#7905,#7903,#6353,.T.);
#10177=EDGE_CURVE('',#7904,#7906,#6354,.T.);
#10178=EDGE_CURVE('',#7907,#7908,#4663,.T.);
#10179=EDGE_CURVE('',#7907,#7905,#6355,.T.);
#10180=EDGE_CURVE('',#7906,#7908,#6356,.T.);
#10181=EDGE_CURVE('',#7909,#7910,#4664,.T.);
#10182=EDGE_CURVE('',#7909,#7907,#6357,.T.);
#10183=EDGE_CURVE('',#7908,#7910,#6358,.T.);
#10184=EDGE_CURVE('',#7911,#7912,#4665,.T.);
#10185=EDGE_CURVE('',#7911,#7909,#6359,.T.);
#10186=EDGE_CURVE('',#7910,#7912,#6360,.T.);
#10187=EDGE_CURVE('',#7913,#7914,#4666,.T.);
#10188=EDGE_CURVE('',#7913,#7911,#6361,.T.);
#10189=EDGE_CURVE('',#7912,#7914,#6362,.T.);
#10190=EDGE_CURVE('',#7915,#7916,#4667,.T.);
#10191=EDGE_CURVE('',#7915,#7913,#6363,.T.);
#10192=EDGE_CURVE('',#7914,#7916,#6364,.T.);
#10193=EDGE_CURVE('',#7917,#7918,#4668,.T.);
#10194=EDGE_CURVE('',#7917,#7915,#6365,.T.);
#10195=EDGE_CURVE('',#7916,#7918,#6366,.T.);
#10196=EDGE_CURVE('',#7919,#7920,#4669,.T.);
#10197=EDGE_CURVE('',#7919,#7917,#6367,.T.);
#10198=EDGE_CURVE('',#7918,#7920,#6368,.T.);
#10199=EDGE_CURVE('',#7921,#7922,#4670,.T.);
#10200=EDGE_CURVE('',#7921,#7919,#6369,.T.);
#10201=EDGE_CURVE('',#7920,#7922,#6370,.T.);
#10202=EDGE_CURVE('',#7923,#7924,#4671,.T.);
#10203=EDGE_CURVE('',#7923,#7921,#6371,.T.);
#10204=EDGE_CURVE('',#7922,#7924,#6372,.T.);
#10205=EDGE_CURVE('',#7925,#7926,#4672,.T.);
#10206=EDGE_CURVE('',#7925,#7923,#6373,.T.);
#10207=EDGE_CURVE('',#7924,#7926,#6374,.T.);
#10208=EDGE_CURVE('',#7927,#7928,#4673,.T.);
#10209=EDGE_CURVE('',#7927,#7925,#6375,.T.);
#10210=EDGE_CURVE('',#7926,#7928,#6376,.T.);
#10211=EDGE_CURVE('',#7929,#7930,#4674,.T.);
#10212=EDGE_CURVE('',#7929,#7927,#6377,.T.);
#10213=EDGE_CURVE('',#7928,#7930,#6378,.T.);
#10214=EDGE_CURVE('',#7931,#7932,#4675,.T.);
#10215=EDGE_CURVE('',#7931,#7929,#6379,.T.);
#10216=EDGE_CURVE('',#7930,#7932,#6380,.T.);
#10217=EDGE_CURVE('',#7933,#7934,#4676,.T.);
#10218=EDGE_CURVE('',#7933,#7931,#6381,.T.);
#10219=EDGE_CURVE('',#7932,#7934,#6382,.T.);
#10220=EDGE_CURVE('',#7935,#7936,#4677,.T.);
#10221=EDGE_CURVE('',#7935,#7933,#6383,.T.);
#10222=EDGE_CURVE('',#7934,#7936,#6384,.T.);
#10223=EDGE_CURVE('',#7937,#7938,#4678,.T.);
#10224=EDGE_CURVE('',#7937,#7935,#6385,.T.);
#10225=EDGE_CURVE('',#7936,#7938,#6386,.T.);
#10226=EDGE_CURVE('',#7939,#7940,#4679,.T.);
#10227=EDGE_CURVE('',#7939,#7937,#6387,.T.);
#10228=EDGE_CURVE('',#7938,#7940,#6388,.T.);
#10229=EDGE_CURVE('',#7941,#7942,#4680,.T.);
#10230=EDGE_CURVE('',#7941,#7939,#6389,.T.);
#10231=EDGE_CURVE('',#7940,#7942,#6390,.T.);
#10232=EDGE_CURVE('',#7943,#7944,#4681,.T.);
#10233=EDGE_CURVE('',#7943,#7941,#6391,.T.);
#10234=EDGE_CURVE('',#7942,#7944,#6392,.T.);
#10235=EDGE_CURVE('',#7945,#7946,#4682,.T.);
#10236=EDGE_CURVE('',#7945,#7943,#6393,.T.);
#10237=EDGE_CURVE('',#7944,#7946,#6394,.T.);
#10238=EDGE_CURVE('',#7947,#7948,#4683,.T.);
#10239=EDGE_CURVE('',#7947,#7945,#6395,.T.);
#10240=EDGE_CURVE('',#7946,#7948,#6396,.T.);
#10241=EDGE_CURVE('',#7949,#7950,#4684,.T.);
#10242=EDGE_CURVE('',#7949,#7947,#6397,.T.);
#10243=EDGE_CURVE('',#7948,#7950,#6398,.T.);
#10244=EDGE_CURVE('',#7951,#7952,#4685,.T.);
#10245=EDGE_CURVE('',#7951,#7949,#6399,.T.);
#10246=EDGE_CURVE('',#7950,#7952,#6400,.T.);
#10247=EDGE_CURVE('',#7953,#7954,#4686,.T.);
#10248=EDGE_CURVE('',#7953,#7951,#6401,.T.);
#10249=EDGE_CURVE('',#7952,#7954,#6402,.T.);
#10250=EDGE_CURVE('',#7955,#7956,#4687,.T.);
#10251=EDGE_CURVE('',#7955,#7953,#6403,.T.);
#10252=EDGE_CURVE('',#7954,#7956,#6404,.T.);
#10253=EDGE_CURVE('',#7957,#7958,#4688,.T.);
#10254=EDGE_CURVE('',#7957,#7955,#6405,.T.);
#10255=EDGE_CURVE('',#7956,#7958,#6406,.T.);
#10256=EDGE_CURVE('',#7959,#7960,#4689,.T.);
#10257=EDGE_CURVE('',#7959,#7957,#6407,.T.);
#10258=EDGE_CURVE('',#7958,#7960,#6408,.T.);
#10259=EDGE_CURVE('',#7961,#7962,#4690,.T.);
#10260=EDGE_CURVE('',#7961,#7959,#6409,.T.);
#10261=EDGE_CURVE('',#7960,#7962,#6410,.T.);
#10262=EDGE_CURVE('',#7963,#7964,#4691,.T.);
#10263=EDGE_CURVE('',#7963,#7961,#6411,.T.);
#10264=EDGE_CURVE('',#7962,#7964,#6412,.T.);
#10265=EDGE_CURVE('',#7965,#7966,#4692,.T.);
#10266=EDGE_CURVE('',#7965,#7963,#6413,.T.);
#10267=EDGE_CURVE('',#7964,#7966,#6414,.T.);
#10268=EDGE_CURVE('',#7967,#7968,#4693,.T.);
#10269=EDGE_CURVE('',#7967,#7965,#6415,.T.);
#10270=EDGE_CURVE('',#7966,#7968,#6416,.T.);
#10271=EDGE_CURVE('',#7969,#7970,#4694,.T.);
#10272=EDGE_CURVE('',#7969,#7967,#6417,.T.);
#10273=EDGE_CURVE('',#7968,#7970,#6418,.T.);
#10274=EDGE_CURVE('',#7971,#7972,#4695,.T.);
#10275=EDGE_CURVE('',#7971,#7969,#6419,.T.);
#10276=EDGE_CURVE('',#7970,#7972,#6420,.T.);
#10277=EDGE_CURVE('',#7973,#7974,#4696,.T.);
#10278=EDGE_CURVE('',#7973,#7971,#6421,.T.);
#10279=EDGE_CURVE('',#7972,#7974,#6422,.T.);
#10280=EDGE_CURVE('',#7975,#7976,#4697,.T.);
#10281=EDGE_CURVE('',#7975,#7973,#6423,.T.);
#10282=EDGE_CURVE('',#7974,#7976,#6424,.T.);
#10283=EDGE_CURVE('',#7977,#7978,#4698,.T.);
#10284=EDGE_CURVE('',#7977,#7975,#6425,.T.);
#10285=EDGE_CURVE('',#7976,#7978,#6426,.T.);
#10286=EDGE_CURVE('',#7979,#7980,#4699,.T.);
#10287=EDGE_CURVE('',#7979,#7977,#6427,.T.);
#10288=EDGE_CURVE('',#7978,#7980,#6428,.T.);
#10289=EDGE_CURVE('',#7981,#7982,#4700,.T.);
#10290=EDGE_CURVE('',#7981,#7979,#6429,.T.);
#10291=EDGE_CURVE('',#7980,#7982,#6430,.T.);
#10292=EDGE_CURVE('',#7983,#7984,#4701,.T.);
#10293=EDGE_CURVE('',#7983,#7981,#6431,.T.);
#10294=EDGE_CURVE('',#7982,#7984,#6432,.T.);
#10295=EDGE_CURVE('',#7985,#7986,#4702,.T.);
#10296=EDGE_CURVE('',#7985,#7983,#6433,.T.);
#10297=EDGE_CURVE('',#7984,#7986,#6434,.T.);
#10298=EDGE_CURVE('',#7987,#7988,#4703,.T.);
#10299=EDGE_CURVE('',#7987,#7985,#6435,.T.);
#10300=EDGE_CURVE('',#7986,#7988,#6436,.T.);
#10301=EDGE_CURVE('',#7989,#7990,#4704,.T.);
#10302=EDGE_CURVE('',#7989,#7987,#6437,.T.);
#10303=EDGE_CURVE('',#7988,#7990,#6438,.T.);
#10304=EDGE_CURVE('',#7991,#7992,#4705,.T.);
#10305=EDGE_CURVE('',#7991,#7989,#6439,.T.);
#10306=EDGE_CURVE('',#7990,#7992,#6440,.T.);
#10307=EDGE_CURVE('',#7993,#7994,#4706,.T.);
#10308=EDGE_CURVE('',#7993,#7991,#6441,.T.);
#10309=EDGE_CURVE('',#7992,#7994,#6442,.T.);
#10310=EDGE_CURVE('',#7995,#7996,#4707,.T.);
#10311=EDGE_CURVE('',#7995,#7993,#6443,.T.);
#10312=EDGE_CURVE('',#7994,#7996,#6444,.T.);
#10313=EDGE_CURVE('',#7997,#7998,#4708,.T.);
#10314=EDGE_CURVE('',#7997,#7995,#6445,.T.);
#10315=EDGE_CURVE('',#7996,#7998,#6446,.T.);
#10316=EDGE_CURVE('',#7999,#8000,#4709,.T.);
#10317=EDGE_CURVE('',#7999,#7997,#6447,.T.);
#10318=EDGE_CURVE('',#7998,#8000,#6448,.T.);
#10319=EDGE_CURVE('',#8001,#8002,#4710,.T.);
#10320=EDGE_CURVE('',#8001,#7999,#6449,.T.);
#10321=EDGE_CURVE('',#8000,#8002,#6450,.T.);
#10322=EDGE_CURVE('',#8003,#8004,#4711,.T.);
#10323=EDGE_CURVE('',#8003,#8001,#6451,.T.);
#10324=EDGE_CURVE('',#8002,#8004,#6452,.T.);
#10325=EDGE_CURVE('',#8005,#8006,#4712,.T.);
#10326=EDGE_CURVE('',#8005,#8003,#6453,.T.);
#10327=EDGE_CURVE('',#8004,#8006,#6454,.T.);
#10328=EDGE_CURVE('',#8007,#8008,#4713,.T.);
#10329=EDGE_CURVE('',#8007,#8005,#6455,.T.);
#10330=EDGE_CURVE('',#8006,#8008,#6456,.T.);
#10331=EDGE_CURVE('',#8009,#8010,#4714,.T.);
#10332=EDGE_CURVE('',#8009,#8007,#6457,.T.);
#10333=EDGE_CURVE('',#8008,#8010,#6458,.T.);
#10334=EDGE_CURVE('',#8011,#8012,#4715,.T.);
#10335=EDGE_CURVE('',#8011,#8009,#6459,.T.);
#10336=EDGE_CURVE('',#8010,#8012,#6460,.T.);
#10337=EDGE_CURVE('',#8013,#8014,#4716,.T.);
#10338=EDGE_CURVE('',#8013,#8011,#6461,.T.);
#10339=EDGE_CURVE('',#8012,#8014,#6462,.T.);
#10340=EDGE_CURVE('',#8015,#8016,#4717,.T.);
#10341=EDGE_CURVE('',#8015,#8013,#6463,.T.);
#10342=EDGE_CURVE('',#8014,#8016,#6464,.T.);
#10343=EDGE_CURVE('',#8017,#8018,#4718,.T.);
#10344=EDGE_CURVE('',#8017,#8015,#6465,.T.);
#10345=EDGE_CURVE('',#8016,#8018,#6466,.T.);
#10346=EDGE_CURVE('',#8019,#8020,#4719,.T.);
#10347=EDGE_CURVE('',#8019,#8017,#6467,.T.);
#10348=EDGE_CURVE('',#8018,#8020,#6468,.T.);
#10349=EDGE_CURVE('',#8021,#8022,#4720,.T.);
#10350=EDGE_CURVE('',#8021,#8019,#6469,.T.);
#10351=EDGE_CURVE('',#8020,#8022,#6470,.T.);
#10352=EDGE_CURVE('',#8023,#8024,#4721,.T.);
#10353=EDGE_CURVE('',#8023,#8021,#6471,.T.);
#10354=EDGE_CURVE('',#8022,#8024,#6472,.T.);
#10355=EDGE_CURVE('',#8025,#8026,#4722,.T.);
#10356=EDGE_CURVE('',#8025,#8023,#6473,.T.);
#10357=EDGE_CURVE('',#8024,#8026,#6474,.T.);
#10358=EDGE_CURVE('',#8027,#8028,#4723,.T.);
#10359=EDGE_CURVE('',#8027,#8025,#6475,.T.);
#10360=EDGE_CURVE('',#8026,#8028,#6476,.T.);
#10361=EDGE_CURVE('',#8029,#8030,#4724,.T.);
#10362=EDGE_CURVE('',#8029,#8027,#6477,.T.);
#10363=EDGE_CURVE('',#8028,#8030,#6478,.T.);
#10364=EDGE_CURVE('',#8031,#8032,#4725,.T.);
#10365=EDGE_CURVE('',#8031,#8029,#6479,.T.);
#10366=EDGE_CURVE('',#8030,#8032,#6480,.T.);
#10367=EDGE_CURVE('',#8033,#8034,#4726,.T.);
#10368=EDGE_CURVE('',#8033,#8031,#6481,.T.);
#10369=EDGE_CURVE('',#8032,#8034,#6482,.T.);
#10370=EDGE_CURVE('',#8035,#8036,#4727,.T.);
#10371=EDGE_CURVE('',#8035,#8033,#6483,.T.);
#10372=EDGE_CURVE('',#8034,#8036,#6484,.T.);
#10373=EDGE_CURVE('',#8037,#8038,#4728,.T.);
#10374=EDGE_CURVE('',#8037,#8035,#6485,.T.);
#10375=EDGE_CURVE('',#8036,#8038,#6486,.T.);
#10376=EDGE_CURVE('',#8039,#8040,#4729,.T.);
#10377=EDGE_CURVE('',#8039,#8037,#6487,.T.);
#10378=EDGE_CURVE('',#8038,#8040,#6488,.T.);
#10379=EDGE_CURVE('',#8041,#8042,#4730,.T.);
#10380=EDGE_CURVE('',#8041,#8043,#6489,.T.);
#10381=EDGE_CURVE('',#8042,#8043,#1206,.T.);
#10382=EDGE_CURVE('',#8044,#8045,#4731,.T.);
#10383=EDGE_CURVE('',#8044,#8041,#6490,.T.);
#10384=EDGE_CURVE('',#8046,#8042,#1207,.T.);
#10385=EDGE_CURVE('',#8045,#8046,#6491,.T.);
#10386=EDGE_CURVE('',#8047,#8048,#4732,.T.);
#10387=EDGE_CURVE('',#8047,#8044,#6492,.T.);
#10388=EDGE_CURVE('',#8048,#8045,#6493,.T.);
#10389=EDGE_CURVE('',#8049,#8050,#4733,.T.);
#10390=EDGE_CURVE('',#8049,#8047,#6494,.T.);
#10391=EDGE_CURVE('',#8050,#8048,#6495,.T.);
#10392=EDGE_CURVE('',#8051,#8052,#4734,.T.);
#10393=EDGE_CURVE('',#8051,#8049,#6496,.T.);
#10394=EDGE_CURVE('',#8052,#8050,#6497,.T.);
#10395=EDGE_CURVE('',#8053,#8054,#4735,.T.);
#10396=EDGE_CURVE('',#8053,#8051,#6498,.T.);
#10397=EDGE_CURVE('',#8054,#8052,#6499,.T.);
#10398=EDGE_CURVE('',#8055,#8056,#4736,.T.);
#10399=EDGE_CURVE('',#8055,#8053,#6500,.T.);
#10400=EDGE_CURVE('',#8056,#8054,#6501,.T.);
#10401=EDGE_CURVE('',#8057,#8058,#4737,.T.);
#10402=EDGE_CURVE('',#8057,#8055,#6502,.T.);
#10403=EDGE_CURVE('',#8058,#8056,#6503,.T.);
#10404=EDGE_CURVE('',#8059,#8060,#4738,.T.);
#10405=EDGE_CURVE('',#8059,#8057,#6504,.T.);
#10406=EDGE_CURVE('',#8060,#8058,#6505,.T.);
#10407=EDGE_CURVE('',#8061,#8062,#4739,.T.);
#10408=EDGE_CURVE('',#8061,#8059,#6506,.T.);
#10409=EDGE_CURVE('',#8062,#8060,#6507,.T.);
#10410=EDGE_CURVE('',#8063,#8064,#4740,.T.);
#10411=EDGE_CURVE('',#8063,#8061,#6508,.T.);
#10412=EDGE_CURVE('',#8064,#8062,#6509,.T.);
#10413=EDGE_CURVE('',#8065,#8066,#4741,.T.);
#10414=EDGE_CURVE('',#8065,#8063,#6510,.T.);
#10415=EDGE_CURVE('',#8066,#8064,#6511,.T.);
#10416=EDGE_CURVE('',#8067,#8068,#4742,.T.);
#10417=EDGE_CURVE('',#8067,#8065,#6512,.T.);
#10418=EDGE_CURVE('',#8068,#8066,#6513,.T.);
#10419=EDGE_CURVE('',#8069,#8070,#4743,.T.);
#10420=EDGE_CURVE('',#8069,#8067,#6514,.T.);
#10421=EDGE_CURVE('',#8070,#8068,#6515,.T.);
#10422=EDGE_CURVE('',#8071,#8072,#4744,.T.);
#10423=EDGE_CURVE('',#8071,#8069,#6516,.T.);
#10424=EDGE_CURVE('',#8072,#8070,#6517,.T.);
#10425=EDGE_CURVE('',#8073,#8074,#4745,.T.);
#10426=EDGE_CURVE('',#8073,#8071,#6518,.T.);
#10427=EDGE_CURVE('',#8074,#8072,#6519,.T.);
#10428=EDGE_CURVE('',#8075,#8076,#4746,.T.);
#10429=EDGE_CURVE('',#8075,#8073,#6520,.T.);
#10430=EDGE_CURVE('',#8076,#8074,#6521,.T.);
#10431=EDGE_CURVE('',#8077,#8078,#4747,.T.);
#10432=EDGE_CURVE('',#8077,#8075,#6522,.T.);
#10433=EDGE_CURVE('',#8078,#8076,#6523,.T.);
#10434=EDGE_CURVE('',#8079,#8080,#4748,.T.);
#10435=EDGE_CURVE('',#8079,#8077,#6524,.T.);
#10436=EDGE_CURVE('',#8080,#8078,#6525,.T.);
#10437=EDGE_CURVE('',#8081,#8082,#4749,.T.);
#10438=EDGE_CURVE('',#8081,#8079,#6526,.T.);
#10439=EDGE_CURVE('',#8082,#8080,#6527,.T.);
#10440=EDGE_CURVE('',#8083,#8084,#4750,.T.);
#10441=EDGE_CURVE('',#8083,#8081,#6528,.T.);
#10442=EDGE_CURVE('',#8084,#8082,#6529,.T.);
#10443=EDGE_CURVE('',#8085,#8086,#4751,.T.);
#10444=EDGE_CURVE('',#8085,#8083,#6530,.T.);
#10445=EDGE_CURVE('',#8086,#8084,#6531,.T.);
#10446=EDGE_CURVE('',#8087,#8088,#4752,.T.);
#10447=EDGE_CURVE('',#8087,#8085,#6532,.T.);
#10448=EDGE_CURVE('',#8088,#8086,#6533,.T.);
#10449=EDGE_CURVE('',#8089,#8090,#4753,.T.);
#10450=EDGE_CURVE('',#8089,#8087,#6534,.T.);
#10451=EDGE_CURVE('',#8090,#8088,#6535,.T.);
#10452=EDGE_CURVE('',#8091,#8092,#4754,.T.);
#10453=EDGE_CURVE('',#8091,#8089,#6536,.T.);
#10454=EDGE_CURVE('',#8092,#8090,#6537,.T.);
#10455=EDGE_CURVE('',#8093,#8094,#4755,.T.);
#10456=EDGE_CURVE('',#8093,#8091,#6538,.T.);
#10457=EDGE_CURVE('',#8094,#8092,#6539,.T.);
#10458=EDGE_CURVE('',#8095,#8096,#4756,.T.);
#10459=EDGE_CURVE('',#8095,#8093,#6540,.T.);
#10460=EDGE_CURVE('',#8096,#8094,#6541,.T.);
#10461=EDGE_CURVE('',#8097,#8098,#4757,.T.);
#10462=EDGE_CURVE('',#8097,#8095,#6542,.T.);
#10463=EDGE_CURVE('',#8098,#8096,#6543,.T.);
#10464=EDGE_CURVE('',#8099,#8100,#4758,.T.);
#10465=EDGE_CURVE('',#8099,#8097,#6544,.T.);
#10466=EDGE_CURVE('',#8100,#8098,#6545,.T.);
#10467=EDGE_CURVE('',#8101,#8102,#4759,.T.);
#10468=EDGE_CURVE('',#8101,#8099,#6546,.T.);
#10469=EDGE_CURVE('',#8102,#8100,#6547,.T.);
#10470=EDGE_CURVE('',#8103,#8104,#4760,.T.);
#10471=EDGE_CURVE('',#8103,#8101,#6548,.T.);
#10472=EDGE_CURVE('',#8104,#8102,#6549,.T.);
#10473=EDGE_CURVE('',#8105,#8106,#4761,.T.);
#10474=EDGE_CURVE('',#8105,#8103,#6550,.T.);
#10475=EDGE_CURVE('',#8106,#8104,#6551,.T.);
#10476=EDGE_CURVE('',#8107,#8108,#4762,.T.);
#10477=EDGE_CURVE('',#8107,#8105,#6552,.T.);
#10478=EDGE_CURVE('',#8108,#8106,#6553,.T.);
#10479=EDGE_CURVE('',#8109,#8110,#4763,.T.);
#10480=EDGE_CURVE('',#8109,#8107,#6554,.T.);
#10481=EDGE_CURVE('',#8110,#8108,#6555,.T.);
#10482=EDGE_CURVE('',#8111,#8112,#4764,.T.);
#10483=EDGE_CURVE('',#8111,#8109,#6556,.T.);
#10484=EDGE_CURVE('',#8112,#8110,#6557,.T.);
#10485=EDGE_CURVE('',#8113,#8114,#4765,.T.);
#10486=EDGE_CURVE('',#8113,#8111,#6558,.T.);
#10487=EDGE_CURVE('',#8114,#8112,#6559,.T.);
#10488=EDGE_CURVE('',#8115,#8116,#4766,.T.);
#10489=EDGE_CURVE('',#8115,#8113,#6560,.T.);
#10490=EDGE_CURVE('',#8116,#8114,#6561,.T.);
#10491=EDGE_CURVE('',#8117,#8118,#4767,.T.);
#10492=EDGE_CURVE('',#8117,#8115,#6562,.T.);
#10493=EDGE_CURVE('',#8118,#8116,#6563,.T.);
#10494=EDGE_CURVE('',#8119,#8120,#4768,.T.);
#10495=EDGE_CURVE('',#8119,#8117,#6564,.T.);
#10496=EDGE_CURVE('',#8120,#8118,#6565,.T.);
#10497=EDGE_CURVE('',#8121,#8122,#4769,.T.);
#10498=EDGE_CURVE('',#8121,#8119,#6566,.T.);
#10499=EDGE_CURVE('',#8122,#8120,#6567,.T.);
#10500=EDGE_CURVE('',#8123,#8124,#4770,.T.);
#10501=EDGE_CURVE('',#8123,#8121,#6568,.T.);
#10502=EDGE_CURVE('',#8124,#8122,#6569,.T.);
#10503=EDGE_CURVE('',#8125,#8126,#4771,.T.);
#10504=EDGE_CURVE('',#8125,#8123,#6570,.T.);
#10505=EDGE_CURVE('',#8126,#8124,#6571,.T.);
#10506=EDGE_CURVE('',#8127,#8128,#4772,.T.);
#10507=EDGE_CURVE('',#8127,#8125,#6572,.T.);
#10508=EDGE_CURVE('',#8128,#8126,#6573,.T.);
#10509=EDGE_CURVE('',#8129,#8130,#4773,.T.);
#10510=EDGE_CURVE('',#8129,#8127,#6574,.T.);
#10511=EDGE_CURVE('',#8130,#8128,#6575,.T.);
#10512=EDGE_CURVE('',#8131,#8132,#4774,.T.);
#10513=EDGE_CURVE('',#8131,#8129,#6576,.T.);
#10514=EDGE_CURVE('',#8132,#8130,#6577,.T.);
#10515=EDGE_CURVE('',#8133,#8134,#4775,.T.);
#10516=EDGE_CURVE('',#8133,#8131,#6578,.T.);
#10517=EDGE_CURVE('',#8134,#8132,#6579,.T.);
#10518=EDGE_CURVE('',#8135,#8136,#4776,.T.);
#10519=EDGE_CURVE('',#8135,#8133,#6580,.T.);
#10520=EDGE_CURVE('',#8136,#8134,#6581,.T.);
#10521=EDGE_CURVE('',#8137,#8138,#4777,.T.);
#10522=EDGE_CURVE('',#8137,#8135,#6582,.T.);
#10523=EDGE_CURVE('',#8138,#8136,#6583,.T.);
#10524=EDGE_CURVE('',#8139,#8140,#4778,.T.);
#10525=EDGE_CURVE('',#8139,#8137,#6584,.T.);
#10526=EDGE_CURVE('',#8140,#8138,#6585,.T.);
#10527=EDGE_CURVE('',#8141,#8142,#4779,.T.);
#10528=EDGE_CURVE('',#8141,#8139,#6586,.T.);
#10529=EDGE_CURVE('',#8142,#8140,#6587,.T.);
#10530=EDGE_CURVE('',#8143,#8144,#4780,.T.);
#10531=EDGE_CURVE('',#8143,#8141,#6588,.T.);
#10532=EDGE_CURVE('',#8144,#8142,#6589,.T.);
#10533=EDGE_CURVE('',#8145,#8146,#4781,.T.);
#10534=EDGE_CURVE('',#8145,#8143,#6590,.T.);
#10535=EDGE_CURVE('',#8146,#8144,#6591,.T.);
#10536=EDGE_CURVE('',#8147,#8148,#4782,.T.);
#10537=EDGE_CURVE('',#8147,#8145,#6592,.T.);
#10538=EDGE_CURVE('',#8148,#8146,#6593,.T.);
#10539=EDGE_CURVE('',#8149,#8150,#4783,.T.);
#10540=EDGE_CURVE('',#8149,#8147,#6594,.T.);
#10541=EDGE_CURVE('',#8150,#8148,#6595,.T.);
#10542=EDGE_CURVE('',#8151,#8152,#4784,.T.);
#10543=EDGE_CURVE('',#8151,#8149,#6596,.T.);
#10544=EDGE_CURVE('',#8152,#8150,#6597,.T.);
#10545=EDGE_CURVE('',#8153,#8154,#4785,.T.);
#10546=EDGE_CURVE('',#8153,#8151,#6598,.T.);
#10547=EDGE_CURVE('',#8154,#8152,#6599,.T.);
#10548=EDGE_CURVE('',#8155,#8156,#4786,.T.);
#10549=EDGE_CURVE('',#8155,#8153,#6600,.T.);
#10550=EDGE_CURVE('',#8156,#8154,#6601,.T.);
#10551=EDGE_CURVE('',#8157,#8158,#4787,.T.);
#10552=EDGE_CURVE('',#8157,#8155,#6602,.T.);
#10553=EDGE_CURVE('',#8158,#8156,#6603,.T.);
#10554=EDGE_CURVE('',#8159,#8160,#4788,.T.);
#10555=EDGE_CURVE('',#8159,#8157,#6604,.T.);
#10556=EDGE_CURVE('',#8160,#8158,#6605,.T.);
#10557=EDGE_CURVE('',#8161,#8162,#4789,.T.);
#10558=EDGE_CURVE('',#8161,#8159,#6606,.T.);
#10559=EDGE_CURVE('',#8162,#8160,#6607,.T.);
#10560=EDGE_CURVE('',#8163,#8164,#4790,.T.);
#10561=EDGE_CURVE('',#8163,#8161,#6608,.T.);
#10562=EDGE_CURVE('',#8164,#8162,#6609,.T.);
#10563=EDGE_CURVE('',#8165,#8166,#4791,.T.);
#10564=EDGE_CURVE('',#8165,#8163,#6610,.T.);
#10565=EDGE_CURVE('',#8166,#8164,#6611,.T.);
#10566=EDGE_CURVE('',#8167,#8168,#4792,.T.);
#10567=EDGE_CURVE('',#8167,#8165,#6612,.T.);
#10568=EDGE_CURVE('',#8168,#8166,#6613,.T.);
#10569=EDGE_CURVE('',#8169,#8170,#4793,.T.);
#10570=EDGE_CURVE('',#8169,#8167,#6614,.T.);
#10571=EDGE_CURVE('',#8170,#8168,#6615,.T.);
#10572=EDGE_CURVE('',#8171,#8172,#4794,.T.);
#10573=EDGE_CURVE('',#8171,#8169,#6616,.T.);
#10574=EDGE_CURVE('',#8172,#8170,#6617,.T.);
#10575=EDGE_CURVE('',#8173,#8174,#4795,.T.);
#10576=EDGE_CURVE('',#8173,#8171,#6618,.T.);
#10577=EDGE_CURVE('',#8174,#8172,#6619,.T.);
#10578=EDGE_CURVE('',#8175,#8176,#4796,.T.);
#10579=EDGE_CURVE('',#8175,#8173,#6620,.T.);
#10580=EDGE_CURVE('',#8176,#8174,#6621,.T.);
#10581=EDGE_CURVE('',#8177,#8178,#4797,.T.);
#10582=EDGE_CURVE('',#8177,#8175,#6622,.T.);
#10583=EDGE_CURVE('',#8178,#8176,#6623,.T.);
#10584=EDGE_CURVE('',#8179,#8180,#4798,.T.);
#10585=EDGE_CURVE('',#8179,#8177,#6624,.T.);
#10586=EDGE_CURVE('',#8180,#8178,#6625,.T.);
#10587=EDGE_CURVE('',#8181,#8182,#4799,.T.);
#10588=EDGE_CURVE('',#8181,#8179,#6626,.T.);
#10589=EDGE_CURVE('',#8182,#8180,#6627,.T.);
#10590=EDGE_CURVE('',#8183,#8184,#4800,.T.);
#10591=EDGE_CURVE('',#8183,#8181,#6628,.T.);
#10592=EDGE_CURVE('',#8184,#8182,#6629,.T.);
#10593=EDGE_CURVE('',#8185,#8186,#4801,.T.);
#10594=EDGE_CURVE('',#8185,#8183,#6630,.T.);
#10595=EDGE_CURVE('',#8186,#8184,#6631,.T.);
#10596=EDGE_CURVE('',#8187,#8188,#4802,.T.);
#10597=EDGE_CURVE('',#8187,#8185,#6632,.T.);
#10598=EDGE_CURVE('',#8188,#8186,#6633,.T.);
#10599=EDGE_CURVE('',#8189,#8190,#4803,.T.);
#10600=EDGE_CURVE('',#8189,#8187,#6634,.T.);
#10601=EDGE_CURVE('',#8190,#8188,#6635,.T.);
#10602=EDGE_CURVE('',#8191,#8192,#4804,.T.);
#10603=EDGE_CURVE('',#8191,#8189,#6636,.T.);
#10604=EDGE_CURVE('',#8192,#8190,#6637,.T.);
#10605=EDGE_CURVE('',#8193,#8194,#4805,.T.);
#10606=EDGE_CURVE('',#8193,#8191,#6638,.T.);
#10607=EDGE_CURVE('',#8194,#8192,#6639,.T.);
#10608=EDGE_CURVE('',#8195,#8196,#4806,.T.);
#10609=EDGE_CURVE('',#8195,#8193,#6640,.T.);
#10610=EDGE_CURVE('',#8196,#8194,#6641,.T.);
#10611=EDGE_CURVE('',#8197,#8198,#4807,.T.);
#10612=EDGE_CURVE('',#8197,#8195,#6642,.T.);
#10613=EDGE_CURVE('',#8198,#8196,#6643,.T.);
#10614=EDGE_CURVE('',#8199,#8200,#4808,.T.);
#10615=EDGE_CURVE('',#8199,#8197,#6644,.T.);
#10616=EDGE_CURVE('',#8200,#8198,#6645,.T.);
#10617=EDGE_CURVE('',#8201,#8202,#4809,.T.);
#10618=EDGE_CURVE('',#8201,#8199,#6646,.T.);
#10619=EDGE_CURVE('',#8202,#8200,#6647,.T.);
#10620=EDGE_CURVE('',#8203,#8204,#4810,.T.);
#10621=EDGE_CURVE('',#8203,#8201,#6648,.T.);
#10622=EDGE_CURVE('',#8204,#8202,#6649,.T.);
#10623=EDGE_CURVE('',#8205,#8206,#4811,.T.);
#10624=EDGE_CURVE('',#8205,#8203,#6650,.T.);
#10625=EDGE_CURVE('',#8206,#8204,#6651,.T.);
#10626=EDGE_CURVE('',#8207,#8208,#4812,.T.);
#10627=EDGE_CURVE('',#8207,#8205,#6652,.T.);
#10628=EDGE_CURVE('',#8208,#8206,#6653,.T.);
#10629=EDGE_CURVE('',#8209,#8210,#4813,.T.);
#10630=EDGE_CURVE('',#8209,#8207,#6654,.T.);
#10631=EDGE_CURVE('',#8210,#8208,#6655,.T.);
#10632=EDGE_CURVE('',#8211,#8212,#4814,.T.);
#10633=EDGE_CURVE('',#8211,#8209,#6656,.T.);
#10634=EDGE_CURVE('',#8212,#8210,#6657,.T.);
#10635=EDGE_CURVE('',#8213,#8214,#4815,.T.);
#10636=EDGE_CURVE('',#8213,#8211,#6658,.T.);
#10637=EDGE_CURVE('',#8214,#8212,#6659,.T.);
#10638=EDGE_CURVE('',#8215,#8216,#4816,.T.);
#10639=EDGE_CURVE('',#8215,#8213,#6660,.T.);
#10640=EDGE_CURVE('',#8216,#8214,#6661,.T.);
#10641=EDGE_CURVE('',#8217,#8218,#4817,.T.);
#10642=EDGE_CURVE('',#8217,#8215,#6662,.T.);
#10643=EDGE_CURVE('',#8218,#8216,#6663,.T.);
#10644=EDGE_CURVE('',#8219,#8046,#6664,.T.);
#10645=EDGE_CURVE('',#8040,#8219,#6665,.T.);
#10646=EDGE_CURVE('',#8220,#7866,#6666,.T.);
#10647=EDGE_CURVE('',#8220,#8218,#6667,.T.);
#10648=EDGE_CURVE('',#7866,#8221,#1208,.T.);
#10649=EDGE_CURVE('',#8221,#7865,#1209,.T.);
#10650=EDGE_CURVE('',#7865,#8222,#6668,.T.);
#10651=EDGE_CURVE('',#8222,#8220,#1210,.T.);
#10652=EDGE_CURVE('',#8222,#8217,#6669,.T.);
#10653=EDGE_CURVE('',#8043,#8223,#6670,.T.);
#10654=EDGE_CURVE('',#8223,#8039,#6671,.T.);
#10655=EDGE_CURVE('',#8224,#8225,#1785,.T.);
#10656=EDGE_CURVE('',#8226,#8224,#1786,.T.);
#10657=EDGE_CURVE('',#8227,#8226,#1787,.T.);
#10658=EDGE_CURVE('',#8228,#8227,#1788,.T.);
#10659=EDGE_CURVE('',#8229,#8228,#1789,.T.);
#10660=EDGE_CURVE('',#8229,#8230,#4818,.T.);
#10661=EDGE_CURVE('',#8230,#8230,#1211,.T.);
#10662=EDGE_CURVE('',#8231,#8229,#1790,.T.);
#10663=EDGE_CURVE('',#8225,#8231,#1791,.T.);
#10664=EDGE_CURVE('',#8232,#8227,#4819,.T.);
#10665=EDGE_CURVE('',#8232,#8233,#4820,.T.);
#10666=EDGE_CURVE('',#8233,#8228,#4821,.T.);
#10667=EDGE_CURVE('',#8234,#8226,#4822,.T.);
#10668=EDGE_CURVE('',#8234,#8232,#4823,.T.);
#10669=EDGE_CURVE('',#8235,#8224,#4824,.T.);
#10670=EDGE_CURVE('',#8235,#8234,#4825,.T.);
#10671=EDGE_CURVE('',#8236,#8235,#4826,.T.);
#10672=EDGE_CURVE('',#8237,#8236,#4827,.T.);
#10673=EDGE_CURVE('',#8233,#8237,#4828,.T.);
#10674=EDGE_CURVE('',#8223,#8219,#1212,.F.);
#10675=EDGE_CURVE('',#8236,#8225,#4829,.T.);
#10676=EDGE_CURVE('',#8237,#8231,#4830,.T.);
#10677=EDGE_CURVE('',#8238,#8238,#1213,.T.);
#10678=EDGE_CURVE('',#8221,#8238,#4831,.T.);
#10679=EDGE_CURVE('',#8239,#8239,#1214,.T.);
#10680=EDGE_CURVE('',#8239,#8240,#4832,.T.);
#10681=EDGE_CURVE('',#8240,#8241,#6672,.T.);
#10682=EDGE_CURVE('',#8241,#8242,#1215,.T.);
#10683=EDGE_CURVE('',#8242,#8243,#6673,.T.);
#10684=EDGE_CURVE('',#8243,#8244,#1216,.T.);
#10685=EDGE_CURVE('',#8244,#8245,#6674,.T.);
#10686=EDGE_CURVE('',#8245,#8246,#1217,.T.);
#10687=EDGE_CURVE('',#8246,#8247,#6675,.T.);
#10688=EDGE_CURVE('',#8247,#8248,#1218,.T.);
#10689=EDGE_CURVE('',#8248,#8249,#6676,.T.);
#10690=EDGE_CURVE('',#8249,#8250,#1219,.T.);
#10691=EDGE_CURVE('',#8250,#8251,#6677,.T.);
#10692=EDGE_CURVE('',#8251,#8252,#1220,.T.);
#10693=EDGE_CURVE('',#8252,#8240,#6678,.T.);
#10694=EDGE_CURVE('',#8248,#8253,#6679,.T.);
#10695=EDGE_CURVE('',#8253,#8254,#6680,.F.);
#10696=EDGE_CURVE('',#8254,#8255,#6681,.T.);
#10697=EDGE_CURVE('',#8255,#8256,#6682,.F.);
#10698=EDGE_CURVE('',#8256,#8249,#6683,.T.);
#10699=EDGE_CURVE('',#8246,#8257,#6684,.T.);
#10700=EDGE_CURVE('',#8257,#8258,#6685,.F.);
#10701=EDGE_CURVE('',#8258,#8259,#6686,.T.);
#10702=EDGE_CURVE('',#8259,#8253,#6687,.F.);
#10703=EDGE_CURVE('',#8253,#8247,#6688,.T.);
#10704=EDGE_CURVE('',#8257,#8245,#6689,.T.);
#10705=EDGE_CURVE('',#8260,#8243,#6690,.T.);
#10706=EDGE_CURVE('',#8244,#8260,#6691,.T.);
#10707=EDGE_CURVE('',#8261,#8241,#6692,.T.);
#10708=EDGE_CURVE('',#8242,#8261,#6693,.T.);
#10709=EDGE_CURVE('',#8262,#8251,#6694,.T.);
#10710=EDGE_CURVE('',#8252,#8262,#6695,.T.);
#10711=EDGE_CURVE('',#8250,#8256,#6696,.T.);
#10712=EDGE_CURVE('',#8260,#8263,#6697,.F.);
#10713=EDGE_CURVE('',#8263,#8264,#6698,.T.);
#10714=EDGE_CURVE('',#8264,#8257,#6699,.F.);
#10715=EDGE_CURVE('',#8265,#8265,#1221,.T.);
#10716=EDGE_CURVE('',#8258,#8264,#4833,.T.);
#10717=EDGE_CURVE('',#8266,#8260,#6700,.F.);
#10718=EDGE_CURVE('',#8263,#8266,#4834,.T.);
#10719=EDGE_CURVE('',#8254,#8259,#4835,.T.);
#10720=EDGE_CURVE('',#8261,#8267,#6701,.F.);
#10721=EDGE_CURVE('',#8268,#8261,#6702,.F.);
#10722=EDGE_CURVE('',#8267,#8268,#4836,.T.);
#10723=EDGE_CURVE('',#8269,#8255,#4837,.T.);
#10724=EDGE_CURVE('',#8256,#8269,#6703,.F.);
#10725=EDGE_CURVE('',#8262,#8270,#6704,.F.);
#10726=EDGE_CURVE('',#8271,#8262,#6705,.F.);
#10727=EDGE_CURVE('',#8270,#8271,#4838,.T.);
#10728=EDGE_CURVE('',#8269,#8271,#6706,.T.);
#10729=EDGE_CURVE('',#8272,#8273,#1792,.T.);
#10730=EDGE_CURVE('',#8273,#8270,#4839,.T.);
#10731=EDGE_CURVE('',#8271,#8272,#4840,.T.);
#10732=EDGE_CURVE('',#8270,#8268,#6707,.T.);
#10733=EDGE_CURVE('',#8274,#8275,#1793,.T.);
#10734=EDGE_CURVE('',#8275,#8269,#4841,.T.);
#10735=EDGE_CURVE('',#8255,#8274,#4842,.T.);
#10736=EDGE_CURVE('',#8276,#8277,#1794,.T.);
#10737=EDGE_CURVE('',#8277,#8267,#4843,.T.);
#10738=EDGE_CURVE('',#8268,#8276,#4844,.T.);
#10739=EDGE_CURVE('',#8267,#8266,#6708,.T.);
#10740=EDGE_CURVE('',#8278,#8279,#1795,.T.);
#10741=EDGE_CURVE('',#8279,#8254,#4845,.T.);
#10742=EDGE_CURVE('',#8259,#8278,#4846,.T.);
#10743=EDGE_CURVE('',#8280,#8281,#1796,.T.);
#10744=EDGE_CURVE('',#8281,#8263,#4847,.T.);
#10745=EDGE_CURVE('',#8266,#8280,#4848,.T.);
#10746=EDGE_CURVE('',#8282,#8283,#1797,.T.);
#10747=EDGE_CURVE('',#8283,#8258,#4849,.T.);
#10748=EDGE_CURVE('',#8264,#8282,#4850,.T.);
#10749=EDGE_CURVE('',#8279,#8274,#1798,.T.);
#10750=EDGE_CURVE('',#8283,#8278,#1799,.T.);
#10751=EDGE_CURVE('',#8281,#8282,#1800,.T.);
#10752=EDGE_CURVE('',#8284,#8284,#1222,.T.);
#10753=EDGE_CURVE('',#8284,#8285,#4851,.T.);
#10754=EDGE_CURVE('',#8273,#8285,#1801,.T.);
#10755=EDGE_CURVE('',#8275,#8272,#1802,.T.);
#10756=EDGE_CURVE('',#8277,#8280,#1803,.T.);
#10757=EDGE_CURVE('',#8285,#8276,#1804,.T.);
#10758=EDGE_CURVE('',#8286,#8286,#1223,.T.);
#10759=EDGE_CURVE('',#8286,#8287,#4852,.T.);
#10760=EDGE_CURVE('',#8287,#8287,#1224,.T.);
#10761=EDGE_CURVE('',#8287,#8288,#4853,.T.);
#10762=EDGE_CURVE('',#8288,#8288,#1225,.T.);
#10763=EDGE_CURVE('',#8288,#8265,#4854,.T.);
#10764=ORIENTED_EDGE('',*,*,#8289,.T.);
#10765=ORIENTED_EDGE('',*,*,#8290,.T.);
#10766=ORIENTED_EDGE('',*,*,#8291,.T.);
#10767=ORIENTED_EDGE('',*,*,#8292,.T.);
#10768=ORIENTED_EDGE('',*,*,#8293,.T.);
#10769=ORIENTED_EDGE('',*,*,#8290,.F.);
#10770=ORIENTED_EDGE('',*,*,#8294,.T.);
#10771=ORIENTED_EDGE('',*,*,#8295,.T.);
#10772=ORIENTED_EDGE('',*,*,#8296,.T.);
#10773=ORIENTED_EDGE('',*,*,#8297,.F.);
#10774=ORIENTED_EDGE('',*,*,#8298,.F.);
#10775=ORIENTED_EDGE('',*,*,#8299,.T.);
#10776=ORIENTED_EDGE('',*,*,#8300,.F.);
#10777=ORIENTED_EDGE('',*,*,#8301,.F.);
#10778=ORIENTED_EDGE('',*,*,#8302,.T.);
#10779=ORIENTED_EDGE('',*,*,#8303,.T.);
#10780=ORIENTED_EDGE('',*,*,#8304,.T.);
#10781=ORIENTED_EDGE('',*,*,#8301,.T.);
#10782=ORIENTED_EDGE('',*,*,#8305,.F.);
#10783=ORIENTED_EDGE('',*,*,#8306,.T.);
#10784=ORIENTED_EDGE('',*,*,#8307,.F.);
#10785=ORIENTED_EDGE('',*,*,#8292,.F.);
#10786=ORIENTED_EDGE('',*,*,#8308,.T.);
#10787=ORIENTED_EDGE('',*,*,#8303,.F.);
#10788=ORIENTED_EDGE('',*,*,#8309,.F.);
#10789=ORIENTED_EDGE('',*,*,#8306,.F.);
#10790=ORIENTED_EDGE('',*,*,#8310,.T.);
#10791=ORIENTED_EDGE('',*,*,#8311,.T.);
#10792=ORIENTED_EDGE('',*,*,#8312,.T.);
#10793=ORIENTED_EDGE('',*,*,#8313,.T.);
#10794=ORIENTED_EDGE('',*,*,#8314,.T.);
#10795=ORIENTED_EDGE('',*,*,#8311,.F.);
#10796=ORIENTED_EDGE('',*,*,#8315,.T.);
#10797=ORIENTED_EDGE('',*,*,#8316,.T.);
#10798=ORIENTED_EDGE('',*,*,#8317,.T.);
#10799=ORIENTED_EDGE('',*,*,#8318,.F.);
#10800=ORIENTED_EDGE('',*,*,#8319,.F.);
#10801=ORIENTED_EDGE('',*,*,#8320,.T.);
#10802=ORIENTED_EDGE('',*,*,#8321,.F.);
#10803=ORIENTED_EDGE('',*,*,#8322,.F.);
#10804=ORIENTED_EDGE('',*,*,#8323,.T.);
#10805=ORIENTED_EDGE('',*,*,#8324,.T.);
#10806=ORIENTED_EDGE('',*,*,#8325,.T.);
#10807=ORIENTED_EDGE('',*,*,#8322,.T.);
#10808=ORIENTED_EDGE('',*,*,#8326,.F.);
#10809=ORIENTED_EDGE('',*,*,#8327,.T.);
#10810=ORIENTED_EDGE('',*,*,#8328,.F.);
#10811=ORIENTED_EDGE('',*,*,#8313,.F.);
#10812=ORIENTED_EDGE('',*,*,#8329,.T.);
#10813=ORIENTED_EDGE('',*,*,#8324,.F.);
#10814=ORIENTED_EDGE('',*,*,#8330,.F.);
#10815=ORIENTED_EDGE('',*,*,#8327,.F.);
#10816=ORIENTED_EDGE('',*,*,#8331,.T.);
#10817=ORIENTED_EDGE('',*,*,#8332,.T.);
#10818=ORIENTED_EDGE('',*,*,#8305,.T.);
#10819=ORIENTED_EDGE('',*,*,#8332,.F.);
#10820=ORIENTED_EDGE('',*,*,#8333,.F.);
#10821=ORIENTED_EDGE('',*,*,#8334,.F.);
#10822=ORIENTED_EDGE('',*,*,#8335,.F.);
#10823=ORIENTED_EDGE('',*,*,#8336,.F.);
#10824=ORIENTED_EDGE('',*,*,#8337,.F.);
#10825=ORIENTED_EDGE('',*,*,#8338,.F.);
#10826=ORIENTED_EDGE('',*,*,#8339,.F.);
#10827=ORIENTED_EDGE('',*,*,#8340,.F.);
#10828=ORIENTED_EDGE('',*,*,#8341,.F.);
#10829=ORIENTED_EDGE('',*,*,#8342,.T.);
#10830=ORIENTED_EDGE('',*,*,#8331,.F.);
#10831=ORIENTED_EDGE('',*,*,#8341,.T.);
#10832=ORIENTED_EDGE('',*,*,#8343,.T.);
#10833=ORIENTED_EDGE('',*,*,#8326,.T.);
#10834=ORIENTED_EDGE('',*,*,#8343,.F.);
#10835=ORIENTED_EDGE('',*,*,#8344,.T.);
#10836=ORIENTED_EDGE('',*,*,#8345,.T.);
#10837=ORIENTED_EDGE('',*,*,#8346,.T.);
#10838=ORIENTED_EDGE('',*,*,#8345,.F.);
#10839=ORIENTED_EDGE('',*,*,#8347,.F.);
#10840=ORIENTED_EDGE('',*,*,#8348,.F.);
#10841=ORIENTED_EDGE('',*,*,#8349,.F.);
#10842=ORIENTED_EDGE('',*,*,#8350,.F.);
#10843=ORIENTED_EDGE('',*,*,#8351,.F.);
#10844=ORIENTED_EDGE('',*,*,#8352,.F.);
#10845=ORIENTED_EDGE('',*,*,#8353,.F.);
#10846=ORIENTED_EDGE('',*,*,#8354,.F.);
#10847=ORIENTED_EDGE('',*,*,#8355,.F.);
#10848=ORIENTED_EDGE('',*,*,#8356,.T.);
#10849=ORIENTED_EDGE('',*,*,#8344,.F.);
#10850=ORIENTED_EDGE('',*,*,#8346,.F.);
#10851=ORIENTED_EDGE('',*,*,#8357,.T.);
#10852=ORIENTED_EDGE('',*,*,#8358,.T.);
#10853=ORIENTED_EDGE('',*,*,#8357,.F.);
#10854=ORIENTED_EDGE('',*,*,#8355,.T.);
#10855=ORIENTED_EDGE('',*,*,#8359,.T.);
#10856=ORIENTED_EDGE('',*,*,#8360,.T.);
#10857=ORIENTED_EDGE('',*,*,#8359,.F.);
#10858=ORIENTED_EDGE('',*,*,#8360,.F.);
#10859=ORIENTED_EDGE('',*,*,#8361,.T.);
#10860=ORIENTED_EDGE('',*,*,#8362,.T.);
#10861=ORIENTED_EDGE('',*,*,#8361,.F.);
#10862=ORIENTED_EDGE('',*,*,#8363,.T.);
#10863=ORIENTED_EDGE('',*,*,#8364,.T.);
#10864=ORIENTED_EDGE('',*,*,#8365,.T.);
#10865=ORIENTED_EDGE('',*,*,#8366,.T.);
#10866=ORIENTED_EDGE('',*,*,#8364,.F.);
#10867=ORIENTED_EDGE('',*,*,#8367,.T.);
#10868=ORIENTED_EDGE('',*,*,#8297,.T.);
#10869=ORIENTED_EDGE('',*,*,#8368,.T.);
#10870=ORIENTED_EDGE('',*,*,#8369,.T.);
#10871=ORIENTED_EDGE('',*,*,#8370,.T.);
#10872=ORIENTED_EDGE('',*,*,#8371,.T.);
#10873=ORIENTED_EDGE('',*,*,#8372,.T.);
#10874=ORIENTED_EDGE('',*,*,#8373,.T.);
#10875=ORIENTED_EDGE('',*,*,#8374,.T.);
#10876=ORIENTED_EDGE('',*,*,#8375,.T.);
#10877=ORIENTED_EDGE('',*,*,#8376,.T.);
#10878=ORIENTED_EDGE('',*,*,#8377,.T.);
#10879=ORIENTED_EDGE('',*,*,#8374,.F.);
#10880=ORIENTED_EDGE('',*,*,#8378,.T.);
#10881=ORIENTED_EDGE('',*,*,#8379,.T.);
#10882=ORIENTED_EDGE('',*,*,#8380,.T.);
#10883=ORIENTED_EDGE('',*,*,#8381,.T.);
#10884=ORIENTED_EDGE('',*,*,#8382,.T.);
#10885=ORIENTED_EDGE('',*,*,#8318,.T.);
#10886=ORIENTED_EDGE('',*,*,#8383,.T.);
#10887=ORIENTED_EDGE('',*,*,#8384,.T.);
#10888=ORIENTED_EDGE('',*,*,#8385,.T.);
#10889=ORIENTED_EDGE('',*,*,#8386,.T.);
#10890=ORIENTED_EDGE('',*,*,#8387,.T.);
#10891=ORIENTED_EDGE('',*,*,#8385,.F.);
#10892=ORIENTED_EDGE('',*,*,#8387,.F.);
#10893=ORIENTED_EDGE('',*,*,#8388,.T.);
#10894=ORIENTED_EDGE('',*,*,#8376,.F.);
#10895=ORIENTED_EDGE('',*,*,#8389,.T.);
#10896=ORIENTED_EDGE('',*,*,#8390,.T.);
#10897=ORIENTED_EDGE('',*,*,#8391,.T.);
#10898=ORIENTED_EDGE('',*,*,#8366,.F.);
#10899=ORIENTED_EDGE('',*,*,#8392,.T.);
#10900=ORIENTED_EDGE('',*,*,#8393,.T.);
#10901=ORIENTED_EDGE('',*,*,#8394,.T.);
#10902=ORIENTED_EDGE('',*,*,#8377,.F.);
#10903=ORIENTED_EDGE('',*,*,#8388,.F.);
#10904=ORIENTED_EDGE('',*,*,#8386,.F.);
#10905=ORIENTED_EDGE('',*,*,#8384,.F.);
#10906=ORIENTED_EDGE('',*,*,#8395,.T.);
#10907=ORIENTED_EDGE('',*,*,#8396,.T.);
#10908=ORIENTED_EDGE('',*,*,#8397,.T.);
#10909=ORIENTED_EDGE('',*,*,#8398,.T.);
#10910=ORIENTED_EDGE('',*,*,#8399,.T.);
#10911=ORIENTED_EDGE('',*,*,#8400,.T.);
#10912=ORIENTED_EDGE('',*,*,#8401,.T.);
#10913=ORIENTED_EDGE('',*,*,#8402,.T.);
#10914=ORIENTED_EDGE('',*,*,#8403,.T.);
#10915=ORIENTED_EDGE('',*,*,#8404,.T.);
#10916=ORIENTED_EDGE('',*,*,#8405,.T.);
#10917=ORIENTED_EDGE('',*,*,#8406,.T.);
#10918=ORIENTED_EDGE('',*,*,#8407,.T.);
#10919=ORIENTED_EDGE('',*,*,#8408,.T.);
#10920=ORIENTED_EDGE('',*,*,#8409,.T.);
#10921=ORIENTED_EDGE('',*,*,#8410,.T.);
#10922=ORIENTED_EDGE('',*,*,#8411,.T.);
#10923=ORIENTED_EDGE('',*,*,#8412,.T.);
#10924=ORIENTED_EDGE('',*,*,#8413,.T.);
#10925=ORIENTED_EDGE('',*,*,#8414,.T.);
#10926=ORIENTED_EDGE('',*,*,#8415,.T.);
#10927=ORIENTED_EDGE('',*,*,#8416,.T.);
#10928=ORIENTED_EDGE('',*,*,#8417,.T.);
#10929=ORIENTED_EDGE('',*,*,#8418,.T.);
#10930=ORIENTED_EDGE('',*,*,#8419,.T.);
#10931=ORIENTED_EDGE('',*,*,#8420,.F.);
#10932=ORIENTED_EDGE('',*,*,#8421,.T.);
#10933=ORIENTED_EDGE('',*,*,#8422,.F.);
#10934=ORIENTED_EDGE('',*,*,#8423,.T.);
#10935=ORIENTED_EDGE('',*,*,#8423,.F.);
#10936=ORIENTED_EDGE('',*,*,#8424,.F.);
#10937=ORIENTED_EDGE('',*,*,#8425,.T.);
#10938=ORIENTED_EDGE('',*,*,#8426,.T.);
#10939=ORIENTED_EDGE('',*,*,#8381,.F.);
#10940=ORIENTED_EDGE('',*,*,#8427,.T.);
#10941=ORIENTED_EDGE('',*,*,#8428,.T.);
#10942=ORIENTED_EDGE('',*,*,#8429,.F.);
#10943=ORIENTED_EDGE('',*,*,#8430,.T.);
#10944=ORIENTED_EDGE('',*,*,#8431,.T.);
#10945=ORIENTED_EDGE('',*,*,#8432,.T.);
#10946=ORIENTED_EDGE('',*,*,#8433,.T.);
#10947=ORIENTED_EDGE('',*,*,#8434,.T.);
#10948=ORIENTED_EDGE('',*,*,#8435,.T.);
#10949=ORIENTED_EDGE('',*,*,#8436,.T.);
#10950=ORIENTED_EDGE('',*,*,#8420,.T.);
#10951=ORIENTED_EDGE('',*,*,#8434,.F.);
#10952=ORIENTED_EDGE('',*,*,#8437,.F.);
#10953=ORIENTED_EDGE('',*,*,#8438,.T.);
#10954=ORIENTED_EDGE('',*,*,#8439,.T.);
#10955=ORIENTED_EDGE('',*,*,#8440,.T.);
#10956=ORIENTED_EDGE('',*,*,#8441,.T.);
#10957=ORIENTED_EDGE('',*,*,#8442,.F.);
#10958=ORIENTED_EDGE('',*,*,#8443,.T.);
#10959=ORIENTED_EDGE('',*,*,#8444,.T.);
#10960=ORIENTED_EDGE('',*,*,#8445,.T.);
#10961=ORIENTED_EDGE('',*,*,#8435,.F.);
#10962=ORIENTED_EDGE('',*,*,#8446,.T.);
#10963=ORIENTED_EDGE('',*,*,#8447,.F.);
#10964=ORIENTED_EDGE('',*,*,#8446,.F.);
#10965=ORIENTED_EDGE('',*,*,#8448,.F.);
#10966=ORIENTED_EDGE('',*,*,#8449,.F.);
#10967=ORIENTED_EDGE('',*,*,#8450,.F.);
#10968=ORIENTED_EDGE('',*,*,#8451,.T.);
#10969=ORIENTED_EDGE('',*,*,#8452,.T.);
#10970=ORIENTED_EDGE('',*,*,#8451,.F.);
#10971=ORIENTED_EDGE('',*,*,#8453,.T.);
#10972=ORIENTED_EDGE('',*,*,#8454,.T.);
#10973=ORIENTED_EDGE('',*,*,#8455,.T.);
#10974=ORIENTED_EDGE('',*,*,#8369,.F.);
#10975=ORIENTED_EDGE('',*,*,#8456,.T.);
#10976=ORIENTED_EDGE('',*,*,#8457,.T.);
#10977=ORIENTED_EDGE('',*,*,#8458,.T.);
#10978=ORIENTED_EDGE('',*,*,#8459,.T.);
#10979=ORIENTED_EDGE('',*,*,#8460,.T.);
#10980=ORIENTED_EDGE('',*,*,#8461,.T.);
#10981=ORIENTED_EDGE('',*,*,#8462,.T.);
#10982=ORIENTED_EDGE('',*,*,#8449,.T.);
#10983=ORIENTED_EDGE('',*,*,#8463,.T.);
#10984=ORIENTED_EDGE('',*,*,#8442,.T.);
#10985=ORIENTED_EDGE('',*,*,#8447,.T.);
#10986=ORIENTED_EDGE('',*,*,#8464,.T.);
#10987=ORIENTED_EDGE('',*,*,#8465,.T.);
#10988=ORIENTED_EDGE('',*,*,#8464,.F.);
#10989=ORIENTED_EDGE('',*,*,#8465,.F.);
#10990=ORIENTED_EDGE('',*,*,#8466,.T.);
#10991=ORIENTED_EDGE('',*,*,#8467,.T.);
#10992=ORIENTED_EDGE('',*,*,#8468,.T.);
#10993=ORIENTED_EDGE('',*,*,#8469,.T.);
#10994=ORIENTED_EDGE('',*,*,#8470,.T.);
#10995=ORIENTED_EDGE('',*,*,#8471,.T.);
#10996=ORIENTED_EDGE('',*,*,#8472,.F.);
#10997=ORIENTED_EDGE('',*,*,#8429,.T.);
#10998=ORIENTED_EDGE('',*,*,#8473,.T.);
#10999=ORIENTED_EDGE('',*,*,#8474,.T.);
#11000=ORIENTED_EDGE('',*,*,#8475,.T.);
#11001=ORIENTED_EDGE('',*,*,#8437,.T.);
#11002=ORIENTED_EDGE('',*,*,#8433,.F.);
#11003=ORIENTED_EDGE('',*,*,#8419,.F.);
#11004=ORIENTED_EDGE('',*,*,#8476,.T.);
#11005=ORIENTED_EDGE('',*,*,#8477,.T.);
#11006=ORIENTED_EDGE('',*,*,#8474,.F.);
#11007=ORIENTED_EDGE('',*,*,#8478,.T.);
#11008=ORIENTED_EDGE('',*,*,#8479,.T.);
#11009=ORIENTED_EDGE('',*,*,#8480,.T.);
#11010=ORIENTED_EDGE('',*,*,#8476,.F.);
#11011=ORIENTED_EDGE('',*,*,#8481,.T.);
#11012=ORIENTED_EDGE('',*,*,#8482,.T.);
#11013=ORIENTED_EDGE('',*,*,#8483,.T.);
#11014=ORIENTED_EDGE('',*,*,#8479,.F.);
#11015=ORIENTED_EDGE('',*,*,#8484,.T.);
#11016=ORIENTED_EDGE('',*,*,#8483,.F.);
#11017=ORIENTED_EDGE('',*,*,#8485,.F.);
#11018=ORIENTED_EDGE('',*,*,#8393,.F.);
#11019=ORIENTED_EDGE('',*,*,#8486,.T.);
#11020=ORIENTED_EDGE('',*,*,#8487,.F.);
#11021=ORIENTED_EDGE('',*,*,#8488,.T.);
#11022=ORIENTED_EDGE('',*,*,#8489,.F.);
#11023=ORIENTED_EDGE('',*,*,#8490,.F.);
#11024=ORIENTED_EDGE('',*,*,#8484,.F.);
#11025=ORIENTED_EDGE('',*,*,#8481,.F.);
#11026=ORIENTED_EDGE('',*,*,#8478,.F.);
#11027=ORIENTED_EDGE('',*,*,#8473,.F.);
#11028=ORIENTED_EDGE('',*,*,#8428,.F.);
#11029=ORIENTED_EDGE('',*,*,#8491,.F.);
#11030=ORIENTED_EDGE('',*,*,#8492,.F.);
#11031=ORIENTED_EDGE('',*,*,#8493,.F.);
#11032=ORIENTED_EDGE('',*,*,#8494,.T.);
#11033=ORIENTED_EDGE('',*,*,#8489,.T.);
#11034=ORIENTED_EDGE('',*,*,#8495,.T.);
#11035=ORIENTED_EDGE('',*,*,#8347,.T.);
#11036=ORIENTED_EDGE('',*,*,#8496,.T.);
#11037=ORIENTED_EDGE('',*,*,#8348,.T.);
#11038=ORIENTED_EDGE('',*,*,#8495,.F.);
#11039=ORIENTED_EDGE('',*,*,#8497,.T.);
#11040=ORIENTED_EDGE('',*,*,#8498,.T.);
#11041=ORIENTED_EDGE('',*,*,#8349,.T.);
#11042=ORIENTED_EDGE('',*,*,#8496,.F.);
#11043=ORIENTED_EDGE('',*,*,#8499,.T.);
#11044=ORIENTED_EDGE('',*,*,#8500,.T.);
#11045=ORIENTED_EDGE('',*,*,#8350,.T.);
#11046=ORIENTED_EDGE('',*,*,#8498,.F.);
#11047=ORIENTED_EDGE('',*,*,#8501,.T.);
#11048=ORIENTED_EDGE('',*,*,#8502,.T.);
#11049=ORIENTED_EDGE('',*,*,#8351,.T.);
#11050=ORIENTED_EDGE('',*,*,#8500,.F.);
#11051=ORIENTED_EDGE('',*,*,#8503,.T.);
#11052=ORIENTED_EDGE('',*,*,#8504,.T.);
#11053=ORIENTED_EDGE('',*,*,#8352,.T.);
#11054=ORIENTED_EDGE('',*,*,#8502,.F.);
#11055=ORIENTED_EDGE('',*,*,#8505,.T.);
#11056=ORIENTED_EDGE('',*,*,#8506,.T.);
#11057=ORIENTED_EDGE('',*,*,#8353,.T.);
#11058=ORIENTED_EDGE('',*,*,#8504,.F.);
#11059=ORIENTED_EDGE('',*,*,#8507,.T.);
#11060=ORIENTED_EDGE('',*,*,#8494,.F.);
#11061=ORIENTED_EDGE('',*,*,#8354,.T.);
#11062=ORIENTED_EDGE('',*,*,#8506,.F.);
#11063=ORIENTED_EDGE('',*,*,#8508,.T.);
#11064=ORIENTED_EDGE('',*,*,#8501,.F.);
#11065=ORIENTED_EDGE('',*,*,#8509,.F.);
#11066=ORIENTED_EDGE('',*,*,#8510,.F.);
#11067=ORIENTED_EDGE('',*,*,#8440,.F.);
#11068=ORIENTED_EDGE('',*,*,#8511,.T.);
#11069=ORIENTED_EDGE('',*,*,#8499,.F.);
#11070=ORIENTED_EDGE('',*,*,#8512,.F.);
#11071=ORIENTED_EDGE('',*,*,#8513,.F.);
#11072=ORIENTED_EDGE('',*,*,#8509,.T.);
#11073=ORIENTED_EDGE('',*,*,#8497,.F.);
#11074=ORIENTED_EDGE('',*,*,#8488,.F.);
#11075=ORIENTED_EDGE('',*,*,#8514,.F.);
#11076=ORIENTED_EDGE('',*,*,#8512,.T.);
#11077=ORIENTED_EDGE('',*,*,#8515,.T.);
#11078=ORIENTED_EDGE('',*,*,#8487,.T.);
#11079=ORIENTED_EDGE('',*,*,#8516,.T.);
#11080=ORIENTED_EDGE('',*,*,#8517,.T.);
#11081=ORIENTED_EDGE('',*,*,#8518,.T.);
#11082=ORIENTED_EDGE('',*,*,#8519,.T.);
#11083=ORIENTED_EDGE('',*,*,#8520,.T.);
#11084=ORIENTED_EDGE('',*,*,#8513,.T.);
#11085=ORIENTED_EDGE('',*,*,#8450,.T.);
#11086=ORIENTED_EDGE('',*,*,#8462,.F.);
#11087=ORIENTED_EDGE('',*,*,#8441,.F.);
#11088=ORIENTED_EDGE('',*,*,#8510,.T.);
#11089=ORIENTED_EDGE('',*,*,#8520,.F.);
#11090=ORIENTED_EDGE('',*,*,#8521,.T.);
#11091=ORIENTED_EDGE('',*,*,#8453,.F.);
#11092=ORIENTED_EDGE('',*,*,#8518,.F.);
#11093=ORIENTED_EDGE('',*,*,#8514,.T.);
#11094=ORIENTED_EDGE('',*,*,#8515,.F.);
#11095=ORIENTED_EDGE('',*,*,#8522,.T.);
#11096=ORIENTED_EDGE('',*,*,#8521,.F.);
#11097=ORIENTED_EDGE('',*,*,#8519,.F.);
#11098=ORIENTED_EDGE('',*,*,#8522,.F.);
#11099=ORIENTED_EDGE('',*,*,#8517,.F.);
#11100=ORIENTED_EDGE('',*,*,#8523,.F.);
#11101=ORIENTED_EDGE('',*,*,#8524,.F.);
#11102=ORIENTED_EDGE('',*,*,#8525,.F.);
#11103=ORIENTED_EDGE('',*,*,#8454,.F.);
#11104=ORIENTED_EDGE('',*,*,#8472,.T.);
#11105=ORIENTED_EDGE('',*,*,#8526,.T.);
#11106=ORIENTED_EDGE('',*,*,#8527,.T.);
#11107=ORIENTED_EDGE('',*,*,#8528,.T.);
#11108=ORIENTED_EDGE('',*,*,#8526,.F.);
#11109=ORIENTED_EDGE('',*,*,#8528,.F.);
#11110=ORIENTED_EDGE('',*,*,#8529,.T.);
#11111=ORIENTED_EDGE('',*,*,#8530,.T.);
#11112=ORIENTED_EDGE('',*,*,#8529,.F.);
#11113=ORIENTED_EDGE('',*,*,#8527,.F.);
#11114=ORIENTED_EDGE('',*,*,#8531,.T.);
#11115=ORIENTED_EDGE('',*,*,#8532,.T.);
#11116=ORIENTED_EDGE('',*,*,#8533,.T.);
#11117=ORIENTED_EDGE('',*,*,#8534,.T.);
#11118=ORIENTED_EDGE('',*,*,#8535,.T.);
#11119=ORIENTED_EDGE('',*,*,#8536,.T.);
#11120=ORIENTED_EDGE('',*,*,#8537,.T.);
#11121=ORIENTED_EDGE('',*,*,#8538,.T.);
#11122=ORIENTED_EDGE('',*,*,#8533,.F.);
#11123=ORIENTED_EDGE('',*,*,#8539,.T.);
#11124=ORIENTED_EDGE('',*,*,#8540,.T.);
#11125=ORIENTED_EDGE('',*,*,#8541,.T.);
#11126=ORIENTED_EDGE('',*,*,#8542,.F.);
#11127=ORIENTED_EDGE('',*,*,#8543,.T.);
#11128=ORIENTED_EDGE('',*,*,#8544,.T.);
#11129=ORIENTED_EDGE('',*,*,#8536,.F.);
#11130=ORIENTED_EDGE('',*,*,#8545,.T.);
#11131=ORIENTED_EDGE('',*,*,#8546,.T.);
#11132=ORIENTED_EDGE('',*,*,#8547,.T.);
#11133=ORIENTED_EDGE('',*,*,#8548,.T.);
#11134=ORIENTED_EDGE('',*,*,#8549,.F.);
#11135=ORIENTED_EDGE('',*,*,#8546,.F.);
#11136=ORIENTED_EDGE('',*,*,#8550,.T.);
#11137=ORIENTED_EDGE('',*,*,#8551,.T.);
#11138=ORIENTED_EDGE('',*,*,#8542,.T.);
#11139=ORIENTED_EDGE('',*,*,#8552,.T.);
#11140=ORIENTED_EDGE('',*,*,#8540,.F.);
#11141=ORIENTED_EDGE('',*,*,#8553,.F.);
#11142=ORIENTED_EDGE('',*,*,#8554,.F.);
#11143=ORIENTED_EDGE('',*,*,#8555,.F.);
#11144=ORIENTED_EDGE('',*,*,#8556,.T.);
#11145=ORIENTED_EDGE('',*,*,#8534,.F.);
#11146=ORIENTED_EDGE('',*,*,#8538,.F.);
#11147=ORIENTED_EDGE('',*,*,#8551,.F.);
#11148=ORIENTED_EDGE('',*,*,#8557,.T.);
#11149=ORIENTED_EDGE('',*,*,#8558,.T.);
#11150=ORIENTED_EDGE('',*,*,#8557,.F.);
#11151=ORIENTED_EDGE('',*,*,#8550,.F.);
#11152=ORIENTED_EDGE('',*,*,#8545,.F.);
#11153=ORIENTED_EDGE('',*,*,#8535,.F.);
#11154=ORIENTED_EDGE('',*,*,#8556,.F.);
#11155=ORIENTED_EDGE('',*,*,#8559,.T.);
#11156=ORIENTED_EDGE('',*,*,#8560,.T.);
#11157=ORIENTED_EDGE('',*,*,#8561,.T.);
#11158=ORIENTED_EDGE('',*,*,#8424,.T.);
#11159=ORIENTED_EDGE('',*,*,#8422,.T.);
#11160=ORIENTED_EDGE('',*,*,#8562,.T.);
#11161=ORIENTED_EDGE('',*,*,#8563,.T.);
#11162=ORIENTED_EDGE('',*,*,#8560,.F.);
#11163=ORIENTED_EDGE('',*,*,#8564,.T.);
#11164=ORIENTED_EDGE('',*,*,#8565,.T.);
#11165=ORIENTED_EDGE('',*,*,#8566,.T.);
#11166=ORIENTED_EDGE('',*,*,#8567,.T.);
#11167=ORIENTED_EDGE('',*,*,#8568,.T.);
#11168=ORIENTED_EDGE('',*,*,#8565,.F.);
#11169=ORIENTED_EDGE('',*,*,#8569,.T.);
#11170=ORIENTED_EDGE('',*,*,#8570,.T.);
#11171=ORIENTED_EDGE('',*,*,#8571,.T.);
#11172=ORIENTED_EDGE('',*,*,#8567,.F.);
#11173=ORIENTED_EDGE('',*,*,#8572,.T.);
#11174=ORIENTED_EDGE('',*,*,#8564,.F.);
#11175=ORIENTED_EDGE('',*,*,#8573,.F.);
#11176=ORIENTED_EDGE('',*,*,#8574,.F.);
#11177=ORIENTED_EDGE('',*,*,#8575,.T.);
#11178=ORIENTED_EDGE('',*,*,#8559,.F.);
#11179=ORIENTED_EDGE('',*,*,#8421,.F.);
#11180=ORIENTED_EDGE('',*,*,#8436,.F.);
#11181=ORIENTED_EDGE('',*,*,#8445,.F.);
#11182=ORIENTED_EDGE('',*,*,#8576,.F.);
#11183=ORIENTED_EDGE('',*,*,#8577,.F.);
#11184=ORIENTED_EDGE('',*,*,#8573,.T.);
#11185=ORIENTED_EDGE('',*,*,#8561,.F.);
#11186=ORIENTED_EDGE('',*,*,#8563,.F.);
#11187=ORIENTED_EDGE('',*,*,#8578,.F.);
#11188=ORIENTED_EDGE('',*,*,#8320,.F.);
#11189=ORIENTED_EDGE('',*,*,#8579,.F.);
#11190=ORIENTED_EDGE('',*,*,#8425,.F.);
#11191=ORIENTED_EDGE('',*,*,#8562,.F.);
#11192=ORIENTED_EDGE('',*,*,#8580,.T.);
#11193=ORIENTED_EDGE('',*,*,#8315,.F.);
#11194=ORIENTED_EDGE('',*,*,#8310,.F.);
#11195=ORIENTED_EDGE('',*,*,#8328,.T.);
#11196=ORIENTED_EDGE('',*,*,#8330,.T.);
#11197=ORIENTED_EDGE('',*,*,#8323,.F.);
#11198=ORIENTED_EDGE('',*,*,#8321,.T.);
#11199=ORIENTED_EDGE('',*,*,#8578,.T.);
#11200=ORIENTED_EDGE('',*,*,#8581,.T.);
#11201=ORIENTED_EDGE('',*,*,#8333,.T.);
#11202=ORIENTED_EDGE('',*,*,#8582,.T.);
#11203=ORIENTED_EDGE('',*,*,#8583,.T.);
#11204=ORIENTED_EDGE('',*,*,#8584,.T.);
#11205=ORIENTED_EDGE('',*,*,#8585,.T.);
#11206=ORIENTED_EDGE('',*,*,#8582,.F.);
#11207=ORIENTED_EDGE('',*,*,#8340,.T.);
#11208=ORIENTED_EDGE('',*,*,#8586,.T.);
#11209=ORIENTED_EDGE('',*,*,#8587,.T.);
#11210=ORIENTED_EDGE('',*,*,#8584,.F.);
#11211=ORIENTED_EDGE('',*,*,#8339,.T.);
#11212=ORIENTED_EDGE('',*,*,#8588,.T.);
#11213=ORIENTED_EDGE('',*,*,#8589,.T.);
#11214=ORIENTED_EDGE('',*,*,#8586,.F.);
#11215=ORIENTED_EDGE('',*,*,#8338,.T.);
#11216=ORIENTED_EDGE('',*,*,#8590,.T.);
#11217=ORIENTED_EDGE('',*,*,#8577,.T.);
#11218=ORIENTED_EDGE('',*,*,#8588,.F.);
#11219=ORIENTED_EDGE('',*,*,#8337,.T.);
#11220=ORIENTED_EDGE('',*,*,#8591,.T.);
#11221=ORIENTED_EDGE('',*,*,#8574,.T.);
#11222=ORIENTED_EDGE('',*,*,#8590,.F.);
#11223=ORIENTED_EDGE('',*,*,#8336,.T.);
#11224=ORIENTED_EDGE('',*,*,#8592,.T.);
#11225=ORIENTED_EDGE('',*,*,#8593,.T.);
#11226=ORIENTED_EDGE('',*,*,#8591,.F.);
#11227=ORIENTED_EDGE('',*,*,#8335,.T.);
#11228=ORIENTED_EDGE('',*,*,#8581,.F.);
#11229=ORIENTED_EDGE('',*,*,#8594,.T.);
#11230=ORIENTED_EDGE('',*,*,#8592,.F.);
#11231=ORIENTED_EDGE('',*,*,#8334,.T.);
#11232=ORIENTED_EDGE('',*,*,#8569,.F.);
#11233=ORIENTED_EDGE('',*,*,#8575,.F.);
#11234=ORIENTED_EDGE('',*,*,#8593,.F.);
#11235=ORIENTED_EDGE('',*,*,#8595,.T.);
#11236=ORIENTED_EDGE('',*,*,#8572,.F.);
#11237=ORIENTED_EDGE('',*,*,#8595,.F.);
#11238=ORIENTED_EDGE('',*,*,#8594,.F.);
#11239=ORIENTED_EDGE('',*,*,#8596,.T.);
#11240=ORIENTED_EDGE('',*,*,#8597,.F.);
#11241=ORIENTED_EDGE('',*,*,#8598,.T.);
#11242=ORIENTED_EDGE('',*,*,#8390,.F.);
#11243=ORIENTED_EDGE('',*,*,#8599,.F.);
#11244=ORIENTED_EDGE('',*,*,#8583,.F.);
#11245=ORIENTED_EDGE('',*,*,#8600,.T.);
#11246=ORIENTED_EDGE('',*,*,#8601,.F.);
#11247=ORIENTED_EDGE('',*,*,#8596,.F.);
#11248=ORIENTED_EDGE('',*,*,#8602,.T.);
#11249=ORIENTED_EDGE('',*,*,#8603,.T.);
#11250=ORIENTED_EDGE('',*,*,#8604,.T.);
#11251=ORIENTED_EDGE('',*,*,#8597,.T.);
#11252=ORIENTED_EDGE('',*,*,#8605,.T.);
#11253=ORIENTED_EDGE('',*,*,#8606,.T.);
#11254=ORIENTED_EDGE('',*,*,#8602,.F.);
#11255=ORIENTED_EDGE('',*,*,#8601,.T.);
#11256=ORIENTED_EDGE('',*,*,#8607,.T.);
#11257=ORIENTED_EDGE('',*,*,#8608,.T.);
#11258=ORIENTED_EDGE('',*,*,#8605,.F.);
#11259=ORIENTED_EDGE('',*,*,#8609,.T.);
#11260=ORIENTED_EDGE('',*,*,#8610,.T.);
#11261=ORIENTED_EDGE('',*,*,#8611,.T.);
#11262=ORIENTED_EDGE('',*,*,#8458,.F.);
#11263=ORIENTED_EDGE('',*,*,#8612,.T.);
#11264=ORIENTED_EDGE('',*,*,#8610,.F.);
#11265=ORIENTED_EDGE('',*,*,#8613,.T.);
#11266=ORIENTED_EDGE('',*,*,#8452,.F.);
#11267=ORIENTED_EDGE('',*,*,#8612,.F.);
#11268=ORIENTED_EDGE('',*,*,#8457,.F.);
#11269=ORIENTED_EDGE('',*,*,#8614,.F.);
#11270=ORIENTED_EDGE('',*,*,#8295,.F.);
#11271=ORIENTED_EDGE('',*,*,#8615,.F.);
#11272=ORIENTED_EDGE('',*,*,#8611,.F.);
#11273=ORIENTED_EDGE('',*,*,#8603,.F.);
#11274=ORIENTED_EDGE('',*,*,#8606,.F.);
#11275=ORIENTED_EDGE('',*,*,#8608,.F.);
#11276=ORIENTED_EDGE('',*,*,#8616,.F.);
#11277=ORIENTED_EDGE('',*,*,#8299,.F.);
#11278=ORIENTED_EDGE('',*,*,#8617,.F.);
#11279=ORIENTED_EDGE('',*,*,#8607,.F.);
#11280=ORIENTED_EDGE('',*,*,#8615,.T.);
#11281=ORIENTED_EDGE('',*,*,#8294,.F.);
#11282=ORIENTED_EDGE('',*,*,#8289,.F.);
#11283=ORIENTED_EDGE('',*,*,#8307,.T.);
#11284=ORIENTED_EDGE('',*,*,#8309,.T.);
#11285=ORIENTED_EDGE('',*,*,#8302,.F.);
#11286=ORIENTED_EDGE('',*,*,#8300,.T.);
#11287=ORIENTED_EDGE('',*,*,#8616,.T.);
#11288=ORIENTED_EDGE('',*,*,#8618,.F.);
#11289=ORIENTED_EDGE('',*,*,#8398,.F.);
#11290=ORIENTED_EDGE('',*,*,#8618,.T.);
#11291=ORIENTED_EDGE('',*,*,#8397,.F.);
#11292=ORIENTED_EDGE('',*,*,#8619,.T.);
#11293=ORIENTED_EDGE('',*,*,#8395,.F.);
#11294=ORIENTED_EDGE('',*,*,#8620,.F.);
#11295=ORIENTED_EDGE('',*,*,#8402,.F.);
#11296=ORIENTED_EDGE('',*,*,#8620,.T.);
#11297=ORIENTED_EDGE('',*,*,#8401,.F.);
#11298=ORIENTED_EDGE('',*,*,#8621,.T.);
#11299=ORIENTED_EDGE('',*,*,#8399,.F.);
#11300=ORIENTED_EDGE('',*,*,#8622,.F.);
#11301=ORIENTED_EDGE('',*,*,#8406,.F.);
#11302=ORIENTED_EDGE('',*,*,#8622,.T.);
#11303=ORIENTED_EDGE('',*,*,#8405,.F.);
#11304=ORIENTED_EDGE('',*,*,#8623,.T.);
#11305=ORIENTED_EDGE('',*,*,#8403,.F.);
#11306=ORIENTED_EDGE('',*,*,#8624,.F.);
#11307=ORIENTED_EDGE('',*,*,#8410,.F.);
#11308=ORIENTED_EDGE('',*,*,#8624,.T.);
#11309=ORIENTED_EDGE('',*,*,#8409,.F.);
#11310=ORIENTED_EDGE('',*,*,#8625,.T.);
#11311=ORIENTED_EDGE('',*,*,#8407,.F.);
#11312=ORIENTED_EDGE('',*,*,#8626,.F.);
#11313=ORIENTED_EDGE('',*,*,#8414,.F.);
#11314=ORIENTED_EDGE('',*,*,#8626,.T.);
#11315=ORIENTED_EDGE('',*,*,#8413,.F.);
#11316=ORIENTED_EDGE('',*,*,#8627,.T.);
#11317=ORIENTED_EDGE('',*,*,#8411,.F.);
#11318=ORIENTED_EDGE('',*,*,#8628,.F.);
#11319=ORIENTED_EDGE('',*,*,#8418,.F.);
#11320=ORIENTED_EDGE('',*,*,#8628,.T.);
#11321=ORIENTED_EDGE('',*,*,#8417,.F.);
#11322=ORIENTED_EDGE('',*,*,#8629,.T.);
#11323=ORIENTED_EDGE('',*,*,#8415,.F.);
#11324=ORIENTED_EDGE('',*,*,#8629,.F.);
#11325=ORIENTED_EDGE('',*,*,#8416,.F.);
#11326=ORIENTED_EDGE('',*,*,#8627,.F.);
#11327=ORIENTED_EDGE('',*,*,#8412,.F.);
#11328=ORIENTED_EDGE('',*,*,#8625,.F.);
#11329=ORIENTED_EDGE('',*,*,#8408,.F.);
#11330=ORIENTED_EDGE('',*,*,#8623,.F.);
#11331=ORIENTED_EDGE('',*,*,#8404,.F.);
#11332=ORIENTED_EDGE('',*,*,#8621,.F.);
#11333=ORIENTED_EDGE('',*,*,#8400,.F.);
#11334=ORIENTED_EDGE('',*,*,#8619,.F.);
#11335=ORIENTED_EDGE('',*,*,#8396,.F.);
#11336=ORIENTED_EDGE('',*,*,#8358,.F.);
#11337=ORIENTED_EDGE('',*,*,#8362,.F.);
#11338=ORIENTED_EDGE('',*,*,#8293,.F.);
#11339=ORIENTED_EDGE('',*,*,#8304,.F.);
#11340=ORIENTED_EDGE('',*,*,#8308,.F.);
#11341=ORIENTED_EDGE('',*,*,#8291,.F.);
#11342=ORIENTED_EDGE('',*,*,#8314,.F.);
#11343=ORIENTED_EDGE('',*,*,#8325,.F.);
#11344=ORIENTED_EDGE('',*,*,#8329,.F.);
#11345=ORIENTED_EDGE('',*,*,#8312,.F.);
#11346=ORIENTED_EDGE('',*,*,#8571,.F.);
#11347=ORIENTED_EDGE('',*,*,#8630,.F.);
#11348=ORIENTED_EDGE('',*,*,#8316,.F.);
#11349=ORIENTED_EDGE('',*,*,#8580,.F.);
#11350=ORIENTED_EDGE('',*,*,#8566,.F.);
#11351=ORIENTED_EDGE('',*,*,#8568,.F.);
#11352=ORIENTED_EDGE('',*,*,#8466,.F.);
#11353=ORIENTED_EDGE('',*,*,#8631,.T.);
#11354=ORIENTED_EDGE('',*,*,#8432,.F.);
#11355=ORIENTED_EDGE('',*,*,#8631,.F.);
#11356=ORIENTED_EDGE('',*,*,#8467,.F.);
#11357=ORIENTED_EDGE('',*,*,#8632,.T.);
#11358=ORIENTED_EDGE('',*,*,#8461,.F.);
#11359=ORIENTED_EDGE('',*,*,#8632,.F.);
#11360=ORIENTED_EDGE('',*,*,#8468,.F.);
#11361=ORIENTED_EDGE('',*,*,#8633,.T.);
#11362=ORIENTED_EDGE('',*,*,#8460,.F.);
#11363=ORIENTED_EDGE('',*,*,#8633,.F.);
#11364=ORIENTED_EDGE('',*,*,#8469,.F.);
#11365=ORIENTED_EDGE('',*,*,#8634,.T.);
#11366=ORIENTED_EDGE('',*,*,#8431,.F.);
#11367=ORIENTED_EDGE('',*,*,#8634,.F.);
#11368=ORIENTED_EDGE('',*,*,#8470,.F.);
#11369=ORIENTED_EDGE('',*,*,#8635,.T.);
#11370=ORIENTED_EDGE('',*,*,#8430,.F.);
#11371=ORIENTED_EDGE('',*,*,#8635,.F.);
#11372=ORIENTED_EDGE('',*,*,#8471,.F.);
#11373=ORIENTED_EDGE('',*,*,#8636,.T.);
#11374=ORIENTED_EDGE('',*,*,#8459,.F.);
#11375=ORIENTED_EDGE('',*,*,#8636,.F.);
#11376=ORIENTED_EDGE('',*,*,#8342,.F.);
#11377=ORIENTED_EDGE('',*,*,#8637,.T.);
#11378=ORIENTED_EDGE('',*,*,#8638,.T.);
#11379=ORIENTED_EDGE('',*,*,#8637,.F.);
#11380=ORIENTED_EDGE('',*,*,#8638,.F.);
#11381=ORIENTED_EDGE('',*,*,#8639,.T.);
#11382=ORIENTED_EDGE('',*,*,#8639,.F.);
#11383=ORIENTED_EDGE('',*,*,#8640,.T.);
#11384=ORIENTED_EDGE('',*,*,#8641,.T.);
#11385=ORIENTED_EDGE('',*,*,#8640,.F.);
#11386=ORIENTED_EDGE('',*,*,#8641,.F.);
#11387=ORIENTED_EDGE('',*,*,#8555,.T.);
#11388=ORIENTED_EDGE('',*,*,#8642,.T.);
#11389=ORIENTED_EDGE('',*,*,#8558,.F.);
#11390=ORIENTED_EDGE('',*,*,#8642,.F.);
#11391=ORIENTED_EDGE('',*,*,#8643,.T.);
#11392=ORIENTED_EDGE('',*,*,#8356,.F.);
#11393=ORIENTED_EDGE('',*,*,#8643,.F.);
#11394=ORIENTED_EDGE('',*,*,#8530,.F.);
#11395=ORIENTED_EDGE('',*,*,#8644,.T.);
#11396=ORIENTED_EDGE('',*,*,#8553,.T.);
#11397=ORIENTED_EDGE('',*,*,#8539,.F.);
#11398=ORIENTED_EDGE('',*,*,#8532,.F.);
#11399=ORIENTED_EDGE('',*,*,#8531,.F.);
#11400=ORIENTED_EDGE('',*,*,#8537,.F.);
#11401=ORIENTED_EDGE('',*,*,#8544,.F.);
#11402=ORIENTED_EDGE('',*,*,#8645,.T.);
#11403=ORIENTED_EDGE('',*,*,#8547,.F.);
#11404=ORIENTED_EDGE('',*,*,#8549,.T.);
#11405=ORIENTED_EDGE('',*,*,#8548,.F.);
#11406=ORIENTED_EDGE('',*,*,#8552,.F.);
#11407=ORIENTED_EDGE('',*,*,#8541,.F.);
#11408=ORIENTED_EDGE('',*,*,#8554,.T.);
#11409=ORIENTED_EDGE('',*,*,#8644,.F.);
#11410=ORIENTED_EDGE('',*,*,#8543,.F.);
#11411=ORIENTED_EDGE('',*,*,#8645,.F.);
#11412=ORIENTED_EDGE('',*,*,#8480,.F.);
#11413=ORIENTED_EDGE('',*,*,#8490,.T.);
#11414=ORIENTED_EDGE('',*,*,#8508,.F.);
#11415=ORIENTED_EDGE('',*,*,#8646,.F.);
#11416=ORIENTED_EDGE('',*,*,#8477,.F.);
#11417=ORIENTED_EDGE('',*,*,#8646,.T.);
#11418=ORIENTED_EDGE('',*,*,#8507,.F.);
#11419=ORIENTED_EDGE('',*,*,#8647,.F.);
#11420=ORIENTED_EDGE('',*,*,#8475,.F.);
#11421=ORIENTED_EDGE('',*,*,#8647,.T.);
#11422=ORIENTED_EDGE('',*,*,#8505,.F.);
#11423=ORIENTED_EDGE('',*,*,#8648,.F.);
#11424=ORIENTED_EDGE('',*,*,#8438,.F.);
#11425=ORIENTED_EDGE('',*,*,#8587,.F.);
#11426=ORIENTED_EDGE('',*,*,#8649,.T.);
#11427=ORIENTED_EDGE('',*,*,#8443,.F.);
#11428=ORIENTED_EDGE('',*,*,#8463,.F.);
#11429=ORIENTED_EDGE('',*,*,#8448,.T.);
#11430=ORIENTED_EDGE('',*,*,#8613,.F.);
#11431=ORIENTED_EDGE('',*,*,#8650,.F.);
#11432=ORIENTED_EDGE('',*,*,#8585,.F.);
#11433=ORIENTED_EDGE('',*,*,#8650,.T.);
#11434=ORIENTED_EDGE('',*,*,#8609,.F.);
#11435=ORIENTED_EDGE('',*,*,#8600,.F.);
#11436=ORIENTED_EDGE('',*,*,#8614,.T.);
#11437=ORIENTED_EDGE('',*,*,#8456,.F.);
#11438=ORIENTED_EDGE('',*,*,#8368,.F.);
#11439=ORIENTED_EDGE('',*,*,#8296,.F.);
#11440=ORIENTED_EDGE('',*,*,#8589,.F.);
#11441=ORIENTED_EDGE('',*,*,#8576,.T.);
#11442=ORIENTED_EDGE('',*,*,#8444,.F.);
#11443=ORIENTED_EDGE('',*,*,#8649,.F.);
#11444=ORIENTED_EDGE('',*,*,#8503,.F.);
#11445=ORIENTED_EDGE('',*,*,#8511,.F.);
#11446=ORIENTED_EDGE('',*,*,#8439,.F.);
#11447=ORIENTED_EDGE('',*,*,#8648,.T.);
#11448=ORIENTED_EDGE('',*,*,#8579,.T.);
#11449=ORIENTED_EDGE('',*,*,#8319,.T.);
#11450=ORIENTED_EDGE('',*,*,#8382,.F.);
#11451=ORIENTED_EDGE('',*,*,#8426,.F.);
#11452=ORIENTED_EDGE('',*,*,#8491,.T.);
#11453=ORIENTED_EDGE('',*,*,#8427,.F.);
#11454=ORIENTED_EDGE('',*,*,#8380,.F.);
#11455=ORIENTED_EDGE('',*,*,#8651,.T.);
#11456=ORIENTED_EDGE('',*,*,#8617,.T.);
#11457=ORIENTED_EDGE('',*,*,#8298,.T.);
#11458=ORIENTED_EDGE('',*,*,#8367,.F.);
#11459=ORIENTED_EDGE('',*,*,#8363,.F.);
#11460=ORIENTED_EDGE('',*,*,#8391,.F.);
#11461=ORIENTED_EDGE('',*,*,#8598,.F.);
#11462=ORIENTED_EDGE('',*,*,#8604,.F.);
#11463=ORIENTED_EDGE('',*,*,#8630,.T.);
#11464=ORIENTED_EDGE('',*,*,#8570,.F.);
#11465=ORIENTED_EDGE('',*,*,#8599,.T.);
#11466=ORIENTED_EDGE('',*,*,#8389,.F.);
#11467=ORIENTED_EDGE('',*,*,#8375,.F.);
#11468=ORIENTED_EDGE('',*,*,#8383,.F.);
#11469=ORIENTED_EDGE('',*,*,#8317,.F.);
#11470=ORIENTED_EDGE('',*,*,#8492,.T.);
#11471=ORIENTED_EDGE('',*,*,#8651,.F.);
#11472=ORIENTED_EDGE('',*,*,#8379,.F.);
#11473=ORIENTED_EDGE('',*,*,#8652,.T.);
#11474=ORIENTED_EDGE('',*,*,#8525,.T.);
#11475=ORIENTED_EDGE('',*,*,#8653,.F.);
#11476=ORIENTED_EDGE('',*,*,#8370,.F.);
#11477=ORIENTED_EDGE('',*,*,#8455,.F.);
#11478=ORIENTED_EDGE('',*,*,#8524,.T.);
#11479=ORIENTED_EDGE('',*,*,#8654,.F.);
#11480=ORIENTED_EDGE('',*,*,#8371,.F.);
#11481=ORIENTED_EDGE('',*,*,#8653,.T.);
#11482=ORIENTED_EDGE('',*,*,#8523,.T.);
#11483=ORIENTED_EDGE('',*,*,#8516,.F.);
#11484=ORIENTED_EDGE('',*,*,#8486,.F.);
#11485=ORIENTED_EDGE('',*,*,#8392,.F.);
#11486=ORIENTED_EDGE('',*,*,#8365,.F.);
#11487=ORIENTED_EDGE('',*,*,#8372,.F.);
#11488=ORIENTED_EDGE('',*,*,#8654,.T.);
#11489=ORIENTED_EDGE('',*,*,#8493,.T.);
#11490=ORIENTED_EDGE('',*,*,#8652,.F.);
#11491=ORIENTED_EDGE('',*,*,#8378,.F.);
#11492=ORIENTED_EDGE('',*,*,#8373,.F.);
#11493=ORIENTED_EDGE('',*,*,#8394,.F.);
#11494=ORIENTED_EDGE('',*,*,#8485,.T.);
#11495=ORIENTED_EDGE('',*,*,#8482,.F.);
#11496=ORIENTED_EDGE('',*,*,#8655,.T.);
#11497=ORIENTED_EDGE('',*,*,#8656,.T.);
#11498=ORIENTED_EDGE('',*,*,#8657,.T.);
#11499=ORIENTED_EDGE('',*,*,#8656,.F.);
#11500=ORIENTED_EDGE('',*,*,#8655,.F.);
#11501=ORIENTED_EDGE('',*,*,#8658,.T.);
#11502=ORIENTED_EDGE('',*,*,#8659,.F.);
#11503=ORIENTED_EDGE('',*,*,#8658,.F.);
#11504=ORIENTED_EDGE('',*,*,#8657,.F.);
#11505=ORIENTED_EDGE('',*,*,#8660,.T.);
#11506=ORIENTED_EDGE('',*,*,#8659,.T.);
#11507=ORIENTED_EDGE('',*,*,#8661,.T.);
#11508=ORIENTED_EDGE('',*,*,#8662,.T.);
#11509=ORIENTED_EDGE('',*,*,#8661,.F.);
#11510=ORIENTED_EDGE('',*,*,#8662,.F.);
#11511=ORIENTED_EDGE('',*,*,#8663,.T.);
#11512=ORIENTED_EDGE('',*,*,#8664,.F.);
#11513=ORIENTED_EDGE('',*,*,#8665,.F.);
#11514=ORIENTED_EDGE('',*,*,#8663,.F.);
#11515=ORIENTED_EDGE('',*,*,#8666,.T.);
#11516=ORIENTED_EDGE('',*,*,#8667,.T.);
#11517=ORIENTED_EDGE('',*,*,#8668,.T.);
#11518=ORIENTED_EDGE('',*,*,#8669,.T.);
#11519=ORIENTED_EDGE('',*,*,#8667,.F.);
#11520=ORIENTED_EDGE('',*,*,#8668,.F.);
#11521=ORIENTED_EDGE('',*,*,#8669,.F.);
#11522=ORIENTED_EDGE('',*,*,#8670,.T.);
#11523=ORIENTED_EDGE('',*,*,#8671,.T.);
#11524=ORIENTED_EDGE('',*,*,#8670,.F.);
#11525=ORIENTED_EDGE('',*,*,#8664,.T.);
#11526=ORIENTED_EDGE('',*,*,#8665,.T.);
#11527=ORIENTED_EDGE('',*,*,#8666,.F.);
#11528=ORIENTED_EDGE('',*,*,#8672,.T.);
#11529=ORIENTED_EDGE('',*,*,#8673,.T.);
#11530=ORIENTED_EDGE('',*,*,#8674,.T.);
#11531=ORIENTED_EDGE('',*,*,#8675,.T.);
#11532=ORIENTED_EDGE('',*,*,#8676,.T.);
#11533=ORIENTED_EDGE('',*,*,#8677,.T.);
#11534=ORIENTED_EDGE('',*,*,#8678,.F.);
#11535=ORIENTED_EDGE('',*,*,#8660,.F.);
#11536=ORIENTED_EDGE('',*,*,#8679,.T.);
#11537=ORIENTED_EDGE('',*,*,#8680,.T.);
#11538=ORIENTED_EDGE('',*,*,#8679,.F.);
#11539=ORIENTED_EDGE('',*,*,#8680,.F.);
#11540=ORIENTED_EDGE('',*,*,#8672,.F.);
#11541=ORIENTED_EDGE('',*,*,#8681,.T.);
#11542=ORIENTED_EDGE('',*,*,#8682,.F.);
#11543=ORIENTED_EDGE('',*,*,#8681,.F.);
#11544=ORIENTED_EDGE('',*,*,#8673,.F.);
#11545=ORIENTED_EDGE('',*,*,#8683,.T.);
#11546=ORIENTED_EDGE('',*,*,#8684,.F.);
#11547=ORIENTED_EDGE('',*,*,#8683,.F.);
#11548=ORIENTED_EDGE('',*,*,#8674,.F.);
#11549=ORIENTED_EDGE('',*,*,#8685,.T.);
#11550=ORIENTED_EDGE('',*,*,#8686,.F.);
#11551=ORIENTED_EDGE('',*,*,#8685,.F.);
#11552=ORIENTED_EDGE('',*,*,#8675,.F.);
#11553=ORIENTED_EDGE('',*,*,#8687,.T.);
#11554=ORIENTED_EDGE('',*,*,#8688,.F.);
#11555=ORIENTED_EDGE('',*,*,#8687,.F.);
#11556=ORIENTED_EDGE('',*,*,#8676,.F.);
#11557=ORIENTED_EDGE('',*,*,#8689,.T.);
#11558=ORIENTED_EDGE('',*,*,#8690,.F.);
#11559=ORIENTED_EDGE('',*,*,#8689,.F.);
#11560=ORIENTED_EDGE('',*,*,#8677,.F.);
#11561=ORIENTED_EDGE('',*,*,#8691,.T.);
#11562=ORIENTED_EDGE('',*,*,#8692,.F.);
#11563=ORIENTED_EDGE('',*,*,#8691,.F.);
#11564=ORIENTED_EDGE('',*,*,#8693,.F.);
#11565=ORIENTED_EDGE('',*,*,#8694,.T.);
#11566=ORIENTED_EDGE('',*,*,#8693,.T.);
#11567=ORIENTED_EDGE('',*,*,#8695,.T.);
#11568=ORIENTED_EDGE('',*,*,#8696,.F.);
#11569=ORIENTED_EDGE('',*,*,#8695,.F.);
#11570=ORIENTED_EDGE('',*,*,#8696,.T.);
#11571=ORIENTED_EDGE('',*,*,#8697,.T.);
#11572=ORIENTED_EDGE('',*,*,#8698,.F.);
#11573=ORIENTED_EDGE('',*,*,#8697,.F.);
#11574=ORIENTED_EDGE('',*,*,#8699,.F.);
#11575=ORIENTED_EDGE('',*,*,#8698,.T.);
#11576=ORIENTED_EDGE('',*,*,#8692,.T.);
#11577=ORIENTED_EDGE('',*,*,#8690,.T.);
#11578=ORIENTED_EDGE('',*,*,#8688,.T.);
#11579=ORIENTED_EDGE('',*,*,#8686,.T.);
#11580=ORIENTED_EDGE('',*,*,#8684,.T.);
#11581=ORIENTED_EDGE('',*,*,#8682,.T.);
#11582=ORIENTED_EDGE('',*,*,#8671,.F.);
#11583=ORIENTED_EDGE('',*,*,#8700,.T.);
#11584=ORIENTED_EDGE('',*,*,#8699,.T.);
#11585=ORIENTED_EDGE('',*,*,#8700,.F.);
#11586=ORIENTED_EDGE('',*,*,#8678,.T.);
#11587=ORIENTED_EDGE('',*,*,#8701,.T.);
#11588=ORIENTED_EDGE('',*,*,#8694,.F.);
#11589=ORIENTED_EDGE('',*,*,#8701,.F.);
#11590=ORIENTED_EDGE('',*,*,#8702,.T.);
#11591=ORIENTED_EDGE('',*,*,#8703,.T.);
#11592=ORIENTED_EDGE('',*,*,#8704,.T.);
#11593=ORIENTED_EDGE('',*,*,#8703,.F.);
#11594=ORIENTED_EDGE('',*,*,#8702,.F.);
#11595=ORIENTED_EDGE('',*,*,#8705,.T.);
#11596=ORIENTED_EDGE('',*,*,#8706,.F.);
#11597=ORIENTED_EDGE('',*,*,#8705,.F.);
#11598=ORIENTED_EDGE('',*,*,#8704,.F.);
#11599=ORIENTED_EDGE('',*,*,#8707,.T.);
#11600=ORIENTED_EDGE('',*,*,#8706,.T.);
#11601=ORIENTED_EDGE('',*,*,#8708,.T.);
#11602=ORIENTED_EDGE('',*,*,#8709,.T.);
#11603=ORIENTED_EDGE('',*,*,#8710,.F.);
#11604=ORIENTED_EDGE('',*,*,#8711,.T.);
#11605=ORIENTED_EDGE('',*,*,#8708,.F.);
#11606=ORIENTED_EDGE('',*,*,#8712,.T.);
#11607=ORIENTED_EDGE('',*,*,#8713,.T.);
#11608=ORIENTED_EDGE('',*,*,#8714,.T.);
#11609=ORIENTED_EDGE('',*,*,#8715,.T.);
#11610=ORIENTED_EDGE('',*,*,#8714,.F.);
#11611=ORIENTED_EDGE('',*,*,#8715,.F.);
#11612=ORIENTED_EDGE('',*,*,#8716,.T.);
#11613=ORIENTED_EDGE('',*,*,#8717,.T.);
#11614=ORIENTED_EDGE('',*,*,#8718,.T.);
#11615=ORIENTED_EDGE('',*,*,#8719,.T.);
#11616=ORIENTED_EDGE('',*,*,#8720,.T.);
#11617=ORIENTED_EDGE('',*,*,#8721,.T.);
#11618=ORIENTED_EDGE('',*,*,#8722,.T.);
#11619=ORIENTED_EDGE('',*,*,#8723,.F.);
#11620=ORIENTED_EDGE('',*,*,#8724,.T.);
#11621=ORIENTED_EDGE('',*,*,#8712,.F.);
#11622=ORIENTED_EDGE('',*,*,#8713,.F.);
#11623=ORIENTED_EDGE('',*,*,#8724,.F.);
#11624=ORIENTED_EDGE('',*,*,#8725,.T.);
#11625=ORIENTED_EDGE('',*,*,#8710,.T.);
#11626=ORIENTED_EDGE('',*,*,#8711,.F.);
#11627=ORIENTED_EDGE('',*,*,#8725,.F.);
#11628=ORIENTED_EDGE('',*,*,#8709,.F.);
#11629=ORIENTED_EDGE('',*,*,#8707,.F.);
#11630=ORIENTED_EDGE('',*,*,#8726,.T.);
#11631=ORIENTED_EDGE('',*,*,#8727,.T.);
#11632=ORIENTED_EDGE('',*,*,#8726,.F.);
#11633=ORIENTED_EDGE('',*,*,#8727,.F.);
#11634=ORIENTED_EDGE('',*,*,#8716,.F.);
#11635=ORIENTED_EDGE('',*,*,#8728,.T.);
#11636=ORIENTED_EDGE('',*,*,#8729,.F.);
#11637=ORIENTED_EDGE('',*,*,#8728,.F.);
#11638=ORIENTED_EDGE('',*,*,#8717,.F.);
#11639=ORIENTED_EDGE('',*,*,#8730,.T.);
#11640=ORIENTED_EDGE('',*,*,#8731,.F.);
#11641=ORIENTED_EDGE('',*,*,#8730,.F.);
#11642=ORIENTED_EDGE('',*,*,#8718,.F.);
#11643=ORIENTED_EDGE('',*,*,#8732,.T.);
#11644=ORIENTED_EDGE('',*,*,#8733,.F.);
#11645=ORIENTED_EDGE('',*,*,#8732,.F.);
#11646=ORIENTED_EDGE('',*,*,#8719,.F.);
#11647=ORIENTED_EDGE('',*,*,#8734,.T.);
#11648=ORIENTED_EDGE('',*,*,#8735,.F.);
#11649=ORIENTED_EDGE('',*,*,#8734,.F.);
#11650=ORIENTED_EDGE('',*,*,#8720,.F.);
#11651=ORIENTED_EDGE('',*,*,#8736,.T.);
#11652=ORIENTED_EDGE('',*,*,#8737,.F.);
#11653=ORIENTED_EDGE('',*,*,#8736,.F.);
#11654=ORIENTED_EDGE('',*,*,#8721,.F.);
#11655=ORIENTED_EDGE('',*,*,#8738,.T.);
#11656=ORIENTED_EDGE('',*,*,#8739,.F.);
#11657=ORIENTED_EDGE('',*,*,#8738,.F.);
#11658=ORIENTED_EDGE('',*,*,#8740,.T.);
#11659=ORIENTED_EDGE('',*,*,#8741,.T.);
#11660=ORIENTED_EDGE('',*,*,#8722,.F.);
#11661=ORIENTED_EDGE('',*,*,#8741,.F.);
#11662=ORIENTED_EDGE('',*,*,#8742,.F.);
#11663=ORIENTED_EDGE('',*,*,#8743,.T.);
#11664=ORIENTED_EDGE('',*,*,#8723,.T.);
#11665=ORIENTED_EDGE('',*,*,#8743,.F.);
#11666=ORIENTED_EDGE('',*,*,#8742,.T.);
#11667=ORIENTED_EDGE('',*,*,#8744,.F.);
#11668=ORIENTED_EDGE('',*,*,#8739,.T.);
#11669=ORIENTED_EDGE('',*,*,#8737,.T.);
#11670=ORIENTED_EDGE('',*,*,#8735,.T.);
#11671=ORIENTED_EDGE('',*,*,#8733,.T.);
#11672=ORIENTED_EDGE('',*,*,#8731,.T.);
#11673=ORIENTED_EDGE('',*,*,#8729,.T.);
#11674=ORIENTED_EDGE('',*,*,#8744,.T.);
#11675=ORIENTED_EDGE('',*,*,#8745,.T.);
#11676=ORIENTED_EDGE('',*,*,#8746,.F.);
#11677=ORIENTED_EDGE('',*,*,#8745,.F.);
#11678=ORIENTED_EDGE('',*,*,#8746,.T.);
#11679=ORIENTED_EDGE('',*,*,#8747,.T.);
#11680=ORIENTED_EDGE('',*,*,#8748,.F.);
#11681=ORIENTED_EDGE('',*,*,#8747,.F.);
#11682=ORIENTED_EDGE('',*,*,#8748,.T.);
#11683=ORIENTED_EDGE('',*,*,#8740,.F.);
#11684=ORIENTED_EDGE('',*,*,#8749,.F.);
#11685=ORIENTED_EDGE('',*,*,#8750,.T.);
#11686=ORIENTED_EDGE('',*,*,#8751,.F.);
#11687=ORIENTED_EDGE('',*,*,#8750,.F.);
#11688=ORIENTED_EDGE('',*,*,#8752,.F.);
#11689=ORIENTED_EDGE('',*,*,#8753,.T.);
#11690=ORIENTED_EDGE('',*,*,#8754,.F.);
#11691=ORIENTED_EDGE('',*,*,#8753,.F.);
#11692=ORIENTED_EDGE('',*,*,#8755,.F.);
#11693=ORIENTED_EDGE('',*,*,#8756,.T.);
#11694=ORIENTED_EDGE('',*,*,#8757,.F.);
#11695=ORIENTED_EDGE('',*,*,#8756,.F.);
#11696=ORIENTED_EDGE('',*,*,#8758,.F.);
#11697=ORIENTED_EDGE('',*,*,#8759,.T.);
#11698=ORIENTED_EDGE('',*,*,#8760,.F.);
#11699=ORIENTED_EDGE('',*,*,#8759,.F.);
#11700=ORIENTED_EDGE('',*,*,#8761,.F.);
#11701=ORIENTED_EDGE('',*,*,#8762,.T.);
#11702=ORIENTED_EDGE('',*,*,#8763,.F.);
#11703=ORIENTED_EDGE('',*,*,#8762,.F.);
#11704=ORIENTED_EDGE('',*,*,#8764,.F.);
#11705=ORIENTED_EDGE('',*,*,#8765,.T.);
#11706=ORIENTED_EDGE('',*,*,#8766,.F.);
#11707=ORIENTED_EDGE('',*,*,#8765,.F.);
#11708=ORIENTED_EDGE('',*,*,#8767,.T.);
#11709=ORIENTED_EDGE('',*,*,#8768,.T.);
#11710=ORIENTED_EDGE('',*,*,#8769,.F.);
#11711=ORIENTED_EDGE('',*,*,#8768,.F.);
#11712=ORIENTED_EDGE('',*,*,#8770,.F.);
#11713=ORIENTED_EDGE('',*,*,#8769,.T.);
#11714=ORIENTED_EDGE('',*,*,#8764,.T.);
#11715=ORIENTED_EDGE('',*,*,#8761,.T.);
#11716=ORIENTED_EDGE('',*,*,#8758,.T.);
#11717=ORIENTED_EDGE('',*,*,#8755,.T.);
#11718=ORIENTED_EDGE('',*,*,#8752,.T.);
#11719=ORIENTED_EDGE('',*,*,#8749,.T.);
#11720=ORIENTED_EDGE('',*,*,#8771,.F.);
#11721=ORIENTED_EDGE('',*,*,#8772,.T.);
#11722=ORIENTED_EDGE('',*,*,#8770,.T.);
#11723=ORIENTED_EDGE('',*,*,#8772,.F.);
#11724=ORIENTED_EDGE('',*,*,#8771,.T.);
#11725=ORIENTED_EDGE('',*,*,#8767,.F.);
#11726=ORIENTED_EDGE('',*,*,#8766,.T.);
#11727=ORIENTED_EDGE('',*,*,#8763,.T.);
#11728=ORIENTED_EDGE('',*,*,#8760,.T.);
#11729=ORIENTED_EDGE('',*,*,#8757,.T.);
#11730=ORIENTED_EDGE('',*,*,#8754,.T.);
#11731=ORIENTED_EDGE('',*,*,#8751,.T.);
#11732=ORIENTED_EDGE('',*,*,#8773,.F.);
#11733=ORIENTED_EDGE('',*,*,#8774,.T.);
#11734=ORIENTED_EDGE('',*,*,#8775,.F.);
#11735=ORIENTED_EDGE('',*,*,#8774,.F.);
#11736=ORIENTED_EDGE('',*,*,#8776,.F.);
#11737=ORIENTED_EDGE('',*,*,#8777,.T.);
#11738=ORIENTED_EDGE('',*,*,#8778,.F.);
#11739=ORIENTED_EDGE('',*,*,#8777,.F.);
#11740=ORIENTED_EDGE('',*,*,#8779,.F.);
#11741=ORIENTED_EDGE('',*,*,#8780,.T.);
#11742=ORIENTED_EDGE('',*,*,#8781,.F.);
#11743=ORIENTED_EDGE('',*,*,#8780,.F.);
#11744=ORIENTED_EDGE('',*,*,#8782,.F.);
#11745=ORIENTED_EDGE('',*,*,#8783,.T.);
#11746=ORIENTED_EDGE('',*,*,#8784,.F.);
#11747=ORIENTED_EDGE('',*,*,#8783,.F.);
#11748=ORIENTED_EDGE('',*,*,#8785,.F.);
#11749=ORIENTED_EDGE('',*,*,#8786,.T.);
#11750=ORIENTED_EDGE('',*,*,#8787,.F.);
#11751=ORIENTED_EDGE('',*,*,#8786,.F.);
#11752=ORIENTED_EDGE('',*,*,#8788,.F.);
#11753=ORIENTED_EDGE('',*,*,#8789,.T.);
#11754=ORIENTED_EDGE('',*,*,#8790,.F.);
#11755=ORIENTED_EDGE('',*,*,#8789,.F.);
#11756=ORIENTED_EDGE('',*,*,#8791,.T.);
#11757=ORIENTED_EDGE('',*,*,#8792,.T.);
#11758=ORIENTED_EDGE('',*,*,#8793,.F.);
#11759=ORIENTED_EDGE('',*,*,#8792,.F.);
#11760=ORIENTED_EDGE('',*,*,#8794,.F.);
#11761=ORIENTED_EDGE('',*,*,#8793,.T.);
#11762=ORIENTED_EDGE('',*,*,#8794,.T.);
#11763=ORIENTED_EDGE('',*,*,#8795,.T.);
#11764=ORIENTED_EDGE('',*,*,#8796,.F.);
#11765=ORIENTED_EDGE('',*,*,#8795,.F.);
#11766=ORIENTED_EDGE('',*,*,#8797,.F.);
#11767=ORIENTED_EDGE('',*,*,#8796,.T.);
#11768=ORIENTED_EDGE('',*,*,#8788,.T.);
#11769=ORIENTED_EDGE('',*,*,#8785,.T.);
#11770=ORIENTED_EDGE('',*,*,#8782,.T.);
#11771=ORIENTED_EDGE('',*,*,#8779,.T.);
#11772=ORIENTED_EDGE('',*,*,#8776,.T.);
#11773=ORIENTED_EDGE('',*,*,#8773,.T.);
#11774=ORIENTED_EDGE('',*,*,#8798,.F.);
#11775=ORIENTED_EDGE('',*,*,#8799,.T.);
#11776=ORIENTED_EDGE('',*,*,#8797,.T.);
#11777=ORIENTED_EDGE('',*,*,#8799,.F.);
#11778=ORIENTED_EDGE('',*,*,#8798,.T.);
#11779=ORIENTED_EDGE('',*,*,#8800,.F.);
#11780=ORIENTED_EDGE('',*,*,#8790,.T.);
#11781=ORIENTED_EDGE('',*,*,#8787,.T.);
#11782=ORIENTED_EDGE('',*,*,#8784,.T.);
#11783=ORIENTED_EDGE('',*,*,#8781,.T.);
#11784=ORIENTED_EDGE('',*,*,#8778,.T.);
#11785=ORIENTED_EDGE('',*,*,#8775,.T.);
#11786=ORIENTED_EDGE('',*,*,#8800,.T.);
#11787=ORIENTED_EDGE('',*,*,#8801,.T.);
#11788=ORIENTED_EDGE('',*,*,#8802,.F.);
#11789=ORIENTED_EDGE('',*,*,#8801,.F.);
#11790=ORIENTED_EDGE('',*,*,#8802,.T.);
#11791=ORIENTED_EDGE('',*,*,#8791,.F.);
#11792=ORIENTED_EDGE('',*,*,#8803,.T.);
#11793=ORIENTED_EDGE('',*,*,#8804,.T.);
#11794=ORIENTED_EDGE('',*,*,#8805,.T.);
#11795=ORIENTED_EDGE('',*,*,#8806,.T.);
#11796=ORIENTED_EDGE('',*,*,#8805,.F.);
#11797=ORIENTED_EDGE('',*,*,#8806,.F.);
#11798=ORIENTED_EDGE('',*,*,#8807,.T.);
#11799=ORIENTED_EDGE('',*,*,#8808,.F.);
#11800=ORIENTED_EDGE('',*,*,#8809,.T.);
#11801=ORIENTED_EDGE('',*,*,#8803,.F.);
#11802=ORIENTED_EDGE('',*,*,#8804,.F.);
#11803=ORIENTED_EDGE('',*,*,#8809,.F.);
#11804=ORIENTED_EDGE('',*,*,#8810,.T.);
#11805=ORIENTED_EDGE('',*,*,#8811,.T.);
#11806=ORIENTED_EDGE('',*,*,#8807,.F.);
#11807=ORIENTED_EDGE('',*,*,#8811,.F.);
#11808=ORIENTED_EDGE('',*,*,#8812,.F.);
#11809=ORIENTED_EDGE('',*,*,#8813,.T.);
#11810=ORIENTED_EDGE('',*,*,#8808,.T.);
#11811=ORIENTED_EDGE('',*,*,#8813,.F.);
#11812=ORIENTED_EDGE('',*,*,#8812,.T.);
#11813=ORIENTED_EDGE('',*,*,#8810,.F.);
#11814=ORIENTED_EDGE('',*,*,#8814,.T.);
#11815=ORIENTED_EDGE('',*,*,#8815,.T.);
#11816=ORIENTED_EDGE('',*,*,#8816,.T.);
#11817=ORIENTED_EDGE('',*,*,#8817,.T.);
#11818=ORIENTED_EDGE('',*,*,#8815,.F.);
#11819=ORIENTED_EDGE('',*,*,#8814,.F.);
#11820=ORIENTED_EDGE('',*,*,#8818,.F.);
#11821=ORIENTED_EDGE('',*,*,#8816,.F.);
#11822=ORIENTED_EDGE('',*,*,#8817,.F.);
#11823=ORIENTED_EDGE('',*,*,#8819,.T.);
#11824=ORIENTED_EDGE('',*,*,#8820,.T.);
#11825=ORIENTED_EDGE('',*,*,#8819,.F.);
#11826=ORIENTED_EDGE('',*,*,#8821,.T.);
#11827=ORIENTED_EDGE('',*,*,#8822,.T.);
#11828=ORIENTED_EDGE('',*,*,#8823,.T.);
#11829=ORIENTED_EDGE('',*,*,#8824,.T.);
#11830=ORIENTED_EDGE('',*,*,#8822,.F.);
#11831=ORIENTED_EDGE('',*,*,#8825,.F.);
#11832=ORIENTED_EDGE('',*,*,#8826,.F.);
#11833=ORIENTED_EDGE('',*,*,#8827,.T.);
#11834=ORIENTED_EDGE('',*,*,#8823,.F.);
#11835=ORIENTED_EDGE('',*,*,#8824,.F.);
#11836=ORIENTED_EDGE('',*,*,#8827,.F.);
#11837=ORIENTED_EDGE('',*,*,#8828,.F.);
#11838=ORIENTED_EDGE('',*,*,#8821,.F.);
#11839=ORIENTED_EDGE('',*,*,#8825,.T.);
#11840=ORIENTED_EDGE('',*,*,#8826,.T.);
#11841=ORIENTED_EDGE('',*,*,#8829,.T.);
#11842=ORIENTED_EDGE('',*,*,#8818,.T.);
#11843=ORIENTED_EDGE('',*,*,#8829,.F.);
#11844=ORIENTED_EDGE('',*,*,#8820,.F.);
#11845=ORIENTED_EDGE('',*,*,#8830,.T.);
#11846=ORIENTED_EDGE('',*,*,#8828,.T.);
#11847=ORIENTED_EDGE('',*,*,#8830,.F.);
#11848=ORIENTED_EDGE('',*,*,#8831,.F.);
#11849=ORIENTED_EDGE('',*,*,#8832,.T.);
#11850=ORIENTED_EDGE('',*,*,#8833,.T.);
#11851=ORIENTED_EDGE('',*,*,#8834,.T.);
#11852=ORIENTED_EDGE('',*,*,#8835,.F.);
#11853=ORIENTED_EDGE('',*,*,#8836,.T.);
#11854=ORIENTED_EDGE('',*,*,#8831,.T.);
#11855=ORIENTED_EDGE('',*,*,#8837,.T.);
#11856=ORIENTED_EDGE('',*,*,#8838,.F.);
#11857=ORIENTED_EDGE('',*,*,#8839,.T.);
#11858=ORIENTED_EDGE('',*,*,#8835,.T.);
#11859=ORIENTED_EDGE('',*,*,#8840,.T.);
#11860=ORIENTED_EDGE('',*,*,#8841,.F.);
#11861=ORIENTED_EDGE('',*,*,#8842,.T.);
#11862=ORIENTED_EDGE('',*,*,#8838,.T.);
#11863=ORIENTED_EDGE('',*,*,#8843,.T.);
#11864=ORIENTED_EDGE('',*,*,#8844,.F.);
#11865=ORIENTED_EDGE('',*,*,#8845,.T.);
#11866=ORIENTED_EDGE('',*,*,#8841,.T.);
#11867=ORIENTED_EDGE('',*,*,#8846,.T.);
#11868=ORIENTED_EDGE('',*,*,#8847,.F.);
#11869=ORIENTED_EDGE('',*,*,#8848,.T.);
#11870=ORIENTED_EDGE('',*,*,#8844,.T.);
#11871=ORIENTED_EDGE('',*,*,#8849,.T.);
#11872=ORIENTED_EDGE('',*,*,#8850,.F.);
#11873=ORIENTED_EDGE('',*,*,#8851,.T.);
#11874=ORIENTED_EDGE('',*,*,#8847,.T.);
#11875=ORIENTED_EDGE('',*,*,#8852,.T.);
#11876=ORIENTED_EDGE('',*,*,#8853,.F.);
#11877=ORIENTED_EDGE('',*,*,#8854,.T.);
#11878=ORIENTED_EDGE('',*,*,#8850,.T.);
#11879=ORIENTED_EDGE('',*,*,#8855,.T.);
#11880=ORIENTED_EDGE('',*,*,#8856,.F.);
#11881=ORIENTED_EDGE('',*,*,#8857,.T.);
#11882=ORIENTED_EDGE('',*,*,#8853,.T.);
#11883=ORIENTED_EDGE('',*,*,#8858,.T.);
#11884=ORIENTED_EDGE('',*,*,#8859,.F.);
#11885=ORIENTED_EDGE('',*,*,#8860,.T.);
#11886=ORIENTED_EDGE('',*,*,#8856,.T.);
#11887=ORIENTED_EDGE('',*,*,#8861,.T.);
#11888=ORIENTED_EDGE('',*,*,#8862,.F.);
#11889=ORIENTED_EDGE('',*,*,#8863,.T.);
#11890=ORIENTED_EDGE('',*,*,#8859,.T.);
#11891=ORIENTED_EDGE('',*,*,#8864,.T.);
#11892=ORIENTED_EDGE('',*,*,#8865,.F.);
#11893=ORIENTED_EDGE('',*,*,#8866,.T.);
#11894=ORIENTED_EDGE('',*,*,#8862,.T.);
#11895=ORIENTED_EDGE('',*,*,#8867,.T.);
#11896=ORIENTED_EDGE('',*,*,#8868,.F.);
#11897=ORIENTED_EDGE('',*,*,#8869,.T.);
#11898=ORIENTED_EDGE('',*,*,#8865,.T.);
#11899=ORIENTED_EDGE('',*,*,#8870,.T.);
#11900=ORIENTED_EDGE('',*,*,#8871,.F.);
#11901=ORIENTED_EDGE('',*,*,#8872,.T.);
#11902=ORIENTED_EDGE('',*,*,#8868,.T.);
#11903=ORIENTED_EDGE('',*,*,#8873,.T.);
#11904=ORIENTED_EDGE('',*,*,#8874,.F.);
#11905=ORIENTED_EDGE('',*,*,#8875,.T.);
#11906=ORIENTED_EDGE('',*,*,#8871,.T.);
#11907=ORIENTED_EDGE('',*,*,#8876,.T.);
#11908=ORIENTED_EDGE('',*,*,#8877,.F.);
#11909=ORIENTED_EDGE('',*,*,#8878,.T.);
#11910=ORIENTED_EDGE('',*,*,#8879,.F.);
#11911=ORIENTED_EDGE('',*,*,#8880,.F.);
#11912=ORIENTED_EDGE('',*,*,#8881,.F.);
#11913=ORIENTED_EDGE('',*,*,#8882,.T.);
#11914=ORIENTED_EDGE('',*,*,#8877,.T.);
#11915=ORIENTED_EDGE('',*,*,#8883,.F.);
#11916=ORIENTED_EDGE('',*,*,#8884,.F.);
#11917=ORIENTED_EDGE('',*,*,#8885,.T.);
#11918=ORIENTED_EDGE('',*,*,#8881,.T.);
#11919=ORIENTED_EDGE('',*,*,#8886,.F.);
#11920=ORIENTED_EDGE('',*,*,#8887,.F.);
#11921=ORIENTED_EDGE('',*,*,#8888,.T.);
#11922=ORIENTED_EDGE('',*,*,#8884,.T.);
#11923=ORIENTED_EDGE('',*,*,#8889,.F.);
#11924=ORIENTED_EDGE('',*,*,#8890,.F.);
#11925=ORIENTED_EDGE('',*,*,#8891,.T.);
#11926=ORIENTED_EDGE('',*,*,#8887,.T.);
#11927=ORIENTED_EDGE('',*,*,#8892,.F.);
#11928=ORIENTED_EDGE('',*,*,#8893,.F.);
#11929=ORIENTED_EDGE('',*,*,#8894,.T.);
#11930=ORIENTED_EDGE('',*,*,#8890,.T.);
#11931=ORIENTED_EDGE('',*,*,#8895,.F.);
#11932=ORIENTED_EDGE('',*,*,#8896,.F.);
#11933=ORIENTED_EDGE('',*,*,#8897,.T.);
#11934=ORIENTED_EDGE('',*,*,#8893,.T.);
#11935=ORIENTED_EDGE('',*,*,#8898,.F.);
#11936=ORIENTED_EDGE('',*,*,#8899,.F.);
#11937=ORIENTED_EDGE('',*,*,#8900,.T.);
#11938=ORIENTED_EDGE('',*,*,#8896,.T.);
#11939=ORIENTED_EDGE('',*,*,#8901,.F.);
#11940=ORIENTED_EDGE('',*,*,#8902,.F.);
#11941=ORIENTED_EDGE('',*,*,#8903,.T.);
#11942=ORIENTED_EDGE('',*,*,#8899,.T.);
#11943=ORIENTED_EDGE('',*,*,#8904,.F.);
#11944=ORIENTED_EDGE('',*,*,#8905,.F.);
#11945=ORIENTED_EDGE('',*,*,#8906,.T.);
#11946=ORIENTED_EDGE('',*,*,#8902,.T.);
#11947=ORIENTED_EDGE('',*,*,#8907,.F.);
#11948=ORIENTED_EDGE('',*,*,#8908,.F.);
#11949=ORIENTED_EDGE('',*,*,#8909,.T.);
#11950=ORIENTED_EDGE('',*,*,#8905,.T.);
#11951=ORIENTED_EDGE('',*,*,#8910,.F.);
#11952=ORIENTED_EDGE('',*,*,#8911,.F.);
#11953=ORIENTED_EDGE('',*,*,#8912,.T.);
#11954=ORIENTED_EDGE('',*,*,#8908,.T.);
#11955=ORIENTED_EDGE('',*,*,#8913,.F.);
#11956=ORIENTED_EDGE('',*,*,#8914,.F.);
#11957=ORIENTED_EDGE('',*,*,#8915,.T.);
#11958=ORIENTED_EDGE('',*,*,#8911,.T.);
#11959=ORIENTED_EDGE('',*,*,#8916,.F.);
#11960=ORIENTED_EDGE('',*,*,#8917,.F.);
#11961=ORIENTED_EDGE('',*,*,#8918,.T.);
#11962=ORIENTED_EDGE('',*,*,#8914,.T.);
#11963=ORIENTED_EDGE('',*,*,#8919,.F.);
#11964=ORIENTED_EDGE('',*,*,#8920,.F.);
#11965=ORIENTED_EDGE('',*,*,#8921,.T.);
#11966=ORIENTED_EDGE('',*,*,#8917,.T.);
#11967=ORIENTED_EDGE('',*,*,#8922,.F.);
#11968=ORIENTED_EDGE('',*,*,#8923,.F.);
#11969=ORIENTED_EDGE('',*,*,#8924,.T.);
#11970=ORIENTED_EDGE('',*,*,#8925,.T.);
#11971=ORIENTED_EDGE('',*,*,#8926,.T.);
#11972=ORIENTED_EDGE('',*,*,#8927,.F.);
#11973=ORIENTED_EDGE('',*,*,#8928,.T.);
#11974=ORIENTED_EDGE('',*,*,#8923,.T.);
#11975=ORIENTED_EDGE('',*,*,#8929,.T.);
#11976=ORIENTED_EDGE('',*,*,#8930,.F.);
#11977=ORIENTED_EDGE('',*,*,#8931,.T.);
#11978=ORIENTED_EDGE('',*,*,#8927,.T.);
#11979=ORIENTED_EDGE('',*,*,#8932,.T.);
#11980=ORIENTED_EDGE('',*,*,#8933,.F.);
#11981=ORIENTED_EDGE('',*,*,#8934,.T.);
#11982=ORIENTED_EDGE('',*,*,#8930,.T.);
#11983=ORIENTED_EDGE('',*,*,#8935,.T.);
#11984=ORIENTED_EDGE('',*,*,#8936,.F.);
#11985=ORIENTED_EDGE('',*,*,#8937,.T.);
#11986=ORIENTED_EDGE('',*,*,#8933,.T.);
#11987=ORIENTED_EDGE('',*,*,#8938,.T.);
#11988=ORIENTED_EDGE('',*,*,#8939,.F.);
#11989=ORIENTED_EDGE('',*,*,#8940,.T.);
#11990=ORIENTED_EDGE('',*,*,#8936,.T.);
#11991=ORIENTED_EDGE('',*,*,#8941,.T.);
#11992=ORIENTED_EDGE('',*,*,#8942,.F.);
#11993=ORIENTED_EDGE('',*,*,#8943,.T.);
#11994=ORIENTED_EDGE('',*,*,#8939,.T.);
#11995=ORIENTED_EDGE('',*,*,#8944,.T.);
#11996=ORIENTED_EDGE('',*,*,#8945,.F.);
#11997=ORIENTED_EDGE('',*,*,#8946,.T.);
#11998=ORIENTED_EDGE('',*,*,#8942,.T.);
#11999=ORIENTED_EDGE('',*,*,#8947,.T.);
#12000=ORIENTED_EDGE('',*,*,#8948,.F.);
#12001=ORIENTED_EDGE('',*,*,#8949,.T.);
#12002=ORIENTED_EDGE('',*,*,#8945,.T.);
#12003=ORIENTED_EDGE('',*,*,#8950,.T.);
#12004=ORIENTED_EDGE('',*,*,#8951,.F.);
#12005=ORIENTED_EDGE('',*,*,#8952,.T.);
#12006=ORIENTED_EDGE('',*,*,#8948,.T.);
#12007=ORIENTED_EDGE('',*,*,#8953,.T.);
#12008=ORIENTED_EDGE('',*,*,#8954,.F.);
#12009=ORIENTED_EDGE('',*,*,#8955,.T.);
#12010=ORIENTED_EDGE('',*,*,#8951,.T.);
#12011=ORIENTED_EDGE('',*,*,#8956,.T.);
#12012=ORIENTED_EDGE('',*,*,#8957,.F.);
#12013=ORIENTED_EDGE('',*,*,#8958,.T.);
#12014=ORIENTED_EDGE('',*,*,#8954,.T.);
#12015=ORIENTED_EDGE('',*,*,#8959,.T.);
#12016=ORIENTED_EDGE('',*,*,#8960,.F.);
#12017=ORIENTED_EDGE('',*,*,#8961,.T.);
#12018=ORIENTED_EDGE('',*,*,#8957,.T.);
#12019=ORIENTED_EDGE('',*,*,#8962,.T.);
#12020=ORIENTED_EDGE('',*,*,#8963,.F.);
#12021=ORIENTED_EDGE('',*,*,#8964,.T.);
#12022=ORIENTED_EDGE('',*,*,#8960,.T.);
#12023=ORIENTED_EDGE('',*,*,#8965,.T.);
#12024=ORIENTED_EDGE('',*,*,#8966,.F.);
#12025=ORIENTED_EDGE('',*,*,#8967,.T.);
#12026=ORIENTED_EDGE('',*,*,#8963,.T.);
#12027=ORIENTED_EDGE('',*,*,#8968,.T.);
#12028=ORIENTED_EDGE('',*,*,#8969,.F.);
#12029=ORIENTED_EDGE('',*,*,#8970,.T.);
#12030=ORIENTED_EDGE('',*,*,#8971,.F.);
#12031=ORIENTED_EDGE('',*,*,#8972,.F.);
#12032=ORIENTED_EDGE('',*,*,#8973,.F.);
#12033=ORIENTED_EDGE('',*,*,#8974,.T.);
#12034=ORIENTED_EDGE('',*,*,#8969,.T.);
#12035=ORIENTED_EDGE('',*,*,#8975,.F.);
#12036=ORIENTED_EDGE('',*,*,#8976,.F.);
#12037=ORIENTED_EDGE('',*,*,#8977,.T.);
#12038=ORIENTED_EDGE('',*,*,#8973,.T.);
#12039=ORIENTED_EDGE('',*,*,#8978,.F.);
#12040=ORIENTED_EDGE('',*,*,#8979,.F.);
#12041=ORIENTED_EDGE('',*,*,#8980,.T.);
#12042=ORIENTED_EDGE('',*,*,#8976,.T.);
#12043=ORIENTED_EDGE('',*,*,#8981,.F.);
#12044=ORIENTED_EDGE('',*,*,#8982,.F.);
#12045=ORIENTED_EDGE('',*,*,#8983,.T.);
#12046=ORIENTED_EDGE('',*,*,#8979,.T.);
#12047=ORIENTED_EDGE('',*,*,#8984,.F.);
#12048=ORIENTED_EDGE('',*,*,#8985,.F.);
#12049=ORIENTED_EDGE('',*,*,#8986,.T.);
#12050=ORIENTED_EDGE('',*,*,#8982,.T.);
#12051=ORIENTED_EDGE('',*,*,#8987,.F.);
#12052=ORIENTED_EDGE('',*,*,#8988,.F.);
#12053=ORIENTED_EDGE('',*,*,#8989,.T.);
#12054=ORIENTED_EDGE('',*,*,#8985,.T.);
#12055=ORIENTED_EDGE('',*,*,#8990,.F.);
#12056=ORIENTED_EDGE('',*,*,#8991,.F.);
#12057=ORIENTED_EDGE('',*,*,#8992,.T.);
#12058=ORIENTED_EDGE('',*,*,#8988,.T.);
#12059=ORIENTED_EDGE('',*,*,#8993,.F.);
#12060=ORIENTED_EDGE('',*,*,#8994,.F.);
#12061=ORIENTED_EDGE('',*,*,#8995,.T.);
#12062=ORIENTED_EDGE('',*,*,#8991,.T.);
#12063=ORIENTED_EDGE('',*,*,#8996,.F.);
#12064=ORIENTED_EDGE('',*,*,#8997,.F.);
#12065=ORIENTED_EDGE('',*,*,#8998,.T.);
#12066=ORIENTED_EDGE('',*,*,#8994,.T.);
#12067=ORIENTED_EDGE('',*,*,#8999,.F.);
#12068=ORIENTED_EDGE('',*,*,#9000,.F.);
#12069=ORIENTED_EDGE('',*,*,#9001,.T.);
#12070=ORIENTED_EDGE('',*,*,#8997,.T.);
#12071=ORIENTED_EDGE('',*,*,#9002,.F.);
#12072=ORIENTED_EDGE('',*,*,#9003,.F.);
#12073=ORIENTED_EDGE('',*,*,#9004,.T.);
#12074=ORIENTED_EDGE('',*,*,#9000,.T.);
#12075=ORIENTED_EDGE('',*,*,#9005,.F.);
#12076=ORIENTED_EDGE('',*,*,#9006,.F.);
#12077=ORIENTED_EDGE('',*,*,#9007,.T.);
#12078=ORIENTED_EDGE('',*,*,#9003,.T.);
#12079=ORIENTED_EDGE('',*,*,#9008,.F.);
#12080=ORIENTED_EDGE('',*,*,#9009,.F.);
#12081=ORIENTED_EDGE('',*,*,#9010,.T.);
#12082=ORIENTED_EDGE('',*,*,#9006,.T.);
#12083=ORIENTED_EDGE('',*,*,#9011,.F.);
#12084=ORIENTED_EDGE('',*,*,#9012,.F.);
#12085=ORIENTED_EDGE('',*,*,#9013,.T.);
#12086=ORIENTED_EDGE('',*,*,#9009,.T.);
#12087=ORIENTED_EDGE('',*,*,#9014,.F.);
#12088=ORIENTED_EDGE('',*,*,#8971,.T.);
#12089=ORIENTED_EDGE('',*,*,#9015,.T.);
#12090=ORIENTED_EDGE('',*,*,#9016,.F.);
#12091=ORIENTED_EDGE('',*,*,#9017,.F.);
#12092=ORIENTED_EDGE('',*,*,#9018,.T.);
#12093=ORIENTED_EDGE('',*,*,#9018,.F.);
#12094=ORIENTED_EDGE('',*,*,#9019,.F.);
#12095=ORIENTED_EDGE('',*,*,#8968,.F.);
#12096=ORIENTED_EDGE('',*,*,#8965,.F.);
#12097=ORIENTED_EDGE('',*,*,#8962,.F.);
#12098=ORIENTED_EDGE('',*,*,#8959,.F.);
#12099=ORIENTED_EDGE('',*,*,#8956,.F.);
#12100=ORIENTED_EDGE('',*,*,#8953,.F.);
#12101=ORIENTED_EDGE('',*,*,#8950,.F.);
#12102=ORIENTED_EDGE('',*,*,#8947,.F.);
#12103=ORIENTED_EDGE('',*,*,#8944,.F.);
#12104=ORIENTED_EDGE('',*,*,#8941,.F.);
#12105=ORIENTED_EDGE('',*,*,#8938,.F.);
#12106=ORIENTED_EDGE('',*,*,#8935,.F.);
#12107=ORIENTED_EDGE('',*,*,#8932,.F.);
#12108=ORIENTED_EDGE('',*,*,#8929,.F.);
#12109=ORIENTED_EDGE('',*,*,#8926,.F.);
#12110=ORIENTED_EDGE('',*,*,#9020,.F.);
#12111=ORIENTED_EDGE('',*,*,#9021,.T.);
#12112=ORIENTED_EDGE('',*,*,#9014,.T.);
#12113=ORIENTED_EDGE('',*,*,#9011,.T.);
#12114=ORIENTED_EDGE('',*,*,#9008,.T.);
#12115=ORIENTED_EDGE('',*,*,#9005,.T.);
#12116=ORIENTED_EDGE('',*,*,#9002,.T.);
#12117=ORIENTED_EDGE('',*,*,#8999,.T.);
#12118=ORIENTED_EDGE('',*,*,#8996,.T.);
#12119=ORIENTED_EDGE('',*,*,#8993,.T.);
#12120=ORIENTED_EDGE('',*,*,#8990,.T.);
#12121=ORIENTED_EDGE('',*,*,#8987,.T.);
#12122=ORIENTED_EDGE('',*,*,#8984,.T.);
#12123=ORIENTED_EDGE('',*,*,#8981,.T.);
#12124=ORIENTED_EDGE('',*,*,#8978,.T.);
#12125=ORIENTED_EDGE('',*,*,#8975,.T.);
#12126=ORIENTED_EDGE('',*,*,#8972,.T.);
#12127=ORIENTED_EDGE('',*,*,#9012,.T.);
#12128=ORIENTED_EDGE('',*,*,#9021,.F.);
#12129=ORIENTED_EDGE('',*,*,#9022,.F.);
#12130=ORIENTED_EDGE('',*,*,#9023,.T.);
#12131=ORIENTED_EDGE('',*,*,#9015,.F.);
#12132=ORIENTED_EDGE('',*,*,#8970,.F.);
#12133=ORIENTED_EDGE('',*,*,#8974,.F.);
#12134=ORIENTED_EDGE('',*,*,#8977,.F.);
#12135=ORIENTED_EDGE('',*,*,#8980,.F.);
#12136=ORIENTED_EDGE('',*,*,#8983,.F.);
#12137=ORIENTED_EDGE('',*,*,#8986,.F.);
#12138=ORIENTED_EDGE('',*,*,#8989,.F.);
#12139=ORIENTED_EDGE('',*,*,#8992,.F.);
#12140=ORIENTED_EDGE('',*,*,#8995,.F.);
#12141=ORIENTED_EDGE('',*,*,#8998,.F.);
#12142=ORIENTED_EDGE('',*,*,#9001,.F.);
#12143=ORIENTED_EDGE('',*,*,#9004,.F.);
#12144=ORIENTED_EDGE('',*,*,#9007,.F.);
#12145=ORIENTED_EDGE('',*,*,#9010,.F.);
#12146=ORIENTED_EDGE('',*,*,#9013,.F.);
#12147=ORIENTED_EDGE('',*,*,#9023,.F.);
#12148=ORIENTED_EDGE('',*,*,#9024,.F.);
#12149=ORIENTED_EDGE('',*,*,#8924,.F.);
#12150=ORIENTED_EDGE('',*,*,#8928,.F.);
#12151=ORIENTED_EDGE('',*,*,#8931,.F.);
#12152=ORIENTED_EDGE('',*,*,#8934,.F.);
#12153=ORIENTED_EDGE('',*,*,#8937,.F.);
#12154=ORIENTED_EDGE('',*,*,#8940,.F.);
#12155=ORIENTED_EDGE('',*,*,#8943,.F.);
#12156=ORIENTED_EDGE('',*,*,#8946,.F.);
#12157=ORIENTED_EDGE('',*,*,#8949,.F.);
#12158=ORIENTED_EDGE('',*,*,#8952,.F.);
#12159=ORIENTED_EDGE('',*,*,#8955,.F.);
#12160=ORIENTED_EDGE('',*,*,#8958,.F.);
#12161=ORIENTED_EDGE('',*,*,#8961,.F.);
#12162=ORIENTED_EDGE('',*,*,#8964,.F.);
#12163=ORIENTED_EDGE('',*,*,#8967,.F.);
#12164=ORIENTED_EDGE('',*,*,#9025,.F.);
#12165=ORIENTED_EDGE('',*,*,#8966,.T.);
#12166=ORIENTED_EDGE('',*,*,#9019,.T.);
#12167=ORIENTED_EDGE('',*,*,#9026,.F.);
#12168=ORIENTED_EDGE('',*,*,#9025,.T.);
#12169=ORIENTED_EDGE('',*,*,#9027,.F.);
#12170=ORIENTED_EDGE('',*,*,#9028,.F.);
#12171=ORIENTED_EDGE('',*,*,#8876,.F.);
#12172=ORIENTED_EDGE('',*,*,#8873,.F.);
#12173=ORIENTED_EDGE('',*,*,#8870,.F.);
#12174=ORIENTED_EDGE('',*,*,#8867,.F.);
#12175=ORIENTED_EDGE('',*,*,#8864,.F.);
#12176=ORIENTED_EDGE('',*,*,#8861,.F.);
#12177=ORIENTED_EDGE('',*,*,#8858,.F.);
#12178=ORIENTED_EDGE('',*,*,#8855,.F.);
#12179=ORIENTED_EDGE('',*,*,#8852,.F.);
#12180=ORIENTED_EDGE('',*,*,#8849,.F.);
#12181=ORIENTED_EDGE('',*,*,#8846,.F.);
#12182=ORIENTED_EDGE('',*,*,#8843,.F.);
#12183=ORIENTED_EDGE('',*,*,#8840,.F.);
#12184=ORIENTED_EDGE('',*,*,#8837,.F.);
#12185=ORIENTED_EDGE('',*,*,#8834,.F.);
#12186=ORIENTED_EDGE('',*,*,#9029,.F.);
#12187=ORIENTED_EDGE('',*,*,#9030,.T.);
#12188=ORIENTED_EDGE('',*,*,#8922,.T.);
#12189=ORIENTED_EDGE('',*,*,#8919,.T.);
#12190=ORIENTED_EDGE('',*,*,#8916,.T.);
#12191=ORIENTED_EDGE('',*,*,#8913,.T.);
#12192=ORIENTED_EDGE('',*,*,#8910,.T.);
#12193=ORIENTED_EDGE('',*,*,#8907,.T.);
#12194=ORIENTED_EDGE('',*,*,#8904,.T.);
#12195=ORIENTED_EDGE('',*,*,#8901,.T.);
#12196=ORIENTED_EDGE('',*,*,#8898,.T.);
#12197=ORIENTED_EDGE('',*,*,#8895,.T.);
#12198=ORIENTED_EDGE('',*,*,#8892,.T.);
#12199=ORIENTED_EDGE('',*,*,#8889,.T.);
#12200=ORIENTED_EDGE('',*,*,#8886,.T.);
#12201=ORIENTED_EDGE('',*,*,#8883,.T.);
#12202=ORIENTED_EDGE('',*,*,#8880,.T.);
#12203=ORIENTED_EDGE('',*,*,#9031,.T.);
#12204=ORIENTED_EDGE('',*,*,#9032,.T.);
#12205=ORIENTED_EDGE('',*,*,#9033,.T.);
#12206=ORIENTED_EDGE('',*,*,#9034,.T.);
#12207=ORIENTED_EDGE('',*,*,#9029,.T.);
#12208=ORIENTED_EDGE('',*,*,#8920,.T.);
#12209=ORIENTED_EDGE('',*,*,#9030,.F.);
#12210=ORIENTED_EDGE('',*,*,#9034,.F.);
#12211=ORIENTED_EDGE('',*,*,#9035,.T.);
#12212=ORIENTED_EDGE('',*,*,#9036,.F.);
#12213=ORIENTED_EDGE('',*,*,#8878,.F.);
#12214=ORIENTED_EDGE('',*,*,#8882,.F.);
#12215=ORIENTED_EDGE('',*,*,#8885,.F.);
#12216=ORIENTED_EDGE('',*,*,#8888,.F.);
#12217=ORIENTED_EDGE('',*,*,#8891,.F.);
#12218=ORIENTED_EDGE('',*,*,#8894,.F.);
#12219=ORIENTED_EDGE('',*,*,#8897,.F.);
#12220=ORIENTED_EDGE('',*,*,#8900,.F.);
#12221=ORIENTED_EDGE('',*,*,#8903,.F.);
#12222=ORIENTED_EDGE('',*,*,#8906,.F.);
#12223=ORIENTED_EDGE('',*,*,#8909,.F.);
#12224=ORIENTED_EDGE('',*,*,#8912,.F.);
#12225=ORIENTED_EDGE('',*,*,#8915,.F.);
#12226=ORIENTED_EDGE('',*,*,#8918,.F.);
#12227=ORIENTED_EDGE('',*,*,#8921,.F.);
#12228=ORIENTED_EDGE('',*,*,#9035,.F.);
#12229=ORIENTED_EDGE('',*,*,#9033,.F.);
#12230=ORIENTED_EDGE('',*,*,#8832,.F.);
#12231=ORIENTED_EDGE('',*,*,#8836,.F.);
#12232=ORIENTED_EDGE('',*,*,#8839,.F.);
#12233=ORIENTED_EDGE('',*,*,#8842,.F.);
#12234=ORIENTED_EDGE('',*,*,#8845,.F.);
#12235=ORIENTED_EDGE('',*,*,#8848,.F.);
#12236=ORIENTED_EDGE('',*,*,#8851,.F.);
#12237=ORIENTED_EDGE('',*,*,#8854,.F.);
#12238=ORIENTED_EDGE('',*,*,#8857,.F.);
#12239=ORIENTED_EDGE('',*,*,#8860,.F.);
#12240=ORIENTED_EDGE('',*,*,#8863,.F.);
#12241=ORIENTED_EDGE('',*,*,#8866,.F.);
#12242=ORIENTED_EDGE('',*,*,#8869,.F.);
#12243=ORIENTED_EDGE('',*,*,#8872,.F.);
#12244=ORIENTED_EDGE('',*,*,#8875,.F.);
#12245=ORIENTED_EDGE('',*,*,#9037,.F.);
#12246=ORIENTED_EDGE('',*,*,#9038,.F.);
#12247=ORIENTED_EDGE('',*,*,#9031,.F.);
#12248=ORIENTED_EDGE('',*,*,#8833,.F.);
#12249=ORIENTED_EDGE('',*,*,#9032,.F.);
#12250=ORIENTED_EDGE('',*,*,#9039,.T.);
#12251=ORIENTED_EDGE('',*,*,#9038,.T.);
#12252=ORIENTED_EDGE('',*,*,#9039,.F.);
#12253=ORIENTED_EDGE('',*,*,#8874,.T.);
#12254=ORIENTED_EDGE('',*,*,#9028,.T.);
#12255=ORIENTED_EDGE('',*,*,#9040,.F.);
#12256=ORIENTED_EDGE('',*,*,#9037,.T.);
#12257=ORIENTED_EDGE('',*,*,#9041,.F.);
#12258=ORIENTED_EDGE('',*,*,#9040,.T.);
#12259=ORIENTED_EDGE('',*,*,#9027,.T.);
#12260=ORIENTED_EDGE('',*,*,#8879,.T.);
#12261=ORIENTED_EDGE('',*,*,#9036,.T.);
#12262=ORIENTED_EDGE('',*,*,#9042,.F.);
#12263=ORIENTED_EDGE('',*,*,#9043,.T.);
#12264=ORIENTED_EDGE('',*,*,#9041,.T.);
#12265=ORIENTED_EDGE('',*,*,#9043,.F.);
#12266=ORIENTED_EDGE('',*,*,#9042,.T.);
#12267=ORIENTED_EDGE('',*,*,#9024,.T.);
#12268=ORIENTED_EDGE('',*,*,#9022,.T.);
#12269=ORIENTED_EDGE('',*,*,#9020,.T.);
#12270=ORIENTED_EDGE('',*,*,#8925,.F.);
#12271=ORIENTED_EDGE('',*,*,#9044,.F.);
#12272=ORIENTED_EDGE('',*,*,#9045,.T.);
#12273=ORIENTED_EDGE('',*,*,#9016,.T.);
#12274=ORIENTED_EDGE('',*,*,#9026,.T.);
#12275=ORIENTED_EDGE('',*,*,#9017,.T.);
#12276=ORIENTED_EDGE('',*,*,#9045,.F.);
#12277=ORIENTED_EDGE('',*,*,#9044,.T.);
#12278=ORIENTED_EDGE('',*,*,#9046,.T.);
#12279=ORIENTED_EDGE('',*,*,#9047,.T.);
#12280=ORIENTED_EDGE('',*,*,#9048,.T.);
#12281=ORIENTED_EDGE('',*,*,#9049,.T.);
#12282=ORIENTED_EDGE('',*,*,#9050,.T.);
#12283=ORIENTED_EDGE('',*,*,#9051,.T.);
#12284=ORIENTED_EDGE('',*,*,#9052,.T.);
#12285=ORIENTED_EDGE('',*,*,#9053,.T.);
#12286=ORIENTED_EDGE('',*,*,#9054,.T.);
#12287=ORIENTED_EDGE('',*,*,#9055,.T.);
#12288=ORIENTED_EDGE('',*,*,#9056,.T.);
#12289=ORIENTED_EDGE('',*,*,#9057,.T.);
#12290=ORIENTED_EDGE('',*,*,#9058,.T.);
#12291=ORIENTED_EDGE('',*,*,#9059,.T.);
#12292=ORIENTED_EDGE('',*,*,#9060,.T.);
#12293=ORIENTED_EDGE('',*,*,#9047,.F.);
#12294=ORIENTED_EDGE('',*,*,#9056,.F.);
#12295=ORIENTED_EDGE('',*,*,#9061,.T.);
#12296=ORIENTED_EDGE('',*,*,#9062,.T.);
#12297=ORIENTED_EDGE('',*,*,#9063,.T.);
#12298=ORIENTED_EDGE('',*,*,#9064,.T.);
#12299=ORIENTED_EDGE('',*,*,#9065,.T.);
#12300=ORIENTED_EDGE('',*,*,#9054,.F.);
#12301=ORIENTED_EDGE('',*,*,#9066,.T.);
#12302=ORIENTED_EDGE('',*,*,#9067,.T.);
#12303=ORIENTED_EDGE('',*,*,#9068,.T.);
#12304=ORIENTED_EDGE('',*,*,#9069,.T.);
#12305=ORIENTED_EDGE('',*,*,#9070,.T.);
#12306=ORIENTED_EDGE('',*,*,#9055,.F.);
#12307=ORIENTED_EDGE('',*,*,#9070,.F.);
#12308=ORIENTED_EDGE('',*,*,#9061,.F.);
#12309=ORIENTED_EDGE('',*,*,#9053,.F.);
#12310=ORIENTED_EDGE('',*,*,#9071,.F.);
#12311=ORIENTED_EDGE('',*,*,#9066,.F.);
#12312=ORIENTED_EDGE('',*,*,#9051,.F.);
#12313=ORIENTED_EDGE('',*,*,#9072,.F.);
#12314=ORIENTED_EDGE('',*,*,#9073,.F.);
#12315=ORIENTED_EDGE('',*,*,#9049,.F.);
#12316=ORIENTED_EDGE('',*,*,#9074,.F.);
#12317=ORIENTED_EDGE('',*,*,#9075,.F.);
#12318=ORIENTED_EDGE('',*,*,#9059,.F.);
#12319=ORIENTED_EDGE('',*,*,#9076,.F.);
#12320=ORIENTED_EDGE('',*,*,#9077,.F.);
#12321=ORIENTED_EDGE('',*,*,#9057,.F.);
#12322=ORIENTED_EDGE('',*,*,#9065,.F.);
#12323=ORIENTED_EDGE('',*,*,#9078,.F.);
#12324=ORIENTED_EDGE('',*,*,#9052,.F.);
#12325=ORIENTED_EDGE('',*,*,#9073,.T.);
#12326=ORIENTED_EDGE('',*,*,#9079,.T.);
#12327=ORIENTED_EDGE('',*,*,#9080,.T.);
#12328=ORIENTED_EDGE('',*,*,#9081,.T.);
#12329=ORIENTED_EDGE('',*,*,#9071,.T.);
#12330=ORIENTED_EDGE('',*,*,#9046,.F.);
#12331=ORIENTED_EDGE('',*,*,#9082,.T.);
#12332=ORIENTED_EDGE('',*,*,#9083,.F.);
#12333=ORIENTED_EDGE('',*,*,#9067,.F.);
#12334=ORIENTED_EDGE('',*,*,#9081,.F.);
#12335=ORIENTED_EDGE('',*,*,#9079,.F.);
#12336=ORIENTED_EDGE('',*,*,#9084,.F.);
#12337=ORIENTED_EDGE('',*,*,#9085,.F.);
#12338=ORIENTED_EDGE('',*,*,#9086,.F.);
#12339=ORIENTED_EDGE('',*,*,#9062,.F.);
#12340=ORIENTED_EDGE('',*,*,#9069,.F.);
#12341=ORIENTED_EDGE('',*,*,#9087,.F.);
#12342=ORIENTED_EDGE('',*,*,#9088,.F.);
#12343=ORIENTED_EDGE('',*,*,#9089,.F.);
#12344=ORIENTED_EDGE('',*,*,#9090,.F.);
#12345=ORIENTED_EDGE('',*,*,#9091,.F.);
#12346=ORIENTED_EDGE('',*,*,#9064,.F.);
#12347=ORIENTED_EDGE('',*,*,#9092,.F.);
#12348=ORIENTED_EDGE('',*,*,#9093,.F.);
#12349=ORIENTED_EDGE('',*,*,#9094,.F.);
#12350=ORIENTED_EDGE('',*,*,#9058,.F.);
#12351=ORIENTED_EDGE('',*,*,#9078,.T.);
#12352=ORIENTED_EDGE('',*,*,#9091,.T.);
#12353=ORIENTED_EDGE('',*,*,#9095,.T.);
#12354=ORIENTED_EDGE('',*,*,#9093,.T.);
#12355=ORIENTED_EDGE('',*,*,#9076,.T.);
#12356=ORIENTED_EDGE('',*,*,#9096,.T.);
#12357=ORIENTED_EDGE('',*,*,#9097,.T.);
#12358=ORIENTED_EDGE('',*,*,#9094,.T.);
#12359=ORIENTED_EDGE('',*,*,#9098,.T.);
#12360=ORIENTED_EDGE('',*,*,#9060,.F.);
#12361=ORIENTED_EDGE('',*,*,#9077,.T.);
#12362=ORIENTED_EDGE('',*,*,#9092,.T.);
#12363=ORIENTED_EDGE('',*,*,#9099,.T.);
#12364=ORIENTED_EDGE('',*,*,#9088,.T.);
#12365=ORIENTED_EDGE('',*,*,#9074,.T.);
#12366=ORIENTED_EDGE('',*,*,#9048,.F.);
#12367=ORIENTED_EDGE('',*,*,#9100,.T.);
#12368=ORIENTED_EDGE('',*,*,#9101,.T.);
#12369=ORIENTED_EDGE('',*,*,#9090,.T.);
#12370=ORIENTED_EDGE('',*,*,#9102,.T.);
#12371=ORIENTED_EDGE('',*,*,#9103,.T.);
#12372=ORIENTED_EDGE('',*,*,#9104,.T.);
#12373=ORIENTED_EDGE('',*,*,#9089,.T.);
#12374=ORIENTED_EDGE('',*,*,#9105,.T.);
#12375=ORIENTED_EDGE('',*,*,#9050,.F.);
#12376=ORIENTED_EDGE('',*,*,#9075,.T.);
#12377=ORIENTED_EDGE('',*,*,#9087,.T.);
#12378=ORIENTED_EDGE('',*,*,#9106,.T.);
#12379=ORIENTED_EDGE('',*,*,#9084,.T.);
#12380=ORIENTED_EDGE('',*,*,#9072,.T.);
#12381=ORIENTED_EDGE('',*,*,#9107,.T.);
#12382=ORIENTED_EDGE('',*,*,#9108,.T.);
#12383=ORIENTED_EDGE('',*,*,#9086,.T.);
#12384=ORIENTED_EDGE('',*,*,#9109,.T.);
#12385=ORIENTED_EDGE('',*,*,#9110,.T.);
#12386=ORIENTED_EDGE('',*,*,#9111,.T.);
#12387=ORIENTED_EDGE('',*,*,#9085,.T.);
#12388=ORIENTED_EDGE('',*,*,#9112,.T.);
#12389=ORIENTED_EDGE('',*,*,#9113,.T.);
#12390=ORIENTED_EDGE('',*,*,#9114,.T.);
#12391=ORIENTED_EDGE('',*,*,#9083,.T.);
#12392=ORIENTED_EDGE('',*,*,#9115,.T.);
#12393=ORIENTED_EDGE('',*,*,#9102,.F.);
#12394=ORIENTED_EDGE('',*,*,#9063,.F.);
#12395=ORIENTED_EDGE('',*,*,#9108,.F.);
#12396=ORIENTED_EDGE('',*,*,#9116,.T.);
#12397=ORIENTED_EDGE('',*,*,#9109,.F.);
#12398=ORIENTED_EDGE('',*,*,#9068,.F.);
#12399=ORIENTED_EDGE('',*,*,#9114,.F.);
#12400=ORIENTED_EDGE('',*,*,#9117,.T.);
#12401=ORIENTED_EDGE('',*,*,#9115,.F.);
#12402=ORIENTED_EDGE('',*,*,#9080,.F.);
#12403=ORIENTED_EDGE('',*,*,#9111,.F.);
#12404=ORIENTED_EDGE('',*,*,#9118,.T.);
#12405=ORIENTED_EDGE('',*,*,#9119,.F.);
#12406=ORIENTED_EDGE('',*,*,#9120,.T.);
#12407=ORIENTED_EDGE('',*,*,#9121,.F.);
#12408=ORIENTED_EDGE('',*,*,#9096,.F.);
#12409=ORIENTED_EDGE('',*,*,#9122,.F.);
#12410=ORIENTED_EDGE('',*,*,#9100,.F.);
#12411=ORIENTED_EDGE('',*,*,#9116,.F.);
#12412=ORIENTED_EDGE('',*,*,#9107,.F.);
#12413=ORIENTED_EDGE('',*,*,#9117,.F.);
#12414=ORIENTED_EDGE('',*,*,#9113,.F.);
#12415=ORIENTED_EDGE('',*,*,#9118,.F.);
#12416=ORIENTED_EDGE('',*,*,#9110,.F.);
#12417=ORIENTED_EDGE('',*,*,#9123,.F.);
#12418=ORIENTED_EDGE('',*,*,#9103,.F.);
#12419=ORIENTED_EDGE('',*,*,#9124,.F.);
#12420=ORIENTED_EDGE('',*,*,#9120,.F.);
#12421=ORIENTED_EDGE('',*,*,#9125,.F.);
#12422=ORIENTED_EDGE('',*,*,#9126,.T.);
#12423=ORIENTED_EDGE('',*,*,#9127,.T.);
#12424=ORIENTED_EDGE('',*,*,#9126,.F.);
#12425=ORIENTED_EDGE('',*,*,#9127,.F.);
#12426=ORIENTED_EDGE('',*,*,#9128,.T.);
#12427=ORIENTED_EDGE('',*,*,#9129,.T.);
#12428=ORIENTED_EDGE('',*,*,#9128,.F.);
#12429=ORIENTED_EDGE('',*,*,#9129,.F.);
#12430=ORIENTED_EDGE('',*,*,#9130,.T.);
#12431=ORIENTED_EDGE('',*,*,#9082,.F.);
#12432=ORIENTED_EDGE('',*,*,#9130,.F.);
#12433=ORIENTED_EDGE('',*,*,#9104,.F.);
#12434=ORIENTED_EDGE('',*,*,#9123,.T.);
#12435=ORIENTED_EDGE('',*,*,#9112,.F.);
#12436=ORIENTED_EDGE('',*,*,#9106,.F.);
#12437=ORIENTED_EDGE('',*,*,#9097,.F.);
#12438=ORIENTED_EDGE('',*,*,#9121,.T.);
#12439=ORIENTED_EDGE('',*,*,#9124,.T.);
#12440=ORIENTED_EDGE('',*,*,#9105,.F.);
#12441=ORIENTED_EDGE('',*,*,#9099,.F.);
#12442=ORIENTED_EDGE('',*,*,#9101,.F.);
#12443=ORIENTED_EDGE('',*,*,#9122,.T.);
#12444=ORIENTED_EDGE('',*,*,#9098,.F.);
#12445=ORIENTED_EDGE('',*,*,#9095,.F.);
#12446=ORIENTED_EDGE('',*,*,#9119,.T.);
#12447=ORIENTED_EDGE('',*,*,#9125,.T.);
#12448=ORIENTED_EDGE('',*,*,#9131,.T.);
#12449=ORIENTED_EDGE('',*,*,#9132,.T.);
#12450=ORIENTED_EDGE('',*,*,#9133,.T.);
#12451=ORIENTED_EDGE('',*,*,#9134,.T.);
#12452=ORIENTED_EDGE('',*,*,#9132,.F.);
#12453=ORIENTED_EDGE('',*,*,#9135,.F.);
#12454=ORIENTED_EDGE('',*,*,#9131,.F.);
#12455=ORIENTED_EDGE('',*,*,#9133,.F.);
#12456=ORIENTED_EDGE('',*,*,#9134,.F.);
#12457=ORIENTED_EDGE('',*,*,#9136,.T.);
#12458=ORIENTED_EDGE('',*,*,#9137,.T.);
#12459=ORIENTED_EDGE('',*,*,#9138,.T.);
#12460=ORIENTED_EDGE('',*,*,#9139,.T.);
#12461=ORIENTED_EDGE('',*,*,#9138,.F.);
#12462=ORIENTED_EDGE('',*,*,#9140,.F.);
#12463=ORIENTED_EDGE('',*,*,#9141,.F.);
#12464=ORIENTED_EDGE('',*,*,#9137,.F.);
#12465=ORIENTED_EDGE('',*,*,#9142,.F.);
#12466=ORIENTED_EDGE('',*,*,#9143,.F.);
#12467=ORIENTED_EDGE('',*,*,#9136,.F.);
#12468=ORIENTED_EDGE('',*,*,#9144,.T.);
#12469=ORIENTED_EDGE('',*,*,#9145,.T.);
#12470=ORIENTED_EDGE('',*,*,#9146,.T.);
#12471=ORIENTED_EDGE('',*,*,#9145,.F.);
#12472=ORIENTED_EDGE('',*,*,#9147,.F.);
#12473=ORIENTED_EDGE('',*,*,#9144,.F.);
#12474=ORIENTED_EDGE('',*,*,#9148,.F.);
#12475=ORIENTED_EDGE('',*,*,#9149,.T.);
#12476=ORIENTED_EDGE('',*,*,#9146,.F.);
#12477=ORIENTED_EDGE('',*,*,#9149,.F.);
#12478=ORIENTED_EDGE('',*,*,#9150,.T.);
#12479=ORIENTED_EDGE('',*,*,#9151,.T.);
#12480=ORIENTED_EDGE('',*,*,#9147,.T.);
#12481=ORIENTED_EDGE('',*,*,#9151,.F.);
#12482=ORIENTED_EDGE('',*,*,#9150,.F.);
#12483=ORIENTED_EDGE('',*,*,#9152,.T.);
#12484=ORIENTED_EDGE('',*,*,#9153,.F.);
#12485=ORIENTED_EDGE('',*,*,#9154,.F.);
#12486=ORIENTED_EDGE('',*,*,#9152,.F.);
#12487=ORIENTED_EDGE('',*,*,#9153,.T.);
#12488=ORIENTED_EDGE('',*,*,#9154,.T.);
#12489=ORIENTED_EDGE('',*,*,#9155,.T.);
#12490=ORIENTED_EDGE('',*,*,#9156,.T.);
#12491=ORIENTED_EDGE('',*,*,#9155,.F.);
#12492=ORIENTED_EDGE('',*,*,#9156,.F.);
#12493=ORIENTED_EDGE('',*,*,#9157,.T.);
#12494=ORIENTED_EDGE('',*,*,#9158,.T.);
#12495=ORIENTED_EDGE('',*,*,#9159,.T.);
#12496=ORIENTED_EDGE('',*,*,#9160,.T.);
#12497=ORIENTED_EDGE('',*,*,#9161,.T.);
#12498=ORIENTED_EDGE('',*,*,#9159,.F.);
#12499=ORIENTED_EDGE('',*,*,#9161,.F.);
#12500=ORIENTED_EDGE('',*,*,#9162,.T.);
#12501=ORIENTED_EDGE('',*,*,#9163,.F.);
#12502=ORIENTED_EDGE('',*,*,#9162,.F.);
#12503=ORIENTED_EDGE('',*,*,#9160,.F.);
#12504=ORIENTED_EDGE('',*,*,#9158,.F.);
#12505=ORIENTED_EDGE('',*,*,#9164,.F.);
#12506=ORIENTED_EDGE('',*,*,#9163,.T.);
#12507=ORIENTED_EDGE('',*,*,#9165,.T.);
#12508=ORIENTED_EDGE('',*,*,#9166,.T.);
#12509=ORIENTED_EDGE('',*,*,#9165,.F.);
#12510=ORIENTED_EDGE('',*,*,#9166,.F.);
#12511=ORIENTED_EDGE('',*,*,#9167,.T.);
#12512=ORIENTED_EDGE('',*,*,#9168,.T.);
#12513=ORIENTED_EDGE('',*,*,#9169,.T.);
#12514=ORIENTED_EDGE('',*,*,#9170,.T.);
#12515=ORIENTED_EDGE('',*,*,#9171,.T.);
#12516=ORIENTED_EDGE('',*,*,#9172,.T.);
#12517=ORIENTED_EDGE('',*,*,#9173,.T.);
#12518=ORIENTED_EDGE('',*,*,#9170,.F.);
#12519=ORIENTED_EDGE('',*,*,#9174,.T.);
#12520=ORIENTED_EDGE('',*,*,#9175,.T.);
#12521=ORIENTED_EDGE('',*,*,#9176,.T.);
#12522=ORIENTED_EDGE('',*,*,#9172,.F.);
#12523=ORIENTED_EDGE('',*,*,#9177,.T.);
#12524=ORIENTED_EDGE('',*,*,#9178,.T.);
#12525=ORIENTED_EDGE('',*,*,#9179,.T.);
#12526=ORIENTED_EDGE('',*,*,#9175,.F.);
#12527=ORIENTED_EDGE('',*,*,#9180,.T.);
#12528=ORIENTED_EDGE('',*,*,#9181,.T.);
#12529=ORIENTED_EDGE('',*,*,#9182,.T.);
#12530=ORIENTED_EDGE('',*,*,#9178,.F.);
#12531=ORIENTED_EDGE('',*,*,#9183,.T.);
#12532=ORIENTED_EDGE('',*,*,#9184,.T.);
#12533=ORIENTED_EDGE('',*,*,#9185,.T.);
#12534=ORIENTED_EDGE('',*,*,#9181,.F.);
#12535=ORIENTED_EDGE('',*,*,#9186,.T.);
#12536=ORIENTED_EDGE('',*,*,#9187,.T.);
#12537=ORIENTED_EDGE('',*,*,#9188,.T.);
#12538=ORIENTED_EDGE('',*,*,#9184,.F.);
#12539=ORIENTED_EDGE('',*,*,#9189,.T.);
#12540=ORIENTED_EDGE('',*,*,#9168,.F.);
#12541=ORIENTED_EDGE('',*,*,#9190,.T.);
#12542=ORIENTED_EDGE('',*,*,#9187,.F.);
#12543=ORIENTED_EDGE('',*,*,#9191,.T.);
#12544=ORIENTED_EDGE('',*,*,#9180,.F.);
#12545=ORIENTED_EDGE('',*,*,#9192,.F.);
#12546=ORIENTED_EDGE('',*,*,#9193,.F.);
#12547=ORIENTED_EDGE('',*,*,#9194,.T.);
#12548=ORIENTED_EDGE('',*,*,#9177,.F.);
#12549=ORIENTED_EDGE('',*,*,#9195,.F.);
#12550=ORIENTED_EDGE('',*,*,#9196,.F.);
#12551=ORIENTED_EDGE('',*,*,#9192,.T.);
#12552=ORIENTED_EDGE('',*,*,#9174,.F.);
#12553=ORIENTED_EDGE('',*,*,#9197,.F.);
#12554=ORIENTED_EDGE('',*,*,#9198,.F.);
#12555=ORIENTED_EDGE('',*,*,#9195,.T.);
#12556=ORIENTED_EDGE('',*,*,#9169,.F.);
#12557=ORIENTED_EDGE('',*,*,#9199,.F.);
#12558=ORIENTED_EDGE('',*,*,#9200,.F.);
#12559=ORIENTED_EDGE('',*,*,#9197,.T.);
#12560=ORIENTED_EDGE('',*,*,#9201,.F.);
#12561=ORIENTED_EDGE('',*,*,#9171,.F.);
#12562=ORIENTED_EDGE('',*,*,#9173,.F.);
#12563=ORIENTED_EDGE('',*,*,#9176,.F.);
#12564=ORIENTED_EDGE('',*,*,#9179,.F.);
#12565=ORIENTED_EDGE('',*,*,#9182,.F.);
#12566=ORIENTED_EDGE('',*,*,#9185,.F.);
#12567=ORIENTED_EDGE('',*,*,#9188,.F.);
#12568=ORIENTED_EDGE('',*,*,#9190,.F.);
#12569=ORIENTED_EDGE('',*,*,#9202,.T.);
#12570=ORIENTED_EDGE('',*,*,#9203,.T.);
#12571=ORIENTED_EDGE('',*,*,#9204,.T.);
#12572=ORIENTED_EDGE('',*,*,#9205,.T.);
#12573=ORIENTED_EDGE('',*,*,#9206,.T.);
#12574=ORIENTED_EDGE('',*,*,#9207,.T.);
#12575=ORIENTED_EDGE('',*,*,#9200,.T.);
#12576=ORIENTED_EDGE('',*,*,#9208,.T.);
#12577=ORIENTED_EDGE('',*,*,#9198,.T.);
#12578=ORIENTED_EDGE('',*,*,#9207,.F.);
#12579=ORIENTED_EDGE('',*,*,#9209,.T.);
#12580=ORIENTED_EDGE('',*,*,#9210,.T.);
#12581=ORIENTED_EDGE('',*,*,#9196,.T.);
#12582=ORIENTED_EDGE('',*,*,#9208,.F.);
#12583=ORIENTED_EDGE('',*,*,#9211,.T.);
#12584=ORIENTED_EDGE('',*,*,#9212,.T.);
#12585=ORIENTED_EDGE('',*,*,#9193,.T.);
#12586=ORIENTED_EDGE('',*,*,#9210,.F.);
#12587=ORIENTED_EDGE('',*,*,#9213,.T.);
#12588=ORIENTED_EDGE('',*,*,#9214,.T.);
#12589=ORIENTED_EDGE('',*,*,#9215,.T.);
#12590=ORIENTED_EDGE('',*,*,#9212,.F.);
#12591=ORIENTED_EDGE('',*,*,#9216,.T.);
#12592=ORIENTED_EDGE('',*,*,#9217,.T.);
#12593=ORIENTED_EDGE('',*,*,#9218,.T.);
#12594=ORIENTED_EDGE('',*,*,#9214,.F.);
#12595=ORIENTED_EDGE('',*,*,#9219,.T.);
#12596=ORIENTED_EDGE('',*,*,#9220,.T.);
#12597=ORIENTED_EDGE('',*,*,#9221,.T.);
#12598=ORIENTED_EDGE('',*,*,#9217,.F.);
#12599=ORIENTED_EDGE('',*,*,#9222,.T.);
#12600=ORIENTED_EDGE('',*,*,#9205,.F.);
#12601=ORIENTED_EDGE('',*,*,#9223,.T.);
#12602=ORIENTED_EDGE('',*,*,#9220,.F.);
#12603=ORIENTED_EDGE('',*,*,#9224,.T.);
#12604=ORIENTED_EDGE('',*,*,#9186,.F.);
#12605=ORIENTED_EDGE('',*,*,#9225,.F.);
#12606=ORIENTED_EDGE('',*,*,#9218,.F.);
#12607=ORIENTED_EDGE('',*,*,#9226,.T.);
#12608=ORIENTED_EDGE('',*,*,#9189,.F.);
#12609=ORIENTED_EDGE('',*,*,#9226,.F.);
#12610=ORIENTED_EDGE('',*,*,#9221,.F.);
#12611=ORIENTED_EDGE('',*,*,#9227,.T.);
#12612=ORIENTED_EDGE('',*,*,#9191,.F.);
#12613=ORIENTED_EDGE('',*,*,#9227,.F.);
#12614=ORIENTED_EDGE('',*,*,#9223,.F.);
#12615=ORIENTED_EDGE('',*,*,#9199,.T.);
#12616=ORIENTED_EDGE('',*,*,#9206,.F.);
#12617=ORIENTED_EDGE('',*,*,#9224,.F.);
#12618=ORIENTED_EDGE('',*,*,#9222,.F.);
#12619=ORIENTED_EDGE('',*,*,#9219,.F.);
#12620=ORIENTED_EDGE('',*,*,#9216,.F.);
#12621=ORIENTED_EDGE('',*,*,#9213,.F.);
#12622=ORIENTED_EDGE('',*,*,#9211,.F.);
#12623=ORIENTED_EDGE('',*,*,#9209,.F.);
#12624=ORIENTED_EDGE('',*,*,#9228,.T.);
#12625=ORIENTED_EDGE('',*,*,#9229,.T.);
#12626=ORIENTED_EDGE('',*,*,#9230,.T.);
#12627=ORIENTED_EDGE('',*,*,#9231,.T.);
#12628=ORIENTED_EDGE('',*,*,#9232,.T.);
#12629=ORIENTED_EDGE('',*,*,#9233,.T.);
#12630=ORIENTED_EDGE('',*,*,#9234,.T.);
#12631=ORIENTED_EDGE('',*,*,#9235,.T.);
#12632=ORIENTED_EDGE('',*,*,#9232,.F.);
#12633=ORIENTED_EDGE('',*,*,#9236,.T.);
#12634=ORIENTED_EDGE('',*,*,#9237,.T.);
#12635=ORIENTED_EDGE('',*,*,#9238,.T.);
#12636=ORIENTED_EDGE('',*,*,#9234,.F.);
#12637=ORIENTED_EDGE('',*,*,#9239,.T.);
#12638=ORIENTED_EDGE('',*,*,#9240,.T.);
#12639=ORIENTED_EDGE('',*,*,#9241,.T.);
#12640=ORIENTED_EDGE('',*,*,#9237,.F.);
#12641=ORIENTED_EDGE('',*,*,#9242,.T.);
#12642=ORIENTED_EDGE('',*,*,#9243,.T.);
#12643=ORIENTED_EDGE('',*,*,#9244,.T.);
#12644=ORIENTED_EDGE('',*,*,#9240,.F.);
#12645=ORIENTED_EDGE('',*,*,#9245,.T.);
#12646=ORIENTED_EDGE('',*,*,#9246,.T.);
#12647=ORIENTED_EDGE('',*,*,#9247,.T.);
#12648=ORIENTED_EDGE('',*,*,#9243,.F.);
#12649=ORIENTED_EDGE('',*,*,#9248,.T.);
#12650=ORIENTED_EDGE('',*,*,#9249,.T.);
#12651=ORIENTED_EDGE('',*,*,#9250,.T.);
#12652=ORIENTED_EDGE('',*,*,#9246,.F.);
#12653=ORIENTED_EDGE('',*,*,#9251,.T.);
#12654=ORIENTED_EDGE('',*,*,#9230,.F.);
#12655=ORIENTED_EDGE('',*,*,#9252,.T.);
#12656=ORIENTED_EDGE('',*,*,#9249,.F.);
#12657=ORIENTED_EDGE('',*,*,#9253,.T.);
#12658=ORIENTED_EDGE('',*,*,#9242,.F.);
#12659=ORIENTED_EDGE('',*,*,#9254,.F.);
#12660=ORIENTED_EDGE('',*,*,#9255,.F.);
#12661=ORIENTED_EDGE('',*,*,#9256,.T.);
#12662=ORIENTED_EDGE('',*,*,#9239,.F.);
#12663=ORIENTED_EDGE('',*,*,#9257,.F.);
#12664=ORIENTED_EDGE('',*,*,#9258,.F.);
#12665=ORIENTED_EDGE('',*,*,#9254,.T.);
#12666=ORIENTED_EDGE('',*,*,#9236,.F.);
#12667=ORIENTED_EDGE('',*,*,#9259,.F.);
#12668=ORIENTED_EDGE('',*,*,#9260,.F.);
#12669=ORIENTED_EDGE('',*,*,#9257,.T.);
#12670=ORIENTED_EDGE('',*,*,#9231,.F.);
#12671=ORIENTED_EDGE('',*,*,#9261,.F.);
#12672=ORIENTED_EDGE('',*,*,#9262,.F.);
#12673=ORIENTED_EDGE('',*,*,#9259,.T.);
#12674=ORIENTED_EDGE('',*,*,#9263,.F.);
#12675=ORIENTED_EDGE('',*,*,#9233,.F.);
#12676=ORIENTED_EDGE('',*,*,#9235,.F.);
#12677=ORIENTED_EDGE('',*,*,#9238,.F.);
#12678=ORIENTED_EDGE('',*,*,#9241,.F.);
#12679=ORIENTED_EDGE('',*,*,#9244,.F.);
#12680=ORIENTED_EDGE('',*,*,#9247,.F.);
#12681=ORIENTED_EDGE('',*,*,#9250,.F.);
#12682=ORIENTED_EDGE('',*,*,#9252,.F.);
#12683=ORIENTED_EDGE('',*,*,#9264,.T.);
#12684=ORIENTED_EDGE('',*,*,#9265,.T.);
#12685=ORIENTED_EDGE('',*,*,#9266,.T.);
#12686=ORIENTED_EDGE('',*,*,#9267,.T.);
#12687=ORIENTED_EDGE('',*,*,#9268,.T.);
#12688=ORIENTED_EDGE('',*,*,#9269,.T.);
#12689=ORIENTED_EDGE('',*,*,#9262,.T.);
#12690=ORIENTED_EDGE('',*,*,#9270,.T.);
#12691=ORIENTED_EDGE('',*,*,#9260,.T.);
#12692=ORIENTED_EDGE('',*,*,#9269,.F.);
#12693=ORIENTED_EDGE('',*,*,#9271,.T.);
#12694=ORIENTED_EDGE('',*,*,#9272,.T.);
#12695=ORIENTED_EDGE('',*,*,#9258,.T.);
#12696=ORIENTED_EDGE('',*,*,#9270,.F.);
#12697=ORIENTED_EDGE('',*,*,#9273,.T.);
#12698=ORIENTED_EDGE('',*,*,#9274,.T.);
#12699=ORIENTED_EDGE('',*,*,#9255,.T.);
#12700=ORIENTED_EDGE('',*,*,#9272,.F.);
#12701=ORIENTED_EDGE('',*,*,#9275,.T.);
#12702=ORIENTED_EDGE('',*,*,#9276,.T.);
#12703=ORIENTED_EDGE('',*,*,#9277,.T.);
#12704=ORIENTED_EDGE('',*,*,#9274,.F.);
#12705=ORIENTED_EDGE('',*,*,#9278,.T.);
#12706=ORIENTED_EDGE('',*,*,#9279,.T.);
#12707=ORIENTED_EDGE('',*,*,#9280,.T.);
#12708=ORIENTED_EDGE('',*,*,#9276,.F.);
#12709=ORIENTED_EDGE('',*,*,#9281,.T.);
#12710=ORIENTED_EDGE('',*,*,#9282,.T.);
#12711=ORIENTED_EDGE('',*,*,#9283,.T.);
#12712=ORIENTED_EDGE('',*,*,#9279,.F.);
#12713=ORIENTED_EDGE('',*,*,#9284,.T.);
#12714=ORIENTED_EDGE('',*,*,#9267,.F.);
#12715=ORIENTED_EDGE('',*,*,#9285,.T.);
#12716=ORIENTED_EDGE('',*,*,#9282,.F.);
#12717=ORIENTED_EDGE('',*,*,#9286,.T.);
#12718=ORIENTED_EDGE('',*,*,#9248,.F.);
#12719=ORIENTED_EDGE('',*,*,#9287,.F.);
#12720=ORIENTED_EDGE('',*,*,#9280,.F.);
#12721=ORIENTED_EDGE('',*,*,#9288,.T.);
#12722=ORIENTED_EDGE('',*,*,#9251,.F.);
#12723=ORIENTED_EDGE('',*,*,#9288,.F.);
#12724=ORIENTED_EDGE('',*,*,#9283,.F.);
#12725=ORIENTED_EDGE('',*,*,#9289,.T.);
#12726=ORIENTED_EDGE('',*,*,#9253,.F.);
#12727=ORIENTED_EDGE('',*,*,#9289,.F.);
#12728=ORIENTED_EDGE('',*,*,#9285,.F.);
#12729=ORIENTED_EDGE('',*,*,#9261,.T.);
#12730=ORIENTED_EDGE('',*,*,#9268,.F.);
#12731=ORIENTED_EDGE('',*,*,#9286,.F.);
#12732=ORIENTED_EDGE('',*,*,#9284,.F.);
#12733=ORIENTED_EDGE('',*,*,#9281,.F.);
#12734=ORIENTED_EDGE('',*,*,#9278,.F.);
#12735=ORIENTED_EDGE('',*,*,#9275,.F.);
#12736=ORIENTED_EDGE('',*,*,#9273,.F.);
#12737=ORIENTED_EDGE('',*,*,#9271,.F.);
#12738=ORIENTED_EDGE('',*,*,#9290,.T.);
#12739=ORIENTED_EDGE('',*,*,#9291,.T.);
#12740=ORIENTED_EDGE('',*,*,#9292,.T.);
#12741=ORIENTED_EDGE('',*,*,#9293,.T.);
#12742=ORIENTED_EDGE('',*,*,#9141,.T.);
#12743=ORIENTED_EDGE('',*,*,#9294,.T.);
#12744=ORIENTED_EDGE('',*,*,#9140,.T.);
#12745=ORIENTED_EDGE('',*,*,#9295,.T.);
#12746=ORIENTED_EDGE('',*,*,#9296,.T.);
#12747=ORIENTED_EDGE('',*,*,#9143,.T.);
#12748=ORIENTED_EDGE('',*,*,#9297,.T.);
#12749=ORIENTED_EDGE('',*,*,#9142,.T.);
#12750=ORIENTED_EDGE('',*,*,#9266,.F.);
#12751=ORIENTED_EDGE('',*,*,#9298,.T.);
#12752=ORIENTED_EDGE('',*,*,#9291,.F.);
#12753=ORIENTED_EDGE('',*,*,#9298,.F.);
#12754=ORIENTED_EDGE('',*,*,#9204,.F.);
#12755=ORIENTED_EDGE('',*,*,#9299,.T.);
#12756=ORIENTED_EDGE('',*,*,#9229,.F.);
#12757=ORIENTED_EDGE('',*,*,#9299,.F.);
#12758=ORIENTED_EDGE('',*,*,#9203,.F.);
#12759=ORIENTED_EDGE('',*,*,#9300,.T.);
#12760=ORIENTED_EDGE('',*,*,#9228,.F.);
#12761=ORIENTED_EDGE('',*,*,#9300,.F.);
#12762=ORIENTED_EDGE('',*,*,#9265,.F.);
#12763=ORIENTED_EDGE('',*,*,#9301,.T.);
#12764=ORIENTED_EDGE('',*,*,#9290,.F.);
#12765=ORIENTED_EDGE('',*,*,#9301,.F.);
#12766=ORIENTED_EDGE('',*,*,#9202,.F.);
#12767=ORIENTED_EDGE('',*,*,#9302,.T.);
#12768=ORIENTED_EDGE('',*,*,#9295,.F.);
#12769=ORIENTED_EDGE('',*,*,#9297,.F.);
#12770=ORIENTED_EDGE('',*,*,#9296,.F.);
#12771=ORIENTED_EDGE('',*,*,#9302,.F.);
#12772=ORIENTED_EDGE('',*,*,#9264,.F.);
#12773=ORIENTED_EDGE('',*,*,#9303,.T.);
#12774=ORIENTED_EDGE('',*,*,#9292,.F.);
#12775=ORIENTED_EDGE('',*,*,#9294,.F.);
#12776=ORIENTED_EDGE('',*,*,#9293,.F.);
#12777=ORIENTED_EDGE('',*,*,#9303,.F.);
#12778=ORIENTED_EDGE('',*,*,#9167,.F.);
#12779=ORIENTED_EDGE('',*,*,#9304,.T.);
#12780=ORIENTED_EDGE('',*,*,#9135,.T.);
#12781=ORIENTED_EDGE('',*,*,#9304,.F.);
#12782=ORIENTED_EDGE('',*,*,#9148,.T.);
#12783=ORIENTED_EDGE('',*,*,#9139,.F.);
#12784=ORIENTED_EDGE('',*,*,#9245,.F.);
#12785=ORIENTED_EDGE('',*,*,#9256,.F.);
#12786=ORIENTED_EDGE('',*,*,#9277,.F.);
#12787=ORIENTED_EDGE('',*,*,#9287,.T.);
#12788=ORIENTED_EDGE('',*,*,#9305,.F.);
#12789=ORIENTED_EDGE('',*,*,#9157,.F.);
#12790=ORIENTED_EDGE('',*,*,#9306,.T.);
#12791=ORIENTED_EDGE('',*,*,#9305,.T.);
#12792=ORIENTED_EDGE('',*,*,#9306,.F.);
#12793=ORIENTED_EDGE('',*,*,#9183,.F.);
#12794=ORIENTED_EDGE('',*,*,#9194,.F.);
#12795=ORIENTED_EDGE('',*,*,#9215,.F.);
#12796=ORIENTED_EDGE('',*,*,#9225,.T.);
#12797=ORIENTED_EDGE('',*,*,#9307,.F.);
#12798=ORIENTED_EDGE('',*,*,#9263,.T.);
#12799=ORIENTED_EDGE('',*,*,#9308,.T.);
#12800=ORIENTED_EDGE('',*,*,#9307,.T.);
#12801=ORIENTED_EDGE('',*,*,#9308,.F.);
#12802=ORIENTED_EDGE('',*,*,#9201,.T.);
#12803=ORIENTED_EDGE('',*,*,#9309,.T.);
#12804=ORIENTED_EDGE('',*,*,#9164,.T.);
#12805=ORIENTED_EDGE('',*,*,#9309,.F.);
#12806=ORIENTED_EDGE('',*,*,#9310,.F.);
#12807=ORIENTED_EDGE('',*,*,#9311,.T.);
#12808=ORIENTED_EDGE('',*,*,#9312,.T.);
#12809=ORIENTED_EDGE('',*,*,#9313,.T.);
#12810=ORIENTED_EDGE('',*,*,#9314,.F.);
#12811=ORIENTED_EDGE('',*,*,#9315,.T.);
#12812=ORIENTED_EDGE('',*,*,#9310,.T.);
#12813=ORIENTED_EDGE('',*,*,#9316,.T.);
#12814=ORIENTED_EDGE('',*,*,#9317,.F.);
#12815=ORIENTED_EDGE('',*,*,#9318,.T.);
#12816=ORIENTED_EDGE('',*,*,#9314,.T.);
#12817=ORIENTED_EDGE('',*,*,#9319,.T.);
#12818=ORIENTED_EDGE('',*,*,#9320,.F.);
#12819=ORIENTED_EDGE('',*,*,#9321,.T.);
#12820=ORIENTED_EDGE('',*,*,#9317,.T.);
#12821=ORIENTED_EDGE('',*,*,#9322,.T.);
#12822=ORIENTED_EDGE('',*,*,#9323,.F.);
#12823=ORIENTED_EDGE('',*,*,#9324,.T.);
#12824=ORIENTED_EDGE('',*,*,#9320,.T.);
#12825=ORIENTED_EDGE('',*,*,#9325,.T.);
#12826=ORIENTED_EDGE('',*,*,#9326,.F.);
#12827=ORIENTED_EDGE('',*,*,#9327,.T.);
#12828=ORIENTED_EDGE('',*,*,#9323,.T.);
#12829=ORIENTED_EDGE('',*,*,#9328,.T.);
#12830=ORIENTED_EDGE('',*,*,#9329,.F.);
#12831=ORIENTED_EDGE('',*,*,#9330,.T.);
#12832=ORIENTED_EDGE('',*,*,#9331,.F.);
#12833=ORIENTED_EDGE('',*,*,#9332,.F.);
#12834=ORIENTED_EDGE('',*,*,#9333,.T.);
#12835=ORIENTED_EDGE('',*,*,#9329,.T.);
#12836=ORIENTED_EDGE('',*,*,#9334,.F.);
#12837=ORIENTED_EDGE('',*,*,#9335,.F.);
#12838=ORIENTED_EDGE('',*,*,#9336,.F.);
#12839=ORIENTED_EDGE('',*,*,#9337,.T.);
#12840=ORIENTED_EDGE('',*,*,#9332,.T.);
#12841=ORIENTED_EDGE('',*,*,#9338,.F.);
#12842=ORIENTED_EDGE('',*,*,#9339,.F.);
#12843=ORIENTED_EDGE('',*,*,#9340,.T.);
#12844=ORIENTED_EDGE('',*,*,#9336,.T.);
#12845=ORIENTED_EDGE('',*,*,#9341,.F.);
#12846=ORIENTED_EDGE('',*,*,#9342,.F.);
#12847=ORIENTED_EDGE('',*,*,#9343,.T.);
#12848=ORIENTED_EDGE('',*,*,#9339,.T.);
#12849=ORIENTED_EDGE('',*,*,#9344,.F.);
#12850=ORIENTED_EDGE('',*,*,#9345,.F.);
#12851=ORIENTED_EDGE('',*,*,#9346,.T.);
#12852=ORIENTED_EDGE('',*,*,#9342,.T.);
#12853=ORIENTED_EDGE('',*,*,#9347,.F.);
#12854=ORIENTED_EDGE('',*,*,#9348,.T.);
#12855=ORIENTED_EDGE('',*,*,#9349,.T.);
#12856=ORIENTED_EDGE('',*,*,#9350,.T.);
#12857=ORIENTED_EDGE('',*,*,#9351,.T.);
#12858=ORIENTED_EDGE('',*,*,#9349,.F.);
#12859=ORIENTED_EDGE('',*,*,#9350,.F.);
#12860=ORIENTED_EDGE('',*,*,#9351,.F.);
#12861=ORIENTED_EDGE('',*,*,#9352,.T.);
#12862=ORIENTED_EDGE('',*,*,#9353,.F.);
#12863=ORIENTED_EDGE('',*,*,#9354,.F.);
#12864=ORIENTED_EDGE('',*,*,#9352,.F.);
#12865=ORIENTED_EDGE('',*,*,#9348,.F.);
#12866=ORIENTED_EDGE('',*,*,#9355,.T.);
#12867=ORIENTED_EDGE('',*,*,#9356,.T.);
#12868=ORIENTED_EDGE('',*,*,#9357,.T.);
#12869=ORIENTED_EDGE('',*,*,#9312,.F.);
#12870=ORIENTED_EDGE('',*,*,#9353,.T.);
#12871=ORIENTED_EDGE('',*,*,#9354,.T.);
#12872=ORIENTED_EDGE('',*,*,#9358,.T.);
#12873=ORIENTED_EDGE('',*,*,#9359,.T.);
#12874=ORIENTED_EDGE('',*,*,#9360,.T.);
#12875=ORIENTED_EDGE('',*,*,#9358,.F.);
#12876=ORIENTED_EDGE('',*,*,#9359,.F.);
#12877=ORIENTED_EDGE('',*,*,#9360,.F.);
#12878=ORIENTED_EDGE('',*,*,#9361,.T.);
#12879=ORIENTED_EDGE('',*,*,#9362,.F.);
#12880=ORIENTED_EDGE('',*,*,#9363,.F.);
#12881=ORIENTED_EDGE('',*,*,#9361,.F.);
#12882=ORIENTED_EDGE('',*,*,#9362,.T.);
#12883=ORIENTED_EDGE('',*,*,#9363,.T.);
#12884=ORIENTED_EDGE('',*,*,#9364,.T.);
#12885=ORIENTED_EDGE('',*,*,#9365,.T.);
#12886=ORIENTED_EDGE('',*,*,#9364,.F.);
#12887=ORIENTED_EDGE('',*,*,#9365,.F.);
#12888=ORIENTED_EDGE('',*,*,#9366,.F.);
#12889=ORIENTED_EDGE('',*,*,#9367,.F.);
#12890=ORIENTED_EDGE('',*,*,#9368,.F.);
#12891=ORIENTED_EDGE('',*,*,#9369,.F.);
#12892=ORIENTED_EDGE('',*,*,#9370,.F.);
#12893=ORIENTED_EDGE('',*,*,#9371,.F.);
#12894=ORIENTED_EDGE('',*,*,#9369,.T.);
#12895=ORIENTED_EDGE('',*,*,#9372,.T.);
#12896=ORIENTED_EDGE('',*,*,#9373,.T.);
#12897=ORIENTED_EDGE('',*,*,#9374,.F.);
#12898=ORIENTED_EDGE('',*,*,#9368,.T.);
#12899=ORIENTED_EDGE('',*,*,#9375,.T.);
#12900=ORIENTED_EDGE('',*,*,#9376,.T.);
#12901=ORIENTED_EDGE('',*,*,#9372,.F.);
#12902=ORIENTED_EDGE('',*,*,#9366,.T.);
#12903=ORIENTED_EDGE('',*,*,#9377,.T.);
#12904=ORIENTED_EDGE('',*,*,#9378,.T.);
#12905=ORIENTED_EDGE('',*,*,#9379,.T.);
#12906=ORIENTED_EDGE('',*,*,#9380,.T.);
#12907=ORIENTED_EDGE('',*,*,#9377,.F.);
#12908=ORIENTED_EDGE('',*,*,#9371,.T.);
#12909=ORIENTED_EDGE('',*,*,#9381,.T.);
#12910=ORIENTED_EDGE('',*,*,#9367,.T.);
#12911=ORIENTED_EDGE('',*,*,#9379,.F.);
#12912=ORIENTED_EDGE('',*,*,#9382,.T.);
#12913=ORIENTED_EDGE('',*,*,#9375,.F.);
#12914=ORIENTED_EDGE('',*,*,#9383,.T.);
#12915=ORIENTED_EDGE('',*,*,#9381,.F.);
#12916=ORIENTED_EDGE('',*,*,#9370,.T.);
#12917=ORIENTED_EDGE('',*,*,#9374,.T.);
#12918=ORIENTED_EDGE('',*,*,#9376,.F.);
#12919=ORIENTED_EDGE('',*,*,#9384,.T.);
#12920=ORIENTED_EDGE('',*,*,#9385,.T.);
#12921=ORIENTED_EDGE('',*,*,#9386,.F.);
#12922=ORIENTED_EDGE('',*,*,#9382,.F.);
#12923=ORIENTED_EDGE('',*,*,#9387,.T.);
#12924=ORIENTED_EDGE('',*,*,#9388,.T.);
#12925=ORIENTED_EDGE('',*,*,#9384,.F.);
#12926=ORIENTED_EDGE('',*,*,#9378,.F.);
#12927=ORIENTED_EDGE('',*,*,#9389,.T.);
#12928=ORIENTED_EDGE('',*,*,#9390,.T.);
#12929=ORIENTED_EDGE('',*,*,#9387,.F.);
#12930=ORIENTED_EDGE('',*,*,#9334,.T.);
#12931=ORIENTED_EDGE('',*,*,#9331,.T.);
#12932=ORIENTED_EDGE('',*,*,#9391,.T.);
#12933=ORIENTED_EDGE('',*,*,#9392,.F.);
#12934=ORIENTED_EDGE('',*,*,#9393,.F.);
#12935=ORIENTED_EDGE('',*,*,#9394,.T.);
#12936=ORIENTED_EDGE('',*,*,#9394,.F.);
#12937=ORIENTED_EDGE('',*,*,#9395,.F.);
#12938=ORIENTED_EDGE('',*,*,#9328,.F.);
#12939=ORIENTED_EDGE('',*,*,#9325,.F.);
#12940=ORIENTED_EDGE('',*,*,#9322,.F.);
#12941=ORIENTED_EDGE('',*,*,#9319,.F.);
#12942=ORIENTED_EDGE('',*,*,#9316,.F.);
#12943=ORIENTED_EDGE('',*,*,#9313,.F.);
#12944=ORIENTED_EDGE('',*,*,#9357,.F.);
#12945=ORIENTED_EDGE('',*,*,#9396,.T.);
#12946=ORIENTED_EDGE('',*,*,#9347,.T.);
#12947=ORIENTED_EDGE('',*,*,#9344,.T.);
#12948=ORIENTED_EDGE('',*,*,#9341,.T.);
#12949=ORIENTED_EDGE('',*,*,#9338,.T.);
#12950=ORIENTED_EDGE('',*,*,#9335,.T.);
#12951=ORIENTED_EDGE('',*,*,#9345,.T.);
#12952=ORIENTED_EDGE('',*,*,#9396,.F.);
#12953=ORIENTED_EDGE('',*,*,#9356,.F.);
#12954=ORIENTED_EDGE('',*,*,#9397,.T.);
#12955=ORIENTED_EDGE('',*,*,#9391,.F.);
#12956=ORIENTED_EDGE('',*,*,#9330,.F.);
#12957=ORIENTED_EDGE('',*,*,#9333,.F.);
#12958=ORIENTED_EDGE('',*,*,#9337,.F.);
#12959=ORIENTED_EDGE('',*,*,#9340,.F.);
#12960=ORIENTED_EDGE('',*,*,#9343,.F.);
#12961=ORIENTED_EDGE('',*,*,#9346,.F.);
#12962=ORIENTED_EDGE('',*,*,#9397,.F.);
#12963=ORIENTED_EDGE('',*,*,#9355,.F.);
#12964=ORIENTED_EDGE('',*,*,#9311,.F.);
#12965=ORIENTED_EDGE('',*,*,#9315,.F.);
#12966=ORIENTED_EDGE('',*,*,#9318,.F.);
#12967=ORIENTED_EDGE('',*,*,#9321,.F.);
#12968=ORIENTED_EDGE('',*,*,#9324,.F.);
#12969=ORIENTED_EDGE('',*,*,#9327,.F.);
#12970=ORIENTED_EDGE('',*,*,#9398,.F.);
#12971=ORIENTED_EDGE('',*,*,#9326,.T.);
#12972=ORIENTED_EDGE('',*,*,#9395,.T.);
#12973=ORIENTED_EDGE('',*,*,#9399,.F.);
#12974=ORIENTED_EDGE('',*,*,#9398,.T.);
#12975=ORIENTED_EDGE('',*,*,#9380,.F.);
#12976=ORIENTED_EDGE('',*,*,#9400,.T.);
#12977=ORIENTED_EDGE('',*,*,#9401,.T.);
#12978=ORIENTED_EDGE('',*,*,#9389,.F.);
#12979=ORIENTED_EDGE('',*,*,#9383,.F.);
#12980=ORIENTED_EDGE('',*,*,#9402,.T.);
#12981=ORIENTED_EDGE('',*,*,#9403,.T.);
#12982=ORIENTED_EDGE('',*,*,#9400,.F.);
#12983=ORIENTED_EDGE('',*,*,#9373,.F.);
#12984=ORIENTED_EDGE('',*,*,#9386,.T.);
#12985=ORIENTED_EDGE('',*,*,#9404,.T.);
#12986=ORIENTED_EDGE('',*,*,#9402,.F.);
#12987=ORIENTED_EDGE('',*,*,#9388,.F.);
#12988=ORIENTED_EDGE('',*,*,#9390,.F.);
#12989=ORIENTED_EDGE('',*,*,#9401,.F.);
#12990=ORIENTED_EDGE('',*,*,#9403,.F.);
#12991=ORIENTED_EDGE('',*,*,#9404,.F.);
#12992=ORIENTED_EDGE('',*,*,#9385,.F.);
#12993=ORIENTED_EDGE('',*,*,#9405,.F.);
#12994=ORIENTED_EDGE('',*,*,#9406,.T.);
#12995=ORIENTED_EDGE('',*,*,#9392,.T.);
#12996=ORIENTED_EDGE('',*,*,#9399,.T.);
#12997=ORIENTED_EDGE('',*,*,#9393,.T.);
#12998=ORIENTED_EDGE('',*,*,#9406,.F.);
#12999=ORIENTED_EDGE('',*,*,#9405,.T.);
#13000=ORIENTED_EDGE('',*,*,#9407,.F.);
#13001=ORIENTED_EDGE('',*,*,#9408,.F.);
#13002=ORIENTED_EDGE('',*,*,#9409,.F.);
#13003=ORIENTED_EDGE('',*,*,#9410,.F.);
#13004=ORIENTED_EDGE('',*,*,#9411,.F.);
#13005=ORIENTED_EDGE('',*,*,#9412,.F.);
#13006=ORIENTED_EDGE('',*,*,#9413,.F.);
#13007=ORIENTED_EDGE('',*,*,#9414,.F.);
#13008=ORIENTED_EDGE('',*,*,#9415,.T.);
#13009=ORIENTED_EDGE('',*,*,#9408,.T.);
#13010=ORIENTED_EDGE('',*,*,#9416,.T.);
#13011=ORIENTED_EDGE('',*,*,#9417,.F.);
#13012=ORIENTED_EDGE('',*,*,#9418,.F.);
#13013=ORIENTED_EDGE('',*,*,#9409,.T.);
#13014=ORIENTED_EDGE('',*,*,#9418,.T.);
#13015=ORIENTED_EDGE('',*,*,#9419,.F.);
#13016=ORIENTED_EDGE('',*,*,#9420,.F.);
#13017=ORIENTED_EDGE('',*,*,#9410,.T.);
#13018=ORIENTED_EDGE('',*,*,#9420,.T.);
#13019=ORIENTED_EDGE('',*,*,#9421,.F.);
#13020=ORIENTED_EDGE('',*,*,#9422,.F.);
#13021=ORIENTED_EDGE('',*,*,#9411,.T.);
#13022=ORIENTED_EDGE('',*,*,#9422,.T.);
#13023=ORIENTED_EDGE('',*,*,#9423,.F.);
#13024=ORIENTED_EDGE('',*,*,#9424,.F.);
#13025=ORIENTED_EDGE('',*,*,#9412,.T.);
#13026=ORIENTED_EDGE('',*,*,#9424,.T.);
#13027=ORIENTED_EDGE('',*,*,#9425,.F.);
#13028=ORIENTED_EDGE('',*,*,#9426,.F.);
#13029=ORIENTED_EDGE('',*,*,#9413,.T.);
#13030=ORIENTED_EDGE('',*,*,#9426,.T.);
#13031=ORIENTED_EDGE('',*,*,#9427,.F.);
#13032=ORIENTED_EDGE('',*,*,#9428,.F.);
#13033=ORIENTED_EDGE('',*,*,#9414,.T.);
#13034=ORIENTED_EDGE('',*,*,#9428,.T.);
#13035=ORIENTED_EDGE('',*,*,#9429,.F.);
#13036=ORIENTED_EDGE('',*,*,#9430,.F.);
#13037=ORIENTED_EDGE('',*,*,#9407,.T.);
#13038=ORIENTED_EDGE('',*,*,#9430,.T.);
#13039=ORIENTED_EDGE('',*,*,#9431,.F.);
#13040=ORIENTED_EDGE('',*,*,#9416,.F.);
#13041=ORIENTED_EDGE('',*,*,#9431,.T.);
#13042=ORIENTED_EDGE('',*,*,#9429,.T.);
#13043=ORIENTED_EDGE('',*,*,#9427,.T.);
#13044=ORIENTED_EDGE('',*,*,#9425,.T.);
#13045=ORIENTED_EDGE('',*,*,#9423,.T.);
#13046=ORIENTED_EDGE('',*,*,#9421,.T.);
#13047=ORIENTED_EDGE('',*,*,#9419,.T.);
#13048=ORIENTED_EDGE('',*,*,#9417,.T.);
#13049=ORIENTED_EDGE('',*,*,#9415,.F.);
#13050=ORIENTED_EDGE('',*,*,#9432,.T.);
#13051=ORIENTED_EDGE('',*,*,#9433,.F.);
#13052=ORIENTED_EDGE('',*,*,#9434,.F.);
#13053=ORIENTED_EDGE('',*,*,#9435,.F.);
#13054=ORIENTED_EDGE('',*,*,#9432,.F.);
#13055=ORIENTED_EDGE('',*,*,#9434,.T.);
#13056=ORIENTED_EDGE('',*,*,#9436,.T.);
#13057=ORIENTED_EDGE('',*,*,#9437,.F.);
#13058=ORIENTED_EDGE('',*,*,#9438,.F.);
#13059=ORIENTED_EDGE('',*,*,#9439,.F.);
#13060=ORIENTED_EDGE('',*,*,#9440,.F.);
#13061=ORIENTED_EDGE('',*,*,#9441,.T.);
#13062=ORIENTED_EDGE('',*,*,#9442,.T.);
#13063=ORIENTED_EDGE('',*,*,#9443,.T.);
#13064=ORIENTED_EDGE('',*,*,#9443,.F.);
#13065=ORIENTED_EDGE('',*,*,#9444,.T.);
#13066=ORIENTED_EDGE('',*,*,#9445,.F.);
#13067=ORIENTED_EDGE('',*,*,#9444,.F.);
#13068=ORIENTED_EDGE('',*,*,#9446,.T.);
#13069=ORIENTED_EDGE('',*,*,#9447,.F.);
#13070=ORIENTED_EDGE('',*,*,#9448,.T.);
#13071=ORIENTED_EDGE('',*,*,#9449,.F.);
#13072=ORIENTED_EDGE('',*,*,#9450,.T.);
#13073=ORIENTED_EDGE('',*,*,#9451,.F.);
#13074=ORIENTED_EDGE('',*,*,#9452,.T.);
#13075=ORIENTED_EDGE('',*,*,#9453,.F.);
#13076=ORIENTED_EDGE('',*,*,#9454,.F.);
#13077=ORIENTED_EDGE('',*,*,#9438,.T.);
#13078=ORIENTED_EDGE('',*,*,#9455,.F.);
#13079=ORIENTED_EDGE('',*,*,#9456,.T.);
#13080=ORIENTED_EDGE('',*,*,#9457,.F.);
#13081=ORIENTED_EDGE('',*,*,#9458,.F.);
#13082=ORIENTED_EDGE('',*,*,#9459,.T.);
#13083=ORIENTED_EDGE('',*,*,#9453,.T.);
#13084=ORIENTED_EDGE('',*,*,#9460,.F.);
#13085=ORIENTED_EDGE('',*,*,#9449,.T.);
#13086=ORIENTED_EDGE('',*,*,#9461,.F.);
#13087=ORIENTED_EDGE('',*,*,#9447,.T.);
#13088=ORIENTED_EDGE('',*,*,#9462,.F.);
#13089=ORIENTED_EDGE('',*,*,#9451,.T.);
#13090=ORIENTED_EDGE('',*,*,#9463,.F.);
#13091=ORIENTED_EDGE('',*,*,#9455,.T.);
#13092=ORIENTED_EDGE('',*,*,#9464,.F.);
#13093=ORIENTED_EDGE('',*,*,#9457,.T.);
#13094=ORIENTED_EDGE('',*,*,#9465,.F.);
#13095=ORIENTED_EDGE('',*,*,#9454,.T.);
#13096=ORIENTED_EDGE('',*,*,#9459,.F.);
#13097=ORIENTED_EDGE('',*,*,#9466,.F.);
#13098=ORIENTED_EDGE('',*,*,#9467,.T.);
#13099=ORIENTED_EDGE('',*,*,#9458,.T.);
#13100=ORIENTED_EDGE('',*,*,#9467,.F.);
#13101=ORIENTED_EDGE('',*,*,#9466,.T.);
#13102=ORIENTED_EDGE('',*,*,#9445,.T.);
#13103=ORIENTED_EDGE('',*,*,#9462,.T.);
#13104=ORIENTED_EDGE('',*,*,#9468,.T.);
#13105=ORIENTED_EDGE('',*,*,#9469,.T.);
#13106=ORIENTED_EDGE('',*,*,#9463,.T.);
#13107=ORIENTED_EDGE('',*,*,#9470,.T.);
#13108=ORIENTED_EDGE('',*,*,#9439,.T.);
#13109=ORIENTED_EDGE('',*,*,#9461,.T.);
#13110=ORIENTED_EDGE('',*,*,#9471,.T.);
#13111=ORIENTED_EDGE('',*,*,#9472,.T.);
#13112=ORIENTED_EDGE('',*,*,#9464,.T.);
#13113=ORIENTED_EDGE('',*,*,#9437,.T.);
#13114=ORIENTED_EDGE('',*,*,#9473,.T.);
#13115=ORIENTED_EDGE('',*,*,#9460,.T.);
#13116=ORIENTED_EDGE('',*,*,#9474,.T.);
#13117=ORIENTED_EDGE('',*,*,#9475,.T.);
#13118=ORIENTED_EDGE('',*,*,#9476,.F.);
#13119=ORIENTED_EDGE('',*,*,#9477,.F.);
#13120=ORIENTED_EDGE('',*,*,#9478,.F.);
#13121=ORIENTED_EDGE('',*,*,#9479,.F.);
#13122=ORIENTED_EDGE('',*,*,#9441,.F.);
#13123=ORIENTED_EDGE('',*,*,#9480,.F.);
#13124=ORIENTED_EDGE('',*,*,#9481,.T.);
#13125=ORIENTED_EDGE('',*,*,#9477,.T.);
#13126=ORIENTED_EDGE('',*,*,#9482,.T.);
#13127=ORIENTED_EDGE('',*,*,#9471,.F.);
#13128=ORIENTED_EDGE('',*,*,#9448,.F.);
#13129=ORIENTED_EDGE('',*,*,#9475,.F.);
#13130=ORIENTED_EDGE('',*,*,#9483,.F.);
#13131=ORIENTED_EDGE('',*,*,#9478,.T.);
#13132=ORIENTED_EDGE('',*,*,#9483,.T.);
#13133=ORIENTED_EDGE('',*,*,#9474,.F.);
#13134=ORIENTED_EDGE('',*,*,#9452,.F.);
#13135=ORIENTED_EDGE('',*,*,#9484,.F.);
#13136=ORIENTED_EDGE('',*,*,#9485,.F.);
#13137=ORIENTED_EDGE('',*,*,#9433,.T.);
#13138=ORIENTED_EDGE('',*,*,#9435,.T.);
#13139=ORIENTED_EDGE('',*,*,#9442,.F.);
#13140=ORIENTED_EDGE('',*,*,#9479,.T.);
#13141=ORIENTED_EDGE('',*,*,#9485,.T.);
#13142=ORIENTED_EDGE('',*,*,#9486,.F.);
#13143=ORIENTED_EDGE('',*,*,#9456,.F.);
#13144=ORIENTED_EDGE('',*,*,#9473,.F.);
#13145=ORIENTED_EDGE('',*,*,#9436,.F.);
#13146=ORIENTED_EDGE('',*,*,#9480,.T.);
#13147=ORIENTED_EDGE('',*,*,#9440,.T.);
#13148=ORIENTED_EDGE('',*,*,#9470,.F.);
#13149=ORIENTED_EDGE('',*,*,#9450,.F.);
#13150=ORIENTED_EDGE('',*,*,#9469,.F.);
#13151=ORIENTED_EDGE('',*,*,#9487,.F.);
#13152=ORIENTED_EDGE('',*,*,#9476,.T.);
#13153=ORIENTED_EDGE('',*,*,#9487,.T.);
#13154=ORIENTED_EDGE('',*,*,#9468,.F.);
#13155=ORIENTED_EDGE('',*,*,#9446,.F.);
#13156=ORIENTED_EDGE('',*,*,#9472,.F.);
#13157=ORIENTED_EDGE('',*,*,#9482,.F.);
#13158=ORIENTED_EDGE('',*,*,#9465,.T.);
#13159=ORIENTED_EDGE('',*,*,#9486,.T.);
#13160=ORIENTED_EDGE('',*,*,#9484,.T.);
#13161=ORIENTED_EDGE('',*,*,#9488,.F.);
#13162=ORIENTED_EDGE('',*,*,#9489,.F.);
#13163=ORIENTED_EDGE('',*,*,#9490,.T.);
#13164=ORIENTED_EDGE('',*,*,#9488,.T.);
#13165=ORIENTED_EDGE('',*,*,#9490,.F.);
#13166=ORIENTED_EDGE('',*,*,#9481,.F.);
#13167=ORIENTED_EDGE('',*,*,#9491,.T.);
#13168=ORIENTED_EDGE('',*,*,#9489,.T.);
#13169=ORIENTED_EDGE('',*,*,#9491,.F.);
#13170=ORIENTED_EDGE('',*,*,#9492,.F.);
#13171=ORIENTED_EDGE('',*,*,#9493,.F.);
#13172=ORIENTED_EDGE('',*,*,#9494,.F.);
#13173=ORIENTED_EDGE('',*,*,#9495,.F.);
#13174=ORIENTED_EDGE('',*,*,#9496,.F.);
#13175=ORIENTED_EDGE('',*,*,#9497,.F.);
#13176=ORIENTED_EDGE('',*,*,#9498,.F.);
#13177=ORIENTED_EDGE('',*,*,#9499,.F.);
#13178=ORIENTED_EDGE('',*,*,#9500,.F.);
#13179=ORIENTED_EDGE('',*,*,#9494,.T.);
#13180=ORIENTED_EDGE('',*,*,#9501,.T.);
#13181=ORIENTED_EDGE('',*,*,#9499,.T.);
#13182=ORIENTED_EDGE('',*,*,#9502,.T.);
#13183=ORIENTED_EDGE('',*,*,#9503,.F.);
#13184=ORIENTED_EDGE('',*,*,#9504,.F.);
#13185=ORIENTED_EDGE('',*,*,#9505,.F.);
#13186=ORIENTED_EDGE('',*,*,#9506,.F.);
#13187=ORIENTED_EDGE('',*,*,#9507,.F.);
#13188=ORIENTED_EDGE('',*,*,#9508,.F.);
#13189=ORIENTED_EDGE('',*,*,#9509,.F.);
#13190=ORIENTED_EDGE('',*,*,#9510,.F.);
#13191=ORIENTED_EDGE('',*,*,#9511,.F.);
#13192=ORIENTED_EDGE('',*,*,#9507,.T.);
#13193=ORIENTED_EDGE('',*,*,#9512,.T.);
#13194=ORIENTED_EDGE('',*,*,#9510,.T.);
#13195=ORIENTED_EDGE('',*,*,#9513,.T.);
#13196=ORIENTED_EDGE('',*,*,#9511,.T.);
#13197=ORIENTED_EDGE('',*,*,#9514,.T.);
#13198=ORIENTED_EDGE('',*,*,#9504,.T.);
#13199=ORIENTED_EDGE('',*,*,#9515,.T.);
#13200=ORIENTED_EDGE('',*,*,#9516,.T.);
#13201=ORIENTED_EDGE('',*,*,#9517,.T.);
#13202=ORIENTED_EDGE('',*,*,#9509,.T.);
#13203=ORIENTED_EDGE('',*,*,#9518,.T.);
#13204=ORIENTED_EDGE('',*,*,#9519,.T.);
#13205=ORIENTED_EDGE('',*,*,#9520,.T.);
#13206=ORIENTED_EDGE('',*,*,#9508,.T.);
#13207=ORIENTED_EDGE('',*,*,#9521,.T.);
#13208=ORIENTED_EDGE('',*,*,#9500,.T.);
#13209=ORIENTED_EDGE('',*,*,#9522,.T.);
#13210=ORIENTED_EDGE('',*,*,#9506,.T.);
#13211=ORIENTED_EDGE('',*,*,#9523,.T.);
#13212=ORIENTED_EDGE('',*,*,#9505,.T.);
#13213=ORIENTED_EDGE('',*,*,#9524,.T.);
#13214=ORIENTED_EDGE('',*,*,#9496,.T.);
#13215=ORIENTED_EDGE('',*,*,#9525,.T.);
#13216=ORIENTED_EDGE('',*,*,#9526,.T.);
#13217=ORIENTED_EDGE('',*,*,#9527,.T.);
#13218=ORIENTED_EDGE('',*,*,#9503,.T.);
#13219=ORIENTED_EDGE('',*,*,#9528,.T.);
#13220=ORIENTED_EDGE('',*,*,#9529,.T.);
#13221=ORIENTED_EDGE('',*,*,#9530,.T.);
#13222=ORIENTED_EDGE('',*,*,#9498,.T.);
#13223=ORIENTED_EDGE('',*,*,#9531,.T.);
#13224=ORIENTED_EDGE('',*,*,#9497,.T.);
#13225=ORIENTED_EDGE('',*,*,#9532,.T.);
#13226=ORIENTED_EDGE('',*,*,#9493,.T.);
#13227=ORIENTED_EDGE('',*,*,#9533,.T.);
#13228=ORIENTED_EDGE('',*,*,#9534,.T.);
#13229=ORIENTED_EDGE('',*,*,#9535,.T.);
#13230=ORIENTED_EDGE('',*,*,#9495,.T.);
#13231=ORIENTED_EDGE('',*,*,#9536,.T.);
#13232=ORIENTED_EDGE('',*,*,#9537,.T.);
#13233=ORIENTED_EDGE('',*,*,#9538,.T.);
#13234=ORIENTED_EDGE('',*,*,#9492,.T.);
#13235=ORIENTED_EDGE('',*,*,#9539,.T.);
#13236=ORIENTED_EDGE('',*,*,#9518,.F.);
#13237=ORIENTED_EDGE('',*,*,#9515,.F.);
#13238=ORIENTED_EDGE('',*,*,#9527,.F.);
#13239=ORIENTED_EDGE('',*,*,#9540,.F.);
#13240=ORIENTED_EDGE('',*,*,#9528,.F.);
#13241=ORIENTED_EDGE('',*,*,#9525,.F.);
#13242=ORIENTED_EDGE('',*,*,#9535,.F.);
#13243=ORIENTED_EDGE('',*,*,#9541,.F.);
#13244=ORIENTED_EDGE('',*,*,#9536,.F.);
#13245=ORIENTED_EDGE('',*,*,#9533,.F.);
#13246=ORIENTED_EDGE('',*,*,#9538,.F.);
#13247=ORIENTED_EDGE('',*,*,#9542,.F.);
#13248=ORIENTED_EDGE('',*,*,#9512,.F.);
#13249=ORIENTED_EDGE('',*,*,#9522,.F.);
#13250=ORIENTED_EDGE('',*,*,#9501,.F.);
#13251=ORIENTED_EDGE('',*,*,#9532,.F.);
#13252=ORIENTED_EDGE('',*,*,#9524,.F.);
#13253=ORIENTED_EDGE('',*,*,#9514,.F.);
#13254=ORIENTED_EDGE('',*,*,#9543,.F.);
#13255=ORIENTED_EDGE('',*,*,#9544,.T.);
#13256=ORIENTED_EDGE('',*,*,#9545,.T.);
#13257=ORIENTED_EDGE('',*,*,#9546,.T.);
#13258=ORIENTED_EDGE('',*,*,#9547,.T.);
#13259=ORIENTED_EDGE('',*,*,#9548,.T.);
#13260=ORIENTED_EDGE('',*,*,#9546,.F.);
#13261=ORIENTED_EDGE('',*,*,#9547,.F.);
#13262=ORIENTED_EDGE('',*,*,#9548,.F.);
#13263=ORIENTED_EDGE('',*,*,#9549,.T.);
#13264=ORIENTED_EDGE('',*,*,#9550,.F.);
#13265=ORIENTED_EDGE('',*,*,#9551,.F.);
#13266=ORIENTED_EDGE('',*,*,#9549,.F.);
#13267=ORIENTED_EDGE('',*,*,#9552,.T.);
#13268=ORIENTED_EDGE('',*,*,#9553,.T.);
#13269=ORIENTED_EDGE('',*,*,#9544,.F.);
#13270=ORIENTED_EDGE('',*,*,#9545,.F.);
#13271=ORIENTED_EDGE('',*,*,#9553,.F.);
#13272=ORIENTED_EDGE('',*,*,#9550,.T.);
#13273=ORIENTED_EDGE('',*,*,#9551,.T.);
#13274=ORIENTED_EDGE('',*,*,#9554,.T.);
#13275=ORIENTED_EDGE('',*,*,#9555,.T.);
#13276=ORIENTED_EDGE('',*,*,#9554,.F.);
#13277=ORIENTED_EDGE('',*,*,#9555,.F.);
#13278=ORIENTED_EDGE('',*,*,#9556,.T.);
#13279=ORIENTED_EDGE('',*,*,#9557,.T.);
#13280=ORIENTED_EDGE('',*,*,#9558,.T.);
#13281=ORIENTED_EDGE('',*,*,#9559,.T.);
#13282=ORIENTED_EDGE('',*,*,#9557,.F.);
#13283=ORIENTED_EDGE('',*,*,#9558,.F.);
#13284=ORIENTED_EDGE('',*,*,#9559,.F.);
#13285=ORIENTED_EDGE('',*,*,#9560,.T.);
#13286=ORIENTED_EDGE('',*,*,#9561,.T.);
#13287=ORIENTED_EDGE('',*,*,#9560,.F.);
#13288=ORIENTED_EDGE('',*,*,#9556,.F.);
#13289=ORIENTED_EDGE('',*,*,#9562,.T.);
#13290=ORIENTED_EDGE('',*,*,#9519,.F.);
#13291=ORIENTED_EDGE('',*,*,#9563,.T.);
#13292=ORIENTED_EDGE('',*,*,#9516,.F.);
#13293=ORIENTED_EDGE('',*,*,#9540,.T.);
#13294=ORIENTED_EDGE('',*,*,#9526,.F.);
#13295=ORIENTED_EDGE('',*,*,#9541,.T.);
#13296=ORIENTED_EDGE('',*,*,#9534,.F.);
#13297=ORIENTED_EDGE('',*,*,#9542,.T.);
#13298=ORIENTED_EDGE('',*,*,#9537,.F.);
#13299=ORIENTED_EDGE('',*,*,#9564,.T.);
#13300=ORIENTED_EDGE('',*,*,#9529,.F.);
#13301=ORIENTED_EDGE('',*,*,#9552,.F.);
#13302=ORIENTED_EDGE('',*,*,#9565,.F.);
#13303=ORIENTED_EDGE('',*,*,#9566,.F.);
#13304=ORIENTED_EDGE('',*,*,#9567,.T.);
#13305=ORIENTED_EDGE('',*,*,#9565,.T.);
#13306=ORIENTED_EDGE('',*,*,#9568,.T.);
#13307=ORIENTED_EDGE('',*,*,#9567,.F.);
#13308=ORIENTED_EDGE('',*,*,#9568,.F.);
#13309=ORIENTED_EDGE('',*,*,#9569,.T.);
#13310=ORIENTED_EDGE('',*,*,#9570,.T.);
#13311=ORIENTED_EDGE('',*,*,#9566,.T.);
#13312=ORIENTED_EDGE('',*,*,#9570,.F.);
#13313=ORIENTED_EDGE('',*,*,#9569,.F.);
#13314=ORIENTED_EDGE('',*,*,#9571,.F.);
#13315=ORIENTED_EDGE('',*,*,#9561,.F.);
#13316=ORIENTED_EDGE('',*,*,#9572,.T.);
#13317=ORIENTED_EDGE('',*,*,#9571,.T.);
#13318=ORIENTED_EDGE('',*,*,#9573,.T.);
#13319=ORIENTED_EDGE('',*,*,#9572,.F.);
#13320=ORIENTED_EDGE('',*,*,#9573,.F.);
#13321=ORIENTED_EDGE('',*,*,#9520,.F.);
#13322=ORIENTED_EDGE('',*,*,#9562,.F.);
#13323=ORIENTED_EDGE('',*,*,#9531,.F.);
#13324=ORIENTED_EDGE('',*,*,#9523,.F.);
#13325=ORIENTED_EDGE('',*,*,#9530,.F.);
#13326=ORIENTED_EDGE('',*,*,#9564,.F.);
#13327=ORIENTED_EDGE('',*,*,#9539,.F.);
#13328=ORIENTED_EDGE('',*,*,#9502,.F.);
#13329=ORIENTED_EDGE('',*,*,#9517,.F.);
#13330=ORIENTED_EDGE('',*,*,#9563,.F.);
#13331=ORIENTED_EDGE('',*,*,#9521,.F.);
#13332=ORIENTED_EDGE('',*,*,#9513,.F.);
#13333=ORIENTED_EDGE('',*,*,#9574,.F.);
#13334=ORIENTED_EDGE('',*,*,#9575,.T.);
#13335=ORIENTED_EDGE('',*,*,#9543,.T.);
#13336=ORIENTED_EDGE('',*,*,#9575,.F.);
#13337=ORIENTED_EDGE('',*,*,#9576,.F.);
#13338=ORIENTED_EDGE('',*,*,#9577,.T.);
#13339=ORIENTED_EDGE('',*,*,#9574,.T.);
#13340=ORIENTED_EDGE('',*,*,#9577,.F.);
#13341=ORIENTED_EDGE('',*,*,#9576,.T.);
#13342=ORIENTED_EDGE('',*,*,#9578,.T.);
#13343=ORIENTED_EDGE('',*,*,#9578,.F.);
#13344=ORIENTED_EDGE('',*,*,#9579,.T.);
#13345=ORIENTED_EDGE('',*,*,#9580,.T.);
#13346=ORIENTED_EDGE('',*,*,#9581,.F.);
#13347=ORIENTED_EDGE('',*,*,#9580,.F.);
#13348=ORIENTED_EDGE('',*,*,#9582,.F.);
#13349=ORIENTED_EDGE('',*,*,#9581,.T.);
#13350=ORIENTED_EDGE('',*,*,#9583,.F.);
#13351=ORIENTED_EDGE('',*,*,#9584,.T.);
#13352=ORIENTED_EDGE('',*,*,#9582,.T.);
#13353=ORIENTED_EDGE('',*,*,#9584,.F.);
#13354=ORIENTED_EDGE('',*,*,#9585,.F.);
#13355=ORIENTED_EDGE('',*,*,#9586,.T.);
#13356=ORIENTED_EDGE('',*,*,#9583,.T.);
#13357=ORIENTED_EDGE('',*,*,#9586,.F.);
#13358=ORIENTED_EDGE('',*,*,#9587,.F.);
#13359=ORIENTED_EDGE('',*,*,#9588,.T.);
#13360=ORIENTED_EDGE('',*,*,#9585,.T.);
#13361=ORIENTED_EDGE('',*,*,#9588,.F.);
#13362=ORIENTED_EDGE('',*,*,#9587,.T.);
#13363=ORIENTED_EDGE('',*,*,#9579,.F.);
#13364=ORIENTED_EDGE('',*,*,#9589,.T.);
#13365=ORIENTED_EDGE('',*,*,#9590,.T.);
#13366=ORIENTED_EDGE('',*,*,#9591,.T.);
#13367=ORIENTED_EDGE('',*,*,#9590,.F.);
#13368=ORIENTED_EDGE('',*,*,#9592,.F.);
#13369=ORIENTED_EDGE('',*,*,#9593,.F.);
#13370=ORIENTED_EDGE('',*,*,#9594,.F.);
#13371=ORIENTED_EDGE('',*,*,#9595,.F.);
#13372=ORIENTED_EDGE('',*,*,#9596,.F.);
#13373=ORIENTED_EDGE('',*,*,#9597,.T.);
#13374=ORIENTED_EDGE('',*,*,#9598,.T.);
#13375=ORIENTED_EDGE('',*,*,#9599,.T.);
#13376=ORIENTED_EDGE('',*,*,#9600,.T.);
#13377=ORIENTED_EDGE('',*,*,#9589,.F.);
#13378=ORIENTED_EDGE('',*,*,#9601,.F.);
#13379=ORIENTED_EDGE('',*,*,#9602,.T.);
#13380=ORIENTED_EDGE('',*,*,#9591,.F.);
#13381=ORIENTED_EDGE('',*,*,#9602,.F.);
#13382=ORIENTED_EDGE('',*,*,#9596,.T.);
#13383=ORIENTED_EDGE('',*,*,#9603,.T.);
#13384=ORIENTED_EDGE('',*,*,#9604,.T.);
#13385=ORIENTED_EDGE('',*,*,#9603,.F.);
#13386=ORIENTED_EDGE('',*,*,#9605,.F.);
#13387=ORIENTED_EDGE('',*,*,#9606,.T.);
#13388=ORIENTED_EDGE('',*,*,#9604,.F.);
#13389=ORIENTED_EDGE('',*,*,#9606,.F.);
#13390=ORIENTED_EDGE('',*,*,#9607,.T.);
#13391=ORIENTED_EDGE('',*,*,#9608,.T.);
#13392=ORIENTED_EDGE('',*,*,#9609,.T.);
#13393=ORIENTED_EDGE('',*,*,#9610,.T.);
#13394=ORIENTED_EDGE('',*,*,#9607,.F.);
#13395=ORIENTED_EDGE('',*,*,#9611,.T.);
#13396=ORIENTED_EDGE('',*,*,#9612,.T.);
#13397=ORIENTED_EDGE('',*,*,#9613,.T.);
#13398=ORIENTED_EDGE('',*,*,#9614,.T.);
#13399=ORIENTED_EDGE('',*,*,#9615,.T.);
#13400=ORIENTED_EDGE('',*,*,#9612,.F.);
#13401=ORIENTED_EDGE('',*,*,#9616,.T.);
#13402=ORIENTED_EDGE('',*,*,#9614,.F.);
#13403=ORIENTED_EDGE('',*,*,#9617,.T.);
#13404=ORIENTED_EDGE('',*,*,#9618,.T.);
#13405=ORIENTED_EDGE('',*,*,#9619,.T.);
#13406=ORIENTED_EDGE('',*,*,#9620,.T.);
#13407=ORIENTED_EDGE('',*,*,#9621,.T.);
#13408=ORIENTED_EDGE('',*,*,#9618,.F.);
#13409=ORIENTED_EDGE('',*,*,#9622,.T.);
#13410=ORIENTED_EDGE('',*,*,#9620,.F.);
#13411=ORIENTED_EDGE('',*,*,#9623,.T.);
#13412=ORIENTED_EDGE('',*,*,#9624,.T.);
#13413=ORIENTED_EDGE('',*,*,#9625,.T.);
#13414=ORIENTED_EDGE('',*,*,#9626,.T.);
#13415=ORIENTED_EDGE('',*,*,#9627,.T.);
#13416=ORIENTED_EDGE('',*,*,#9624,.F.);
#13417=ORIENTED_EDGE('',*,*,#9628,.T.);
#13418=ORIENTED_EDGE('',*,*,#9626,.F.);
#13419=ORIENTED_EDGE('',*,*,#9629,.T.);
#13420=ORIENTED_EDGE('',*,*,#9630,.T.);
#13421=ORIENTED_EDGE('',*,*,#9631,.T.);
#13422=ORIENTED_EDGE('',*,*,#9632,.T.);
#13423=ORIENTED_EDGE('',*,*,#9633,.T.);
#13424=ORIENTED_EDGE('',*,*,#9630,.F.);
#13425=ORIENTED_EDGE('',*,*,#9592,.T.);
#13426=ORIENTED_EDGE('',*,*,#9632,.F.);
#13427=ORIENTED_EDGE('',*,*,#9634,.T.);
#13428=ORIENTED_EDGE('',*,*,#9635,.T.);
#13429=ORIENTED_EDGE('',*,*,#9636,.T.);
#13430=ORIENTED_EDGE('',*,*,#9637,.T.);
#13431=ORIENTED_EDGE('',*,*,#9638,.T.);
#13432=ORIENTED_EDGE('',*,*,#9635,.F.);
#13433=ORIENTED_EDGE('',*,*,#9639,.T.);
#13434=ORIENTED_EDGE('',*,*,#9637,.F.);
#13435=ORIENTED_EDGE('',*,*,#9640,.T.);
#13436=ORIENTED_EDGE('',*,*,#9641,.T.);
#13437=ORIENTED_EDGE('',*,*,#9642,.T.);
#13438=ORIENTED_EDGE('',*,*,#9643,.T.);
#13439=ORIENTED_EDGE('',*,*,#9644,.T.);
#13440=ORIENTED_EDGE('',*,*,#9641,.F.);
#13441=ORIENTED_EDGE('',*,*,#9645,.T.);
#13442=ORIENTED_EDGE('',*,*,#9643,.F.);
#13443=ORIENTED_EDGE('',*,*,#9646,.T.);
#13444=ORIENTED_EDGE('',*,*,#9647,.T.);
#13445=ORIENTED_EDGE('',*,*,#9648,.T.);
#13446=ORIENTED_EDGE('',*,*,#9649,.T.);
#13447=ORIENTED_EDGE('',*,*,#9650,.T.);
#13448=ORIENTED_EDGE('',*,*,#9647,.F.);
#13449=ORIENTED_EDGE('',*,*,#9651,.T.);
#13450=ORIENTED_EDGE('',*,*,#9649,.F.);
#13451=ORIENTED_EDGE('',*,*,#9652,.T.);
#13452=ORIENTED_EDGE('',*,*,#9609,.F.);
#13453=ORIENTED_EDGE('',*,*,#9653,.T.);
#13454=ORIENTED_EDGE('',*,*,#9629,.F.);
#13455=ORIENTED_EDGE('',*,*,#9654,.T.);
#13456=ORIENTED_EDGE('',*,*,#9655,.F.);
#13457=ORIENTED_EDGE('',*,*,#9593,.T.);
#13458=ORIENTED_EDGE('',*,*,#9628,.F.);
#13459=ORIENTED_EDGE('',*,*,#9656,.F.);
#13460=ORIENTED_EDGE('',*,*,#9657,.F.);
#13461=ORIENTED_EDGE('',*,*,#9654,.F.);
#13462=ORIENTED_EDGE('',*,*,#9623,.F.);
#13463=ORIENTED_EDGE('',*,*,#9658,.T.);
#13464=ORIENTED_EDGE('',*,*,#9659,.F.);
#13465=ORIENTED_EDGE('',*,*,#9656,.T.);
#13466=ORIENTED_EDGE('',*,*,#9622,.F.);
#13467=ORIENTED_EDGE('',*,*,#9660,.F.);
#13468=ORIENTED_EDGE('',*,*,#9661,.F.);
#13469=ORIENTED_EDGE('',*,*,#9658,.F.);
#13470=ORIENTED_EDGE('',*,*,#9617,.F.);
#13471=ORIENTED_EDGE('',*,*,#9662,.T.);
#13472=ORIENTED_EDGE('',*,*,#9663,.F.);
#13473=ORIENTED_EDGE('',*,*,#9660,.T.);
#13474=ORIENTED_EDGE('',*,*,#9616,.F.);
#13475=ORIENTED_EDGE('',*,*,#9664,.F.);
#13476=ORIENTED_EDGE('',*,*,#9665,.F.);
#13477=ORIENTED_EDGE('',*,*,#9662,.F.);
#13478=ORIENTED_EDGE('',*,*,#9611,.F.);
#13479=ORIENTED_EDGE('',*,*,#9666,.T.);
#13480=ORIENTED_EDGE('',*,*,#9667,.F.);
#13481=ORIENTED_EDGE('',*,*,#9664,.T.);
#13482=ORIENTED_EDGE('',*,*,#9610,.F.);
#13483=ORIENTED_EDGE('',*,*,#9668,.F.);
#13484=ORIENTED_EDGE('',*,*,#9669,.F.);
#13485=ORIENTED_EDGE('',*,*,#9666,.F.);
#13486=ORIENTED_EDGE('',*,*,#9670,.F.);
#13487=ORIENTED_EDGE('',*,*,#9671,.T.);
#13488=ORIENTED_EDGE('',*,*,#9672,.T.);
#13489=ORIENTED_EDGE('',*,*,#9673,.T.);
#13490=ORIENTED_EDGE('',*,*,#9674,.T.);
#13491=ORIENTED_EDGE('',*,*,#9675,.F.);
#13492=ORIENTED_EDGE('',*,*,#9608,.F.);
#13493=ORIENTED_EDGE('',*,*,#9613,.F.);
#13494=ORIENTED_EDGE('',*,*,#9615,.F.);
#13495=ORIENTED_EDGE('',*,*,#9619,.F.);
#13496=ORIENTED_EDGE('',*,*,#9621,.F.);
#13497=ORIENTED_EDGE('',*,*,#9625,.F.);
#13498=ORIENTED_EDGE('',*,*,#9627,.F.);
#13499=ORIENTED_EDGE('',*,*,#9631,.F.);
#13500=ORIENTED_EDGE('',*,*,#9633,.F.);
#13501=ORIENTED_EDGE('',*,*,#9636,.F.);
#13502=ORIENTED_EDGE('',*,*,#9638,.F.);
#13503=ORIENTED_EDGE('',*,*,#9642,.F.);
#13504=ORIENTED_EDGE('',*,*,#9644,.F.);
#13505=ORIENTED_EDGE('',*,*,#9648,.F.);
#13506=ORIENTED_EDGE('',*,*,#9650,.F.);
#13507=ORIENTED_EDGE('',*,*,#9653,.F.);
#13508=ORIENTED_EDGE('',*,*,#9676,.T.);
#13509=ORIENTED_EDGE('',*,*,#9677,.T.);
#13510=ORIENTED_EDGE('',*,*,#9678,.T.);
#13511=ORIENTED_EDGE('',*,*,#9669,.T.);
#13512=ORIENTED_EDGE('',*,*,#9676,.F.);
#13513=ORIENTED_EDGE('',*,*,#9679,.T.);
#13514=ORIENTED_EDGE('',*,*,#9680,.T.);
#13515=ORIENTED_EDGE('',*,*,#9681,.T.);
#13516=ORIENTED_EDGE('',*,*,#9682,.T.);
#13517=ORIENTED_EDGE('',*,*,#9683,.T.);
#13518=ORIENTED_EDGE('',*,*,#9680,.F.);
#13519=ORIENTED_EDGE('',*,*,#9684,.T.);
#13520=ORIENTED_EDGE('',*,*,#9682,.F.);
#13521=ORIENTED_EDGE('',*,*,#9685,.T.);
#13522=ORIENTED_EDGE('',*,*,#9686,.T.);
#13523=ORIENTED_EDGE('',*,*,#9687,.T.);
#13524=ORIENTED_EDGE('',*,*,#9688,.T.);
#13525=ORIENTED_EDGE('',*,*,#9689,.T.);
#13526=ORIENTED_EDGE('',*,*,#9686,.F.);
#13527=ORIENTED_EDGE('',*,*,#9690,.T.);
#13528=ORIENTED_EDGE('',*,*,#9688,.F.);
#13529=ORIENTED_EDGE('',*,*,#9691,.T.);
#13530=ORIENTED_EDGE('',*,*,#9692,.T.);
#13531=ORIENTED_EDGE('',*,*,#9693,.T.);
#13532=ORIENTED_EDGE('',*,*,#9694,.T.);
#13533=ORIENTED_EDGE('',*,*,#9695,.T.);
#13534=ORIENTED_EDGE('',*,*,#9692,.F.);
#13535=ORIENTED_EDGE('',*,*,#9696,.T.);
#13536=ORIENTED_EDGE('',*,*,#9694,.F.);
#13537=ORIENTED_EDGE('',*,*,#9697,.T.);
#13538=ORIENTED_EDGE('',*,*,#9698,.T.);
#13539=ORIENTED_EDGE('',*,*,#9699,.T.);
#13540=ORIENTED_EDGE('',*,*,#9700,.T.);
#13541=ORIENTED_EDGE('',*,*,#9701,.T.);
#13542=ORIENTED_EDGE('',*,*,#9698,.F.);
#13543=ORIENTED_EDGE('',*,*,#9594,.T.);
#13544=ORIENTED_EDGE('',*,*,#9700,.F.);
#13545=ORIENTED_EDGE('',*,*,#9655,.T.);
#13546=ORIENTED_EDGE('',*,*,#9702,.T.);
#13547=ORIENTED_EDGE('',*,*,#9703,.T.);
#13548=ORIENTED_EDGE('',*,*,#9704,.T.);
#13549=ORIENTED_EDGE('',*,*,#9705,.T.);
#13550=ORIENTED_EDGE('',*,*,#9702,.F.);
#13551=ORIENTED_EDGE('',*,*,#9657,.T.);
#13552=ORIENTED_EDGE('',*,*,#9704,.F.);
#13553=ORIENTED_EDGE('',*,*,#9659,.T.);
#13554=ORIENTED_EDGE('',*,*,#9706,.T.);
#13555=ORIENTED_EDGE('',*,*,#9707,.T.);
#13556=ORIENTED_EDGE('',*,*,#9708,.T.);
#13557=ORIENTED_EDGE('',*,*,#9709,.T.);
#13558=ORIENTED_EDGE('',*,*,#9706,.F.);
#13559=ORIENTED_EDGE('',*,*,#9661,.T.);
#13560=ORIENTED_EDGE('',*,*,#9708,.F.);
#13561=ORIENTED_EDGE('',*,*,#9663,.T.);
#13562=ORIENTED_EDGE('',*,*,#9710,.T.);
#13563=ORIENTED_EDGE('',*,*,#9711,.T.);
#13564=ORIENTED_EDGE('',*,*,#9712,.T.);
#13565=ORIENTED_EDGE('',*,*,#9713,.T.);
#13566=ORIENTED_EDGE('',*,*,#9710,.F.);
#13567=ORIENTED_EDGE('',*,*,#9665,.T.);
#13568=ORIENTED_EDGE('',*,*,#9712,.F.);
#13569=ORIENTED_EDGE('',*,*,#9667,.T.);
#13570=ORIENTED_EDGE('',*,*,#9678,.F.);
#13571=ORIENTED_EDGE('',*,*,#9714,.T.);
#13572=ORIENTED_EDGE('',*,*,#9634,.F.);
#13573=ORIENTED_EDGE('',*,*,#9595,.T.);
#13574=ORIENTED_EDGE('',*,*,#9697,.F.);
#13575=ORIENTED_EDGE('',*,*,#9715,.T.);
#13576=ORIENTED_EDGE('',*,*,#9639,.F.);
#13577=ORIENTED_EDGE('',*,*,#9715,.F.);
#13578=ORIENTED_EDGE('',*,*,#9696,.F.);
#13579=ORIENTED_EDGE('',*,*,#9716,.F.);
#13580=ORIENTED_EDGE('',*,*,#9640,.F.);
#13581=ORIENTED_EDGE('',*,*,#9716,.T.);
#13582=ORIENTED_EDGE('',*,*,#9691,.F.);
#13583=ORIENTED_EDGE('',*,*,#9717,.T.);
#13584=ORIENTED_EDGE('',*,*,#9645,.F.);
#13585=ORIENTED_EDGE('',*,*,#9717,.F.);
#13586=ORIENTED_EDGE('',*,*,#9690,.F.);
#13587=ORIENTED_EDGE('',*,*,#9718,.F.);
#13588=ORIENTED_EDGE('',*,*,#9646,.F.);
#13589=ORIENTED_EDGE('',*,*,#9718,.T.);
#13590=ORIENTED_EDGE('',*,*,#9685,.F.);
#13591=ORIENTED_EDGE('',*,*,#9719,.T.);
#13592=ORIENTED_EDGE('',*,*,#9651,.F.);
#13593=ORIENTED_EDGE('',*,*,#9719,.F.);
#13594=ORIENTED_EDGE('',*,*,#9684,.F.);
#13595=ORIENTED_EDGE('',*,*,#9720,.F.);
#13596=ORIENTED_EDGE('',*,*,#9652,.F.);
#13597=ORIENTED_EDGE('',*,*,#9720,.T.);
#13598=ORIENTED_EDGE('',*,*,#9679,.F.);
#13599=ORIENTED_EDGE('',*,*,#9668,.T.);
#13600=ORIENTED_EDGE('',*,*,#9677,.F.);
#13601=ORIENTED_EDGE('',*,*,#9681,.F.);
#13602=ORIENTED_EDGE('',*,*,#9683,.F.);
#13603=ORIENTED_EDGE('',*,*,#9687,.F.);
#13604=ORIENTED_EDGE('',*,*,#9689,.F.);
#13605=ORIENTED_EDGE('',*,*,#9693,.F.);
#13606=ORIENTED_EDGE('',*,*,#9695,.F.);
#13607=ORIENTED_EDGE('',*,*,#9699,.F.);
#13608=ORIENTED_EDGE('',*,*,#9701,.F.);
#13609=ORIENTED_EDGE('',*,*,#9703,.F.);
#13610=ORIENTED_EDGE('',*,*,#9705,.F.);
#13611=ORIENTED_EDGE('',*,*,#9707,.F.);
#13612=ORIENTED_EDGE('',*,*,#9709,.F.);
#13613=ORIENTED_EDGE('',*,*,#9711,.F.);
#13614=ORIENTED_EDGE('',*,*,#9713,.F.);
#13615=ORIENTED_EDGE('',*,*,#9714,.F.);
#13616=ORIENTED_EDGE('',*,*,#9675,.T.);
#13617=ORIENTED_EDGE('',*,*,#9721,.T.);
#13618=ORIENTED_EDGE('',*,*,#9605,.T.);
#13619=ORIENTED_EDGE('',*,*,#9721,.F.);
#13620=ORIENTED_EDGE('',*,*,#9670,.T.);
#13621=ORIENTED_EDGE('',*,*,#9722,.T.);
#13622=ORIENTED_EDGE('',*,*,#9601,.T.);
#13623=ORIENTED_EDGE('',*,*,#9722,.F.);
#13624=ORIENTED_EDGE('',*,*,#9671,.F.);
#13625=ORIENTED_EDGE('',*,*,#9723,.T.);
#13626=ORIENTED_EDGE('',*,*,#9600,.F.);
#13627=ORIENTED_EDGE('',*,*,#9723,.F.);
#13628=ORIENTED_EDGE('',*,*,#9672,.F.);
#13629=ORIENTED_EDGE('',*,*,#9724,.T.);
#13630=ORIENTED_EDGE('',*,*,#9599,.F.);
#13631=ORIENTED_EDGE('',*,*,#9724,.F.);
#13632=ORIENTED_EDGE('',*,*,#9673,.F.);
#13633=ORIENTED_EDGE('',*,*,#9725,.T.);
#13634=ORIENTED_EDGE('',*,*,#9598,.F.);
#13635=ORIENTED_EDGE('',*,*,#9725,.F.);
#13636=ORIENTED_EDGE('',*,*,#9674,.F.);
#13637=ORIENTED_EDGE('',*,*,#9726,.T.);
#13638=ORIENTED_EDGE('',*,*,#9597,.F.);
#13639=ORIENTED_EDGE('',*,*,#9726,.F.);
#13640=ORIENTED_EDGE('',*,*,#9727,.F.);
#13641=ORIENTED_EDGE('',*,*,#9728,.T.);
#13642=ORIENTED_EDGE('',*,*,#9729,.T.);
#13643=ORIENTED_EDGE('',*,*,#9730,.T.);
#13644=ORIENTED_EDGE('',*,*,#9731,.F.);
#13645=ORIENTED_EDGE('',*,*,#9732,.T.);
#13646=ORIENTED_EDGE('',*,*,#9727,.T.);
#13647=ORIENTED_EDGE('',*,*,#9733,.T.);
#13648=ORIENTED_EDGE('',*,*,#9734,.F.);
#13649=ORIENTED_EDGE('',*,*,#9735,.T.);
#13650=ORIENTED_EDGE('',*,*,#9731,.T.);
#13651=ORIENTED_EDGE('',*,*,#9736,.T.);
#13652=ORIENTED_EDGE('',*,*,#9737,.F.);
#13653=ORIENTED_EDGE('',*,*,#9738,.T.);
#13654=ORIENTED_EDGE('',*,*,#9734,.T.);
#13655=ORIENTED_EDGE('',*,*,#9739,.T.);
#13656=ORIENTED_EDGE('',*,*,#9740,.F.);
#13657=ORIENTED_EDGE('',*,*,#9741,.T.);
#13658=ORIENTED_EDGE('',*,*,#9737,.T.);
#13659=ORIENTED_EDGE('',*,*,#9742,.T.);
#13660=ORIENTED_EDGE('',*,*,#9743,.F.);
#13661=ORIENTED_EDGE('',*,*,#9744,.T.);
#13662=ORIENTED_EDGE('',*,*,#9740,.T.);
#13663=ORIENTED_EDGE('',*,*,#9745,.T.);
#13664=ORIENTED_EDGE('',*,*,#9746,.F.);
#13665=ORIENTED_EDGE('',*,*,#9747,.T.);
#13666=ORIENTED_EDGE('',*,*,#9743,.T.);
#13667=ORIENTED_EDGE('',*,*,#9748,.T.);
#13668=ORIENTED_EDGE('',*,*,#9749,.F.);
#13669=ORIENTED_EDGE('',*,*,#9750,.T.);
#13670=ORIENTED_EDGE('',*,*,#9746,.T.);
#13671=ORIENTED_EDGE('',*,*,#9751,.T.);
#13672=ORIENTED_EDGE('',*,*,#9752,.F.);
#13673=ORIENTED_EDGE('',*,*,#9753,.T.);
#13674=ORIENTED_EDGE('',*,*,#9749,.T.);
#13675=ORIENTED_EDGE('',*,*,#9754,.T.);
#13676=ORIENTED_EDGE('',*,*,#9755,.F.);
#13677=ORIENTED_EDGE('',*,*,#9756,.F.);
#13678=ORIENTED_EDGE('',*,*,#9757,.T.);
#13679=ORIENTED_EDGE('',*,*,#9752,.T.);
#13680=ORIENTED_EDGE('',*,*,#9758,.T.);
#13681=ORIENTED_EDGE('',*,*,#9759,.F.);
#13682=ORIENTED_EDGE('',*,*,#9760,.T.);
#13683=ORIENTED_EDGE('',*,*,#9761,.F.);
#13684=ORIENTED_EDGE('',*,*,#9762,.F.);
#13685=ORIENTED_EDGE('',*,*,#9763,.F.);
#13686=ORIENTED_EDGE('',*,*,#9764,.T.);
#13687=ORIENTED_EDGE('',*,*,#9759,.T.);
#13688=ORIENTED_EDGE('',*,*,#9765,.F.);
#13689=ORIENTED_EDGE('',*,*,#9766,.F.);
#13690=ORIENTED_EDGE('',*,*,#9767,.T.);
#13691=ORIENTED_EDGE('',*,*,#9763,.T.);
#13692=ORIENTED_EDGE('',*,*,#9768,.F.);
#13693=ORIENTED_EDGE('',*,*,#9769,.F.);
#13694=ORIENTED_EDGE('',*,*,#9770,.T.);
#13695=ORIENTED_EDGE('',*,*,#9766,.T.);
#13696=ORIENTED_EDGE('',*,*,#9771,.F.);
#13697=ORIENTED_EDGE('',*,*,#9772,.F.);
#13698=ORIENTED_EDGE('',*,*,#9773,.T.);
#13699=ORIENTED_EDGE('',*,*,#9769,.T.);
#13700=ORIENTED_EDGE('',*,*,#9774,.F.);
#13701=ORIENTED_EDGE('',*,*,#9775,.F.);
#13702=ORIENTED_EDGE('',*,*,#9776,.T.);
#13703=ORIENTED_EDGE('',*,*,#9772,.T.);
#13704=ORIENTED_EDGE('',*,*,#9777,.F.);
#13705=ORIENTED_EDGE('',*,*,#9778,.F.);
#13706=ORIENTED_EDGE('',*,*,#9779,.T.);
#13707=ORIENTED_EDGE('',*,*,#9775,.T.);
#13708=ORIENTED_EDGE('',*,*,#9780,.F.);
#13709=ORIENTED_EDGE('',*,*,#9781,.F.);
#13710=ORIENTED_EDGE('',*,*,#9782,.T.);
#13711=ORIENTED_EDGE('',*,*,#9778,.T.);
#13712=ORIENTED_EDGE('',*,*,#9783,.F.);
#13713=ORIENTED_EDGE('',*,*,#9784,.F.);
#13714=ORIENTED_EDGE('',*,*,#9785,.T.);
#13715=ORIENTED_EDGE('',*,*,#9781,.T.);
#13716=ORIENTED_EDGE('',*,*,#9786,.F.);
#13717=ORIENTED_EDGE('',*,*,#9787,.T.);
#13718=ORIENTED_EDGE('',*,*,#9788,.T.);
#13719=ORIENTED_EDGE('',*,*,#9789,.T.);
#13720=ORIENTED_EDGE('',*,*,#9790,.T.);
#13721=ORIENTED_EDGE('',*,*,#9791,.T.);
#13722=ORIENTED_EDGE('',*,*,#9789,.F.);
#13723=ORIENTED_EDGE('',*,*,#9790,.F.);
#13724=ORIENTED_EDGE('',*,*,#9791,.F.);
#13725=ORIENTED_EDGE('',*,*,#9792,.T.);
#13726=ORIENTED_EDGE('',*,*,#9793,.F.);
#13727=ORIENTED_EDGE('',*,*,#9794,.F.);
#13728=ORIENTED_EDGE('',*,*,#9792,.F.);
#13729=ORIENTED_EDGE('',*,*,#9795,.F.);
#13730=ORIENTED_EDGE('',*,*,#9796,.T.);
#13731=ORIENTED_EDGE('',*,*,#9787,.F.);
#13732=ORIENTED_EDGE('',*,*,#9788,.F.);
#13733=ORIENTED_EDGE('',*,*,#9796,.F.);
#13734=ORIENTED_EDGE('',*,*,#9793,.T.);
#13735=ORIENTED_EDGE('',*,*,#9794,.T.);
#13736=ORIENTED_EDGE('',*,*,#9797,.T.);
#13737=ORIENTED_EDGE('',*,*,#9798,.T.);
#13738=ORIENTED_EDGE('',*,*,#9797,.F.);
#13739=ORIENTED_EDGE('',*,*,#9798,.F.);
#13740=ORIENTED_EDGE('',*,*,#9761,.T.);
#13741=ORIENTED_EDGE('',*,*,#9799,.T.);
#13742=ORIENTED_EDGE('',*,*,#9800,.F.);
#13743=ORIENTED_EDGE('',*,*,#9801,.T.);
#13744=ORIENTED_EDGE('',*,*,#9801,.F.);
#13745=ORIENTED_EDGE('',*,*,#9802,.F.);
#13746=ORIENTED_EDGE('',*,*,#9758,.F.);
#13747=ORIENTED_EDGE('',*,*,#9754,.F.);
#13748=ORIENTED_EDGE('',*,*,#9751,.F.);
#13749=ORIENTED_EDGE('',*,*,#9748,.F.);
#13750=ORIENTED_EDGE('',*,*,#9745,.F.);
#13751=ORIENTED_EDGE('',*,*,#9742,.F.);
#13752=ORIENTED_EDGE('',*,*,#9739,.F.);
#13753=ORIENTED_EDGE('',*,*,#9736,.F.);
#13754=ORIENTED_EDGE('',*,*,#9733,.F.);
#13755=ORIENTED_EDGE('',*,*,#9730,.F.);
#13756=ORIENTED_EDGE('',*,*,#9803,.F.);
#13757=ORIENTED_EDGE('',*,*,#9804,.T.);
#13758=ORIENTED_EDGE('',*,*,#9786,.T.);
#13759=ORIENTED_EDGE('',*,*,#9783,.T.);
#13760=ORIENTED_EDGE('',*,*,#9780,.T.);
#13761=ORIENTED_EDGE('',*,*,#9777,.T.);
#13762=ORIENTED_EDGE('',*,*,#9774,.T.);
#13763=ORIENTED_EDGE('',*,*,#9771,.T.);
#13764=ORIENTED_EDGE('',*,*,#9768,.T.);
#13765=ORIENTED_EDGE('',*,*,#9765,.T.);
#13766=ORIENTED_EDGE('',*,*,#9762,.T.);
#13767=ORIENTED_EDGE('',*,*,#9784,.T.);
#13768=ORIENTED_EDGE('',*,*,#9804,.F.);
#13769=ORIENTED_EDGE('',*,*,#9805,.F.);
#13770=ORIENTED_EDGE('',*,*,#9806,.T.);
#13771=ORIENTED_EDGE('',*,*,#9799,.F.);
#13772=ORIENTED_EDGE('',*,*,#9760,.F.);
#13773=ORIENTED_EDGE('',*,*,#9764,.F.);
#13774=ORIENTED_EDGE('',*,*,#9767,.F.);
#13775=ORIENTED_EDGE('',*,*,#9770,.F.);
#13776=ORIENTED_EDGE('',*,*,#9773,.F.);
#13777=ORIENTED_EDGE('',*,*,#9776,.F.);
#13778=ORIENTED_EDGE('',*,*,#9779,.F.);
#13779=ORIENTED_EDGE('',*,*,#9782,.F.);
#13780=ORIENTED_EDGE('',*,*,#9785,.F.);
#13781=ORIENTED_EDGE('',*,*,#9806,.F.);
#13782=ORIENTED_EDGE('',*,*,#9807,.F.);
#13783=ORIENTED_EDGE('',*,*,#9728,.F.);
#13784=ORIENTED_EDGE('',*,*,#9732,.F.);
#13785=ORIENTED_EDGE('',*,*,#9735,.F.);
#13786=ORIENTED_EDGE('',*,*,#9738,.F.);
#13787=ORIENTED_EDGE('',*,*,#9741,.F.);
#13788=ORIENTED_EDGE('',*,*,#9744,.F.);
#13789=ORIENTED_EDGE('',*,*,#9747,.F.);
#13790=ORIENTED_EDGE('',*,*,#9750,.F.);
#13791=ORIENTED_EDGE('',*,*,#9753,.F.);
#13792=ORIENTED_EDGE('',*,*,#9757,.F.);
#13793=ORIENTED_EDGE('',*,*,#9755,.T.);
#13794=ORIENTED_EDGE('',*,*,#9802,.T.);
#13795=ORIENTED_EDGE('',*,*,#9808,.F.);
#13796=ORIENTED_EDGE('',*,*,#9809,.F.);
#13797=ORIENTED_EDGE('',*,*,#9810,.T.);
#13798=ORIENTED_EDGE('',*,*,#9795,.T.);
#13799=ORIENTED_EDGE('',*,*,#9810,.F.);
#13800=ORIENTED_EDGE('',*,*,#9809,.T.);
#13801=ORIENTED_EDGE('',*,*,#9807,.T.);
#13802=ORIENTED_EDGE('',*,*,#9805,.T.);
#13803=ORIENTED_EDGE('',*,*,#9803,.T.);
#13804=ORIENTED_EDGE('',*,*,#9729,.F.);
#13805=ORIENTED_EDGE('',*,*,#9811,.F.);
#13806=ORIENTED_EDGE('',*,*,#9812,.T.);
#13807=ORIENTED_EDGE('',*,*,#9808,.T.);
#13808=ORIENTED_EDGE('',*,*,#9800,.T.);
#13809=ORIENTED_EDGE('',*,*,#9756,.T.);
#13810=ORIENTED_EDGE('',*,*,#9812,.F.);
#13811=ORIENTED_EDGE('',*,*,#9811,.T.);
#13812=ORIENTED_EDGE('',*,*,#9813,.F.);
#13813=ORIENTED_EDGE('',*,*,#9814,.T.);
#13814=ORIENTED_EDGE('',*,*,#9815,.T.);
#13815=ORIENTED_EDGE('',*,*,#9816,.T.);
#13816=ORIENTED_EDGE('',*,*,#9817,.F.);
#13817=ORIENTED_EDGE('',*,*,#9818,.T.);
#13818=ORIENTED_EDGE('',*,*,#9813,.T.);
#13819=ORIENTED_EDGE('',*,*,#9819,.T.);
#13820=ORIENTED_EDGE('',*,*,#9820,.F.);
#13821=ORIENTED_EDGE('',*,*,#9821,.T.);
#13822=ORIENTED_EDGE('',*,*,#9817,.T.);
#13823=ORIENTED_EDGE('',*,*,#9822,.T.);
#13824=ORIENTED_EDGE('',*,*,#9823,.F.);
#13825=ORIENTED_EDGE('',*,*,#9824,.T.);
#13826=ORIENTED_EDGE('',*,*,#9820,.T.);
#13827=ORIENTED_EDGE('',*,*,#9825,.T.);
#13828=ORIENTED_EDGE('',*,*,#9826,.F.);
#13829=ORIENTED_EDGE('',*,*,#9827,.T.);
#13830=ORIENTED_EDGE('',*,*,#9823,.T.);
#13831=ORIENTED_EDGE('',*,*,#9828,.T.);
#13832=ORIENTED_EDGE('',*,*,#9829,.F.);
#13833=ORIENTED_EDGE('',*,*,#9830,.T.);
#13834=ORIENTED_EDGE('',*,*,#9826,.T.);
#13835=ORIENTED_EDGE('',*,*,#9831,.T.);
#13836=ORIENTED_EDGE('',*,*,#9832,.F.);
#13837=ORIENTED_EDGE('',*,*,#9833,.T.);
#13838=ORIENTED_EDGE('',*,*,#9829,.T.);
#13839=ORIENTED_EDGE('',*,*,#9834,.T.);
#13840=ORIENTED_EDGE('',*,*,#9835,.F.);
#13841=ORIENTED_EDGE('',*,*,#9836,.T.);
#13842=ORIENTED_EDGE('',*,*,#9832,.T.);
#13843=ORIENTED_EDGE('',*,*,#9837,.T.);
#13844=ORIENTED_EDGE('',*,*,#9838,.F.);
#13845=ORIENTED_EDGE('',*,*,#9839,.T.);
#13846=ORIENTED_EDGE('',*,*,#9835,.T.);
#13847=ORIENTED_EDGE('',*,*,#9840,.T.);
#13848=ORIENTED_EDGE('',*,*,#9841,.F.);
#13849=ORIENTED_EDGE('',*,*,#9842,.T.);
#13850=ORIENTED_EDGE('',*,*,#9838,.T.);
#13851=ORIENTED_EDGE('',*,*,#9843,.T.);
#13852=ORIENTED_EDGE('',*,*,#9844,.F.);
#13853=ORIENTED_EDGE('',*,*,#9845,.T.);
#13854=ORIENTED_EDGE('',*,*,#9841,.T.);
#13855=ORIENTED_EDGE('',*,*,#9846,.T.);
#13856=ORIENTED_EDGE('',*,*,#9847,.F.);
#13857=ORIENTED_EDGE('',*,*,#9848,.T.);
#13858=ORIENTED_EDGE('',*,*,#9844,.T.);
#13859=ORIENTED_EDGE('',*,*,#9849,.T.);
#13860=ORIENTED_EDGE('',*,*,#9850,.F.);
#13861=ORIENTED_EDGE('',*,*,#9851,.T.);
#13862=ORIENTED_EDGE('',*,*,#9847,.T.);
#13863=ORIENTED_EDGE('',*,*,#9852,.T.);
#13864=ORIENTED_EDGE('',*,*,#9853,.F.);
#13865=ORIENTED_EDGE('',*,*,#9854,.T.);
#13866=ORIENTED_EDGE('',*,*,#9850,.T.);
#13867=ORIENTED_EDGE('',*,*,#9855,.T.);
#13868=ORIENTED_EDGE('',*,*,#9856,.F.);
#13869=ORIENTED_EDGE('',*,*,#9857,.T.);
#13870=ORIENTED_EDGE('',*,*,#9853,.T.);
#13871=ORIENTED_EDGE('',*,*,#9858,.T.);
#13872=ORIENTED_EDGE('',*,*,#9859,.F.);
#13873=ORIENTED_EDGE('',*,*,#9860,.T.);
#13874=ORIENTED_EDGE('',*,*,#9856,.T.);
#13875=ORIENTED_EDGE('',*,*,#9861,.T.);
#13876=ORIENTED_EDGE('',*,*,#9862,.F.);
#13877=ORIENTED_EDGE('',*,*,#9863,.T.);
#13878=ORIENTED_EDGE('',*,*,#9859,.T.);
#13879=ORIENTED_EDGE('',*,*,#9864,.T.);
#13880=ORIENTED_EDGE('',*,*,#9865,.F.);
#13881=ORIENTED_EDGE('',*,*,#9866,.T.);
#13882=ORIENTED_EDGE('',*,*,#9862,.T.);
#13883=ORIENTED_EDGE('',*,*,#9867,.T.);
#13884=ORIENTED_EDGE('',*,*,#9868,.F.);
#13885=ORIENTED_EDGE('',*,*,#9869,.T.);
#13886=ORIENTED_EDGE('',*,*,#9865,.T.);
#13887=ORIENTED_EDGE('',*,*,#9870,.T.);
#13888=ORIENTED_EDGE('',*,*,#9871,.F.);
#13889=ORIENTED_EDGE('',*,*,#9872,.T.);
#13890=ORIENTED_EDGE('',*,*,#9868,.T.);
#13891=ORIENTED_EDGE('',*,*,#9873,.T.);
#13892=ORIENTED_EDGE('',*,*,#9874,.F.);
#13893=ORIENTED_EDGE('',*,*,#9875,.T.);
#13894=ORIENTED_EDGE('',*,*,#9871,.T.);
#13895=ORIENTED_EDGE('',*,*,#9876,.T.);
#13896=ORIENTED_EDGE('',*,*,#9877,.F.);
#13897=ORIENTED_EDGE('',*,*,#9878,.T.);
#13898=ORIENTED_EDGE('',*,*,#9874,.T.);
#13899=ORIENTED_EDGE('',*,*,#9879,.T.);
#13900=ORIENTED_EDGE('',*,*,#9880,.F.);
#13901=ORIENTED_EDGE('',*,*,#9881,.T.);
#13902=ORIENTED_EDGE('',*,*,#9877,.T.);
#13903=ORIENTED_EDGE('',*,*,#9882,.T.);
#13904=ORIENTED_EDGE('',*,*,#9883,.F.);
#13905=ORIENTED_EDGE('',*,*,#9884,.T.);
#13906=ORIENTED_EDGE('',*,*,#9880,.T.);
#13907=ORIENTED_EDGE('',*,*,#9885,.T.);
#13908=ORIENTED_EDGE('',*,*,#9886,.F.);
#13909=ORIENTED_EDGE('',*,*,#9887,.T.);
#13910=ORIENTED_EDGE('',*,*,#9883,.T.);
#13911=ORIENTED_EDGE('',*,*,#9888,.T.);
#13912=ORIENTED_EDGE('',*,*,#9889,.F.);
#13913=ORIENTED_EDGE('',*,*,#9890,.T.);
#13914=ORIENTED_EDGE('',*,*,#9886,.T.);
#13915=ORIENTED_EDGE('',*,*,#9891,.T.);
#13916=ORIENTED_EDGE('',*,*,#9892,.F.);
#13917=ORIENTED_EDGE('',*,*,#9893,.T.);
#13918=ORIENTED_EDGE('',*,*,#9889,.T.);
#13919=ORIENTED_EDGE('',*,*,#9894,.T.);
#13920=ORIENTED_EDGE('',*,*,#9895,.F.);
#13921=ORIENTED_EDGE('',*,*,#9896,.T.);
#13922=ORIENTED_EDGE('',*,*,#9892,.T.);
#13923=ORIENTED_EDGE('',*,*,#9897,.T.);
#13924=ORIENTED_EDGE('',*,*,#9898,.F.);
#13925=ORIENTED_EDGE('',*,*,#9899,.T.);
#13926=ORIENTED_EDGE('',*,*,#9895,.T.);
#13927=ORIENTED_EDGE('',*,*,#9900,.T.);
#13928=ORIENTED_EDGE('',*,*,#9901,.F.);
#13929=ORIENTED_EDGE('',*,*,#9902,.T.);
#13930=ORIENTED_EDGE('',*,*,#9898,.T.);
#13931=ORIENTED_EDGE('',*,*,#9903,.T.);
#13932=ORIENTED_EDGE('',*,*,#9904,.F.);
#13933=ORIENTED_EDGE('',*,*,#9905,.T.);
#13934=ORIENTED_EDGE('',*,*,#9901,.T.);
#13935=ORIENTED_EDGE('',*,*,#9906,.T.);
#13936=ORIENTED_EDGE('',*,*,#9907,.F.);
#13937=ORIENTED_EDGE('',*,*,#9908,.T.);
#13938=ORIENTED_EDGE('',*,*,#9904,.T.);
#13939=ORIENTED_EDGE('',*,*,#9909,.T.);
#13940=ORIENTED_EDGE('',*,*,#9910,.F.);
#13941=ORIENTED_EDGE('',*,*,#9911,.T.);
#13942=ORIENTED_EDGE('',*,*,#9907,.T.);
#13943=ORIENTED_EDGE('',*,*,#9912,.T.);
#13944=ORIENTED_EDGE('',*,*,#9913,.F.);
#13945=ORIENTED_EDGE('',*,*,#9914,.T.);
#13946=ORIENTED_EDGE('',*,*,#9910,.T.);
#13947=ORIENTED_EDGE('',*,*,#9915,.T.);
#13948=ORIENTED_EDGE('',*,*,#9916,.F.);
#13949=ORIENTED_EDGE('',*,*,#9917,.T.);
#13950=ORIENTED_EDGE('',*,*,#9913,.T.);
#13951=ORIENTED_EDGE('',*,*,#9918,.T.);
#13952=ORIENTED_EDGE('',*,*,#9919,.F.);
#13953=ORIENTED_EDGE('',*,*,#9920,.T.);
#13954=ORIENTED_EDGE('',*,*,#9916,.T.);
#13955=ORIENTED_EDGE('',*,*,#9921,.T.);
#13956=ORIENTED_EDGE('',*,*,#9922,.F.);
#13957=ORIENTED_EDGE('',*,*,#9923,.T.);
#13958=ORIENTED_EDGE('',*,*,#9919,.T.);
#13959=ORIENTED_EDGE('',*,*,#9924,.T.);
#13960=ORIENTED_EDGE('',*,*,#9925,.F.);
#13961=ORIENTED_EDGE('',*,*,#9926,.T.);
#13962=ORIENTED_EDGE('',*,*,#9922,.T.);
#13963=ORIENTED_EDGE('',*,*,#9927,.T.);
#13964=ORIENTED_EDGE('',*,*,#9928,.F.);
#13965=ORIENTED_EDGE('',*,*,#9929,.T.);
#13966=ORIENTED_EDGE('',*,*,#9925,.T.);
#13967=ORIENTED_EDGE('',*,*,#9930,.T.);
#13968=ORIENTED_EDGE('',*,*,#9931,.F.);
#13969=ORIENTED_EDGE('',*,*,#9932,.T.);
#13970=ORIENTED_EDGE('',*,*,#9928,.T.);
#13971=ORIENTED_EDGE('',*,*,#9933,.T.);
#13972=ORIENTED_EDGE('',*,*,#9934,.F.);
#13973=ORIENTED_EDGE('',*,*,#9935,.T.);
#13974=ORIENTED_EDGE('',*,*,#9931,.T.);
#13975=ORIENTED_EDGE('',*,*,#9936,.T.);
#13976=ORIENTED_EDGE('',*,*,#9937,.F.);
#13977=ORIENTED_EDGE('',*,*,#9938,.T.);
#13978=ORIENTED_EDGE('',*,*,#9934,.T.);
#13979=ORIENTED_EDGE('',*,*,#9939,.T.);
#13980=ORIENTED_EDGE('',*,*,#9940,.F.);
#13981=ORIENTED_EDGE('',*,*,#9941,.T.);
#13982=ORIENTED_EDGE('',*,*,#9937,.T.);
#13983=ORIENTED_EDGE('',*,*,#9942,.T.);
#13984=ORIENTED_EDGE('',*,*,#9943,.F.);
#13985=ORIENTED_EDGE('',*,*,#9944,.T.);
#13986=ORIENTED_EDGE('',*,*,#9940,.T.);
#13987=ORIENTED_EDGE('',*,*,#9945,.T.);
#13988=ORIENTED_EDGE('',*,*,#9946,.F.);
#13989=ORIENTED_EDGE('',*,*,#9947,.T.);
#13990=ORIENTED_EDGE('',*,*,#9948,.F.);
#13991=ORIENTED_EDGE('',*,*,#9949,.F.);
#13992=ORIENTED_EDGE('',*,*,#9950,.T.);
#13993=ORIENTED_EDGE('',*,*,#9946,.T.);
#13994=ORIENTED_EDGE('',*,*,#9951,.F.);
#13995=ORIENTED_EDGE('',*,*,#9952,.F.);
#13996=ORIENTED_EDGE('',*,*,#9953,.F.);
#13997=ORIENTED_EDGE('',*,*,#9954,.T.);
#13998=ORIENTED_EDGE('',*,*,#9949,.T.);
#13999=ORIENTED_EDGE('',*,*,#9955,.F.);
#14000=ORIENTED_EDGE('',*,*,#9956,.F.);
#14001=ORIENTED_EDGE('',*,*,#9957,.T.);
#14002=ORIENTED_EDGE('',*,*,#9953,.T.);
#14003=ORIENTED_EDGE('',*,*,#9958,.F.);
#14004=ORIENTED_EDGE('',*,*,#9959,.F.);
#14005=ORIENTED_EDGE('',*,*,#9960,.T.);
#14006=ORIENTED_EDGE('',*,*,#9956,.T.);
#14007=ORIENTED_EDGE('',*,*,#9961,.F.);
#14008=ORIENTED_EDGE('',*,*,#9962,.F.);
#14009=ORIENTED_EDGE('',*,*,#9963,.T.);
#14010=ORIENTED_EDGE('',*,*,#9959,.T.);
#14011=ORIENTED_EDGE('',*,*,#9964,.F.);
#14012=ORIENTED_EDGE('',*,*,#9965,.F.);
#14013=ORIENTED_EDGE('',*,*,#9966,.T.);
#14014=ORIENTED_EDGE('',*,*,#9962,.T.);
#14015=ORIENTED_EDGE('',*,*,#9967,.F.);
#14016=ORIENTED_EDGE('',*,*,#9968,.F.);
#14017=ORIENTED_EDGE('',*,*,#9969,.T.);
#14018=ORIENTED_EDGE('',*,*,#9965,.T.);
#14019=ORIENTED_EDGE('',*,*,#9970,.F.);
#14020=ORIENTED_EDGE('',*,*,#9971,.F.);
#14021=ORIENTED_EDGE('',*,*,#9972,.T.);
#14022=ORIENTED_EDGE('',*,*,#9968,.T.);
#14023=ORIENTED_EDGE('',*,*,#9973,.F.);
#14024=ORIENTED_EDGE('',*,*,#9974,.F.);
#14025=ORIENTED_EDGE('',*,*,#9975,.T.);
#14026=ORIENTED_EDGE('',*,*,#9971,.T.);
#14027=ORIENTED_EDGE('',*,*,#9976,.F.);
#14028=ORIENTED_EDGE('',*,*,#9977,.F.);
#14029=ORIENTED_EDGE('',*,*,#9978,.T.);
#14030=ORIENTED_EDGE('',*,*,#9974,.T.);
#14031=ORIENTED_EDGE('',*,*,#9979,.F.);
#14032=ORIENTED_EDGE('',*,*,#9980,.F.);
#14033=ORIENTED_EDGE('',*,*,#9981,.T.);
#14034=ORIENTED_EDGE('',*,*,#9977,.T.);
#14035=ORIENTED_EDGE('',*,*,#9982,.F.);
#14036=ORIENTED_EDGE('',*,*,#9983,.F.);
#14037=ORIENTED_EDGE('',*,*,#9984,.T.);
#14038=ORIENTED_EDGE('',*,*,#9980,.T.);
#14039=ORIENTED_EDGE('',*,*,#9985,.F.);
#14040=ORIENTED_EDGE('',*,*,#9986,.F.);
#14041=ORIENTED_EDGE('',*,*,#9987,.T.);
#14042=ORIENTED_EDGE('',*,*,#9983,.T.);
#14043=ORIENTED_EDGE('',*,*,#9988,.F.);
#14044=ORIENTED_EDGE('',*,*,#9989,.F.);
#14045=ORIENTED_EDGE('',*,*,#9990,.T.);
#14046=ORIENTED_EDGE('',*,*,#9986,.T.);
#14047=ORIENTED_EDGE('',*,*,#9991,.F.);
#14048=ORIENTED_EDGE('',*,*,#9992,.F.);
#14049=ORIENTED_EDGE('',*,*,#9993,.T.);
#14050=ORIENTED_EDGE('',*,*,#9989,.T.);
#14051=ORIENTED_EDGE('',*,*,#9994,.F.);
#14052=ORIENTED_EDGE('',*,*,#9995,.F.);
#14053=ORIENTED_EDGE('',*,*,#9996,.T.);
#14054=ORIENTED_EDGE('',*,*,#9992,.T.);
#14055=ORIENTED_EDGE('',*,*,#9997,.F.);
#14056=ORIENTED_EDGE('',*,*,#9998,.F.);
#14057=ORIENTED_EDGE('',*,*,#9999,.T.);
#14058=ORIENTED_EDGE('',*,*,#9995,.T.);
#14059=ORIENTED_EDGE('',*,*,#10000,.F.);
#14060=ORIENTED_EDGE('',*,*,#10001,.F.);
#14061=ORIENTED_EDGE('',*,*,#10002,.T.);
#14062=ORIENTED_EDGE('',*,*,#9998,.T.);
#14063=ORIENTED_EDGE('',*,*,#10003,.F.);
#14064=ORIENTED_EDGE('',*,*,#10004,.F.);
#14065=ORIENTED_EDGE('',*,*,#10005,.T.);
#14066=ORIENTED_EDGE('',*,*,#10001,.T.);
#14067=ORIENTED_EDGE('',*,*,#10006,.F.);
#14068=ORIENTED_EDGE('',*,*,#10007,.F.);
#14069=ORIENTED_EDGE('',*,*,#10008,.T.);
#14070=ORIENTED_EDGE('',*,*,#10004,.T.);
#14071=ORIENTED_EDGE('',*,*,#10009,.F.);
#14072=ORIENTED_EDGE('',*,*,#10010,.F.);
#14073=ORIENTED_EDGE('',*,*,#10011,.T.);
#14074=ORIENTED_EDGE('',*,*,#10007,.T.);
#14075=ORIENTED_EDGE('',*,*,#10012,.F.);
#14076=ORIENTED_EDGE('',*,*,#10013,.F.);
#14077=ORIENTED_EDGE('',*,*,#10014,.T.);
#14078=ORIENTED_EDGE('',*,*,#10010,.T.);
#14079=ORIENTED_EDGE('',*,*,#10015,.F.);
#14080=ORIENTED_EDGE('',*,*,#10016,.F.);
#14081=ORIENTED_EDGE('',*,*,#10017,.T.);
#14082=ORIENTED_EDGE('',*,*,#10013,.T.);
#14083=ORIENTED_EDGE('',*,*,#10018,.F.);
#14084=ORIENTED_EDGE('',*,*,#10019,.F.);
#14085=ORIENTED_EDGE('',*,*,#10020,.T.);
#14086=ORIENTED_EDGE('',*,*,#10016,.T.);
#14087=ORIENTED_EDGE('',*,*,#10021,.F.);
#14088=ORIENTED_EDGE('',*,*,#10022,.F.);
#14089=ORIENTED_EDGE('',*,*,#10023,.T.);
#14090=ORIENTED_EDGE('',*,*,#10019,.T.);
#14091=ORIENTED_EDGE('',*,*,#10024,.F.);
#14092=ORIENTED_EDGE('',*,*,#10025,.F.);
#14093=ORIENTED_EDGE('',*,*,#10026,.T.);
#14094=ORIENTED_EDGE('',*,*,#10022,.T.);
#14095=ORIENTED_EDGE('',*,*,#10027,.F.);
#14096=ORIENTED_EDGE('',*,*,#10028,.F.);
#14097=ORIENTED_EDGE('',*,*,#10029,.T.);
#14098=ORIENTED_EDGE('',*,*,#10025,.T.);
#14099=ORIENTED_EDGE('',*,*,#10030,.F.);
#14100=ORIENTED_EDGE('',*,*,#10031,.F.);
#14101=ORIENTED_EDGE('',*,*,#10032,.T.);
#14102=ORIENTED_EDGE('',*,*,#10028,.T.);
#14103=ORIENTED_EDGE('',*,*,#10033,.F.);
#14104=ORIENTED_EDGE('',*,*,#10034,.F.);
#14105=ORIENTED_EDGE('',*,*,#10035,.T.);
#14106=ORIENTED_EDGE('',*,*,#10031,.T.);
#14107=ORIENTED_EDGE('',*,*,#10036,.F.);
#14108=ORIENTED_EDGE('',*,*,#10037,.F.);
#14109=ORIENTED_EDGE('',*,*,#10038,.T.);
#14110=ORIENTED_EDGE('',*,*,#10034,.T.);
#14111=ORIENTED_EDGE('',*,*,#10039,.F.);
#14112=ORIENTED_EDGE('',*,*,#10040,.F.);
#14113=ORIENTED_EDGE('',*,*,#10041,.T.);
#14114=ORIENTED_EDGE('',*,*,#10037,.T.);
#14115=ORIENTED_EDGE('',*,*,#10042,.F.);
#14116=ORIENTED_EDGE('',*,*,#10043,.F.);
#14117=ORIENTED_EDGE('',*,*,#10044,.T.);
#14118=ORIENTED_EDGE('',*,*,#10040,.T.);
#14119=ORIENTED_EDGE('',*,*,#10045,.F.);
#14120=ORIENTED_EDGE('',*,*,#10046,.F.);
#14121=ORIENTED_EDGE('',*,*,#10047,.T.);
#14122=ORIENTED_EDGE('',*,*,#10043,.T.);
#14123=ORIENTED_EDGE('',*,*,#10048,.F.);
#14124=ORIENTED_EDGE('',*,*,#10049,.F.);
#14125=ORIENTED_EDGE('',*,*,#10050,.T.);
#14126=ORIENTED_EDGE('',*,*,#10046,.T.);
#14127=ORIENTED_EDGE('',*,*,#10051,.F.);
#14128=ORIENTED_EDGE('',*,*,#10052,.F.);
#14129=ORIENTED_EDGE('',*,*,#10053,.T.);
#14130=ORIENTED_EDGE('',*,*,#10049,.T.);
#14131=ORIENTED_EDGE('',*,*,#10054,.F.);
#14132=ORIENTED_EDGE('',*,*,#10055,.F.);
#14133=ORIENTED_EDGE('',*,*,#10056,.T.);
#14134=ORIENTED_EDGE('',*,*,#10052,.T.);
#14135=ORIENTED_EDGE('',*,*,#10057,.F.);
#14136=ORIENTED_EDGE('',*,*,#10058,.F.);
#14137=ORIENTED_EDGE('',*,*,#10059,.T.);
#14138=ORIENTED_EDGE('',*,*,#10055,.T.);
#14139=ORIENTED_EDGE('',*,*,#10060,.F.);
#14140=ORIENTED_EDGE('',*,*,#10061,.F.);
#14141=ORIENTED_EDGE('',*,*,#10062,.T.);
#14142=ORIENTED_EDGE('',*,*,#10058,.T.);
#14143=ORIENTED_EDGE('',*,*,#10063,.F.);
#14144=ORIENTED_EDGE('',*,*,#10064,.F.);
#14145=ORIENTED_EDGE('',*,*,#10065,.T.);
#14146=ORIENTED_EDGE('',*,*,#10061,.T.);
#14147=ORIENTED_EDGE('',*,*,#10066,.F.);
#14148=ORIENTED_EDGE('',*,*,#10067,.F.);
#14149=ORIENTED_EDGE('',*,*,#10068,.T.);
#14150=ORIENTED_EDGE('',*,*,#10064,.T.);
#14151=ORIENTED_EDGE('',*,*,#10069,.F.);
#14152=ORIENTED_EDGE('',*,*,#10070,.F.);
#14153=ORIENTED_EDGE('',*,*,#10071,.T.);
#14154=ORIENTED_EDGE('',*,*,#10067,.T.);
#14155=ORIENTED_EDGE('',*,*,#10072,.F.);
#14156=ORIENTED_EDGE('',*,*,#10073,.F.);
#14157=ORIENTED_EDGE('',*,*,#10074,.T.);
#14158=ORIENTED_EDGE('',*,*,#10070,.T.);
#14159=ORIENTED_EDGE('',*,*,#10075,.F.);
#14160=ORIENTED_EDGE('',*,*,#10076,.F.);
#14161=ORIENTED_EDGE('',*,*,#10077,.T.);
#14162=ORIENTED_EDGE('',*,*,#10073,.T.);
#14163=ORIENTED_EDGE('',*,*,#10078,.F.);
#14164=ORIENTED_EDGE('',*,*,#10079,.F.);
#14165=ORIENTED_EDGE('',*,*,#10080,.F.);
#14166=ORIENTED_EDGE('',*,*,#9945,.F.);
#14167=ORIENTED_EDGE('',*,*,#9942,.F.);
#14168=ORIENTED_EDGE('',*,*,#9939,.F.);
#14169=ORIENTED_EDGE('',*,*,#9936,.F.);
#14170=ORIENTED_EDGE('',*,*,#9933,.F.);
#14171=ORIENTED_EDGE('',*,*,#9930,.F.);
#14172=ORIENTED_EDGE('',*,*,#9927,.F.);
#14173=ORIENTED_EDGE('',*,*,#9924,.F.);
#14174=ORIENTED_EDGE('',*,*,#9921,.F.);
#14175=ORIENTED_EDGE('',*,*,#9918,.F.);
#14176=ORIENTED_EDGE('',*,*,#9915,.F.);
#14177=ORIENTED_EDGE('',*,*,#9912,.F.);
#14178=ORIENTED_EDGE('',*,*,#9909,.F.);
#14179=ORIENTED_EDGE('',*,*,#9906,.F.);
#14180=ORIENTED_EDGE('',*,*,#9903,.F.);
#14181=ORIENTED_EDGE('',*,*,#9900,.F.);
#14182=ORIENTED_EDGE('',*,*,#9897,.F.);
#14183=ORIENTED_EDGE('',*,*,#9894,.F.);
#14184=ORIENTED_EDGE('',*,*,#9891,.F.);
#14185=ORIENTED_EDGE('',*,*,#9888,.F.);
#14186=ORIENTED_EDGE('',*,*,#9885,.F.);
#14187=ORIENTED_EDGE('',*,*,#9882,.F.);
#14188=ORIENTED_EDGE('',*,*,#9879,.F.);
#14189=ORIENTED_EDGE('',*,*,#9876,.F.);
#14190=ORIENTED_EDGE('',*,*,#9873,.F.);
#14191=ORIENTED_EDGE('',*,*,#9870,.F.);
#14192=ORIENTED_EDGE('',*,*,#9867,.F.);
#14193=ORIENTED_EDGE('',*,*,#9864,.F.);
#14194=ORIENTED_EDGE('',*,*,#9861,.F.);
#14195=ORIENTED_EDGE('',*,*,#9858,.F.);
#14196=ORIENTED_EDGE('',*,*,#9855,.F.);
#14197=ORIENTED_EDGE('',*,*,#9852,.F.);
#14198=ORIENTED_EDGE('',*,*,#9849,.F.);
#14199=ORIENTED_EDGE('',*,*,#9846,.F.);
#14200=ORIENTED_EDGE('',*,*,#9843,.F.);
#14201=ORIENTED_EDGE('',*,*,#9840,.F.);
#14202=ORIENTED_EDGE('',*,*,#9837,.F.);
#14203=ORIENTED_EDGE('',*,*,#9834,.F.);
#14204=ORIENTED_EDGE('',*,*,#9831,.F.);
#14205=ORIENTED_EDGE('',*,*,#9828,.F.);
#14206=ORIENTED_EDGE('',*,*,#9825,.F.);
#14207=ORIENTED_EDGE('',*,*,#9822,.F.);
#14208=ORIENTED_EDGE('',*,*,#9819,.F.);
#14209=ORIENTED_EDGE('',*,*,#9816,.F.);
#14210=ORIENTED_EDGE('',*,*,#10081,.F.);
#14211=ORIENTED_EDGE('',*,*,#10082,.T.);
#14212=ORIENTED_EDGE('',*,*,#10078,.T.);
#14213=ORIENTED_EDGE('',*,*,#10075,.T.);
#14214=ORIENTED_EDGE('',*,*,#10072,.T.);
#14215=ORIENTED_EDGE('',*,*,#10069,.T.);
#14216=ORIENTED_EDGE('',*,*,#10066,.T.);
#14217=ORIENTED_EDGE('',*,*,#10063,.T.);
#14218=ORIENTED_EDGE('',*,*,#10060,.T.);
#14219=ORIENTED_EDGE('',*,*,#10057,.T.);
#14220=ORIENTED_EDGE('',*,*,#10054,.T.);
#14221=ORIENTED_EDGE('',*,*,#10051,.T.);
#14222=ORIENTED_EDGE('',*,*,#10048,.T.);
#14223=ORIENTED_EDGE('',*,*,#10045,.T.);
#14224=ORIENTED_EDGE('',*,*,#10042,.T.);
#14225=ORIENTED_EDGE('',*,*,#10039,.T.);
#14226=ORIENTED_EDGE('',*,*,#10036,.T.);
#14227=ORIENTED_EDGE('',*,*,#10033,.T.);
#14228=ORIENTED_EDGE('',*,*,#10030,.T.);
#14229=ORIENTED_EDGE('',*,*,#10027,.T.);
#14230=ORIENTED_EDGE('',*,*,#10024,.T.);
#14231=ORIENTED_EDGE('',*,*,#10021,.T.);
#14232=ORIENTED_EDGE('',*,*,#10018,.T.);
#14233=ORIENTED_EDGE('',*,*,#10015,.T.);
#14234=ORIENTED_EDGE('',*,*,#10012,.T.);
#14235=ORIENTED_EDGE('',*,*,#10009,.T.);
#14236=ORIENTED_EDGE('',*,*,#10006,.T.);
#14237=ORIENTED_EDGE('',*,*,#10003,.T.);
#14238=ORIENTED_EDGE('',*,*,#10000,.T.);
#14239=ORIENTED_EDGE('',*,*,#9997,.T.);
#14240=ORIENTED_EDGE('',*,*,#9994,.T.);
#14241=ORIENTED_EDGE('',*,*,#9991,.T.);
#14242=ORIENTED_EDGE('',*,*,#9988,.T.);
#14243=ORIENTED_EDGE('',*,*,#9985,.T.);
#14244=ORIENTED_EDGE('',*,*,#9982,.T.);
#14245=ORIENTED_EDGE('',*,*,#9979,.T.);
#14246=ORIENTED_EDGE('',*,*,#9976,.T.);
#14247=ORIENTED_EDGE('',*,*,#9973,.T.);
#14248=ORIENTED_EDGE('',*,*,#9970,.T.);
#14249=ORIENTED_EDGE('',*,*,#9967,.T.);
#14250=ORIENTED_EDGE('',*,*,#9964,.T.);
#14251=ORIENTED_EDGE('',*,*,#9961,.T.);
#14252=ORIENTED_EDGE('',*,*,#9958,.T.);
#14253=ORIENTED_EDGE('',*,*,#9955,.T.);
#14254=ORIENTED_EDGE('',*,*,#9952,.T.);
#14255=ORIENTED_EDGE('',*,*,#10083,.T.);
#14256=ORIENTED_EDGE('',*,*,#10084,.T.);
#14257=ORIENTED_EDGE('',*,*,#10085,.T.);
#14258=ORIENTED_EDGE('',*,*,#10086,.T.);
#14259=ORIENTED_EDGE('',*,*,#10081,.T.);
#14260=ORIENTED_EDGE('',*,*,#10076,.T.);
#14261=ORIENTED_EDGE('',*,*,#10082,.F.);
#14262=ORIENTED_EDGE('',*,*,#10086,.F.);
#14263=ORIENTED_EDGE('',*,*,#10087,.T.);
#14264=ORIENTED_EDGE('',*,*,#10088,.F.);
#14265=ORIENTED_EDGE('',*,*,#9947,.F.);
#14266=ORIENTED_EDGE('',*,*,#9950,.F.);
#14267=ORIENTED_EDGE('',*,*,#9954,.F.);
#14268=ORIENTED_EDGE('',*,*,#9957,.F.);
#14269=ORIENTED_EDGE('',*,*,#9960,.F.);
#14270=ORIENTED_EDGE('',*,*,#9963,.F.);
#14271=ORIENTED_EDGE('',*,*,#9966,.F.);
#14272=ORIENTED_EDGE('',*,*,#9969,.F.);
#14273=ORIENTED_EDGE('',*,*,#9972,.F.);
#14274=ORIENTED_EDGE('',*,*,#9975,.F.);
#14275=ORIENTED_EDGE('',*,*,#9978,.F.);
#14276=ORIENTED_EDGE('',*,*,#9981,.F.);
#14277=ORIENTED_EDGE('',*,*,#9984,.F.);
#14278=ORIENTED_EDGE('',*,*,#9987,.F.);
#14279=ORIENTED_EDGE('',*,*,#9990,.F.);
#14280=ORIENTED_EDGE('',*,*,#9993,.F.);
#14281=ORIENTED_EDGE('',*,*,#9996,.F.);
#14282=ORIENTED_EDGE('',*,*,#9999,.F.);
#14283=ORIENTED_EDGE('',*,*,#10002,.F.);
#14284=ORIENTED_EDGE('',*,*,#10005,.F.);
#14285=ORIENTED_EDGE('',*,*,#10008,.F.);
#14286=ORIENTED_EDGE('',*,*,#10011,.F.);
#14287=ORIENTED_EDGE('',*,*,#10014,.F.);
#14288=ORIENTED_EDGE('',*,*,#10017,.F.);
#14289=ORIENTED_EDGE('',*,*,#10020,.F.);
#14290=ORIENTED_EDGE('',*,*,#10023,.F.);
#14291=ORIENTED_EDGE('',*,*,#10026,.F.);
#14292=ORIENTED_EDGE('',*,*,#10029,.F.);
#14293=ORIENTED_EDGE('',*,*,#10032,.F.);
#14294=ORIENTED_EDGE('',*,*,#10035,.F.);
#14295=ORIENTED_EDGE('',*,*,#10038,.F.);
#14296=ORIENTED_EDGE('',*,*,#10041,.F.);
#14297=ORIENTED_EDGE('',*,*,#10044,.F.);
#14298=ORIENTED_EDGE('',*,*,#10047,.F.);
#14299=ORIENTED_EDGE('',*,*,#10050,.F.);
#14300=ORIENTED_EDGE('',*,*,#10053,.F.);
#14301=ORIENTED_EDGE('',*,*,#10056,.F.);
#14302=ORIENTED_EDGE('',*,*,#10059,.F.);
#14303=ORIENTED_EDGE('',*,*,#10062,.F.);
#14304=ORIENTED_EDGE('',*,*,#10065,.F.);
#14305=ORIENTED_EDGE('',*,*,#10068,.F.);
#14306=ORIENTED_EDGE('',*,*,#10071,.F.);
#14307=ORIENTED_EDGE('',*,*,#10074,.F.);
#14308=ORIENTED_EDGE('',*,*,#10077,.F.);
#14309=ORIENTED_EDGE('',*,*,#10087,.F.);
#14310=ORIENTED_EDGE('',*,*,#10085,.F.);
#14311=ORIENTED_EDGE('',*,*,#9814,.F.);
#14312=ORIENTED_EDGE('',*,*,#9818,.F.);
#14313=ORIENTED_EDGE('',*,*,#9821,.F.);
#14314=ORIENTED_EDGE('',*,*,#9824,.F.);
#14315=ORIENTED_EDGE('',*,*,#9827,.F.);
#14316=ORIENTED_EDGE('',*,*,#9830,.F.);
#14317=ORIENTED_EDGE('',*,*,#9833,.F.);
#14318=ORIENTED_EDGE('',*,*,#9836,.F.);
#14319=ORIENTED_EDGE('',*,*,#9839,.F.);
#14320=ORIENTED_EDGE('',*,*,#9842,.F.);
#14321=ORIENTED_EDGE('',*,*,#9845,.F.);
#14322=ORIENTED_EDGE('',*,*,#9848,.F.);
#14323=ORIENTED_EDGE('',*,*,#9851,.F.);
#14324=ORIENTED_EDGE('',*,*,#9854,.F.);
#14325=ORIENTED_EDGE('',*,*,#9857,.F.);
#14326=ORIENTED_EDGE('',*,*,#9860,.F.);
#14327=ORIENTED_EDGE('',*,*,#9863,.F.);
#14328=ORIENTED_EDGE('',*,*,#9866,.F.);
#14329=ORIENTED_EDGE('',*,*,#9869,.F.);
#14330=ORIENTED_EDGE('',*,*,#9872,.F.);
#14331=ORIENTED_EDGE('',*,*,#9875,.F.);
#14332=ORIENTED_EDGE('',*,*,#9878,.F.);
#14333=ORIENTED_EDGE('',*,*,#9881,.F.);
#14334=ORIENTED_EDGE('',*,*,#9884,.F.);
#14335=ORIENTED_EDGE('',*,*,#9887,.F.);
#14336=ORIENTED_EDGE('',*,*,#9890,.F.);
#14337=ORIENTED_EDGE('',*,*,#9893,.F.);
#14338=ORIENTED_EDGE('',*,*,#9896,.F.);
#14339=ORIENTED_EDGE('',*,*,#9899,.F.);
#14340=ORIENTED_EDGE('',*,*,#9902,.F.);
#14341=ORIENTED_EDGE('',*,*,#9905,.F.);
#14342=ORIENTED_EDGE('',*,*,#9908,.F.);
#14343=ORIENTED_EDGE('',*,*,#9911,.F.);
#14344=ORIENTED_EDGE('',*,*,#9914,.F.);
#14345=ORIENTED_EDGE('',*,*,#9917,.F.);
#14346=ORIENTED_EDGE('',*,*,#9920,.F.);
#14347=ORIENTED_EDGE('',*,*,#9923,.F.);
#14348=ORIENTED_EDGE('',*,*,#9926,.F.);
#14349=ORIENTED_EDGE('',*,*,#9929,.F.);
#14350=ORIENTED_EDGE('',*,*,#9932,.F.);
#14351=ORIENTED_EDGE('',*,*,#9935,.F.);
#14352=ORIENTED_EDGE('',*,*,#9938,.F.);
#14353=ORIENTED_EDGE('',*,*,#9941,.F.);
#14354=ORIENTED_EDGE('',*,*,#9944,.F.);
#14355=ORIENTED_EDGE('',*,*,#10089,.F.);
#14356=ORIENTED_EDGE('',*,*,#10090,.F.);
#14357=ORIENTED_EDGE('',*,*,#10091,.F.);
#14358=ORIENTED_EDGE('',*,*,#10092,.F.);
#14359=ORIENTED_EDGE('',*,*,#10093,.F.);
#14360=ORIENTED_EDGE('',*,*,#10094,.F.);
#14361=ORIENTED_EDGE('',*,*,#10095,.T.);
#14362=ORIENTED_EDGE('',*,*,#10096,.F.);
#14363=ORIENTED_EDGE('',*,*,#10095,.F.);
#14364=ORIENTED_EDGE('',*,*,#10097,.F.);
#14365=ORIENTED_EDGE('',*,*,#10098,.F.);
#14366=ORIENTED_EDGE('',*,*,#10093,.T.);
#14367=ORIENTED_EDGE('',*,*,#10099,.F.);
#14368=ORIENTED_EDGE('',*,*,#10100,.T.);
#14369=ORIENTED_EDGE('',*,*,#10101,.T.);
#14370=ORIENTED_EDGE('',*,*,#10092,.T.);
#14371=ORIENTED_EDGE('',*,*,#10102,.F.);
#14372=ORIENTED_EDGE('',*,*,#10103,.T.);
#14373=ORIENTED_EDGE('',*,*,#10099,.T.);
#14374=ORIENTED_EDGE('',*,*,#10091,.T.);
#14375=ORIENTED_EDGE('',*,*,#10104,.F.);
#14376=ORIENTED_EDGE('',*,*,#10105,.T.);
#14377=ORIENTED_EDGE('',*,*,#10102,.T.);
#14378=ORIENTED_EDGE('',*,*,#10105,.F.);
#14379=ORIENTED_EDGE('',*,*,#10106,.F.);
#14380=ORIENTED_EDGE('',*,*,#10107,.F.);
#14381=ORIENTED_EDGE('',*,*,#10108,.F.);
#14382=ORIENTED_EDGE('',*,*,#10100,.F.);
#14383=ORIENTED_EDGE('',*,*,#10103,.F.);
#14384=ORIENTED_EDGE('',*,*,#10109,.T.);
#14385=ORIENTED_EDGE('',*,*,#10079,.T.);
#14386=ORIENTED_EDGE('',*,*,#9951,.T.);
#14387=ORIENTED_EDGE('',*,*,#9948,.T.);
#14388=ORIENTED_EDGE('',*,*,#10088,.T.);
#14389=ORIENTED_EDGE('',*,*,#10090,.T.);
#14390=ORIENTED_EDGE('',*,*,#10110,.F.);
#14391=ORIENTED_EDGE('',*,*,#10106,.T.);
#14392=ORIENTED_EDGE('',*,*,#10104,.T.);
#14393=ORIENTED_EDGE('',*,*,#10098,.T.);
#14394=ORIENTED_EDGE('',*,*,#10111,.F.);
#14395=ORIENTED_EDGE('',*,*,#10107,.T.);
#14396=ORIENTED_EDGE('',*,*,#10110,.T.);
#14397=ORIENTED_EDGE('',*,*,#10097,.T.);
#14398=ORIENTED_EDGE('',*,*,#10094,.T.);
#14399=ORIENTED_EDGE('',*,*,#10101,.F.);
#14400=ORIENTED_EDGE('',*,*,#10108,.T.);
#14401=ORIENTED_EDGE('',*,*,#10111,.T.);
#14402=ORIENTED_EDGE('',*,*,#10096,.T.);
#14403=ORIENTED_EDGE('',*,*,#10112,.F.);
#14404=ORIENTED_EDGE('',*,*,#10083,.F.);
#14405=ORIENTED_EDGE('',*,*,#9815,.F.);
#14406=ORIENTED_EDGE('',*,*,#10084,.F.);
#14407=ORIENTED_EDGE('',*,*,#10113,.T.);
#14408=ORIENTED_EDGE('',*,*,#10112,.T.);
#14409=ORIENTED_EDGE('',*,*,#10113,.F.);
#14410=ORIENTED_EDGE('',*,*,#9943,.T.);
#14411=ORIENTED_EDGE('',*,*,#10080,.T.);
#14412=ORIENTED_EDGE('',*,*,#10109,.F.);
#14413=ORIENTED_EDGE('',*,*,#10089,.T.);
#14414=ORIENTED_EDGE('',*,*,#10114,.F.);
#14415=ORIENTED_EDGE('',*,*,#10115,.T.);
#14416=ORIENTED_EDGE('',*,*,#10116,.T.);
#14417=ORIENTED_EDGE('',*,*,#10117,.T.);
#14418=ORIENTED_EDGE('',*,*,#10118,.F.);
#14419=ORIENTED_EDGE('',*,*,#10119,.T.);
#14420=ORIENTED_EDGE('',*,*,#10114,.T.);
#14421=ORIENTED_EDGE('',*,*,#10120,.T.);
#14422=ORIENTED_EDGE('',*,*,#10121,.F.);
#14423=ORIENTED_EDGE('',*,*,#10122,.T.);
#14424=ORIENTED_EDGE('',*,*,#10118,.T.);
#14425=ORIENTED_EDGE('',*,*,#10123,.T.);
#14426=ORIENTED_EDGE('',*,*,#10124,.F.);
#14427=ORIENTED_EDGE('',*,*,#10125,.T.);
#14428=ORIENTED_EDGE('',*,*,#10121,.T.);
#14429=ORIENTED_EDGE('',*,*,#10126,.T.);
#14430=ORIENTED_EDGE('',*,*,#10127,.F.);
#14431=ORIENTED_EDGE('',*,*,#10128,.T.);
#14432=ORIENTED_EDGE('',*,*,#10124,.T.);
#14433=ORIENTED_EDGE('',*,*,#10129,.T.);
#14434=ORIENTED_EDGE('',*,*,#10130,.F.);
#14435=ORIENTED_EDGE('',*,*,#10131,.T.);
#14436=ORIENTED_EDGE('',*,*,#10127,.T.);
#14437=ORIENTED_EDGE('',*,*,#10132,.T.);
#14438=ORIENTED_EDGE('',*,*,#10133,.F.);
#14439=ORIENTED_EDGE('',*,*,#10134,.T.);
#14440=ORIENTED_EDGE('',*,*,#10130,.T.);
#14441=ORIENTED_EDGE('',*,*,#10135,.T.);
#14442=ORIENTED_EDGE('',*,*,#10136,.F.);
#14443=ORIENTED_EDGE('',*,*,#10137,.T.);
#14444=ORIENTED_EDGE('',*,*,#10133,.T.);
#14445=ORIENTED_EDGE('',*,*,#10138,.T.);
#14446=ORIENTED_EDGE('',*,*,#10139,.F.);
#14447=ORIENTED_EDGE('',*,*,#10140,.T.);
#14448=ORIENTED_EDGE('',*,*,#10136,.T.);
#14449=ORIENTED_EDGE('',*,*,#10141,.T.);
#14450=ORIENTED_EDGE('',*,*,#10142,.F.);
#14451=ORIENTED_EDGE('',*,*,#10143,.T.);
#14452=ORIENTED_EDGE('',*,*,#10139,.T.);
#14453=ORIENTED_EDGE('',*,*,#10144,.T.);
#14454=ORIENTED_EDGE('',*,*,#10145,.F.);
#14455=ORIENTED_EDGE('',*,*,#10146,.T.);
#14456=ORIENTED_EDGE('',*,*,#10142,.T.);
#14457=ORIENTED_EDGE('',*,*,#10147,.T.);
#14458=ORIENTED_EDGE('',*,*,#10148,.F.);
#14459=ORIENTED_EDGE('',*,*,#10149,.T.);
#14460=ORIENTED_EDGE('',*,*,#10145,.T.);
#14461=ORIENTED_EDGE('',*,*,#10150,.T.);
#14462=ORIENTED_EDGE('',*,*,#10151,.F.);
#14463=ORIENTED_EDGE('',*,*,#10152,.T.);
#14464=ORIENTED_EDGE('',*,*,#10148,.T.);
#14465=ORIENTED_EDGE('',*,*,#10153,.T.);
#14466=ORIENTED_EDGE('',*,*,#10154,.F.);
#14467=ORIENTED_EDGE('',*,*,#10155,.T.);
#14468=ORIENTED_EDGE('',*,*,#10151,.T.);
#14469=ORIENTED_EDGE('',*,*,#10156,.T.);
#14470=ORIENTED_EDGE('',*,*,#10157,.F.);
#14471=ORIENTED_EDGE('',*,*,#10158,.T.);
#14472=ORIENTED_EDGE('',*,*,#10154,.T.);
#14473=ORIENTED_EDGE('',*,*,#10159,.T.);
#14474=ORIENTED_EDGE('',*,*,#10160,.F.);
#14475=ORIENTED_EDGE('',*,*,#10161,.T.);
#14476=ORIENTED_EDGE('',*,*,#10157,.T.);
#14477=ORIENTED_EDGE('',*,*,#10162,.T.);
#14478=ORIENTED_EDGE('',*,*,#10163,.F.);
#14479=ORIENTED_EDGE('',*,*,#10164,.T.);
#14480=ORIENTED_EDGE('',*,*,#10160,.T.);
#14481=ORIENTED_EDGE('',*,*,#10165,.T.);
#14482=ORIENTED_EDGE('',*,*,#10166,.F.);
#14483=ORIENTED_EDGE('',*,*,#10167,.T.);
#14484=ORIENTED_EDGE('',*,*,#10163,.T.);
#14485=ORIENTED_EDGE('',*,*,#10168,.T.);
#14486=ORIENTED_EDGE('',*,*,#10169,.F.);
#14487=ORIENTED_EDGE('',*,*,#10170,.T.);
#14488=ORIENTED_EDGE('',*,*,#10166,.T.);
#14489=ORIENTED_EDGE('',*,*,#10171,.T.);
#14490=ORIENTED_EDGE('',*,*,#10172,.F.);
#14491=ORIENTED_EDGE('',*,*,#10173,.T.);
#14492=ORIENTED_EDGE('',*,*,#10169,.T.);
#14493=ORIENTED_EDGE('',*,*,#10174,.T.);
#14494=ORIENTED_EDGE('',*,*,#10175,.F.);
#14495=ORIENTED_EDGE('',*,*,#10176,.T.);
#14496=ORIENTED_EDGE('',*,*,#10172,.T.);
#14497=ORIENTED_EDGE('',*,*,#10177,.T.);
#14498=ORIENTED_EDGE('',*,*,#10178,.F.);
#14499=ORIENTED_EDGE('',*,*,#10179,.T.);
#14500=ORIENTED_EDGE('',*,*,#10175,.T.);
#14501=ORIENTED_EDGE('',*,*,#10180,.T.);
#14502=ORIENTED_EDGE('',*,*,#10181,.F.);
#14503=ORIENTED_EDGE('',*,*,#10182,.T.);
#14504=ORIENTED_EDGE('',*,*,#10178,.T.);
#14505=ORIENTED_EDGE('',*,*,#10183,.T.);
#14506=ORIENTED_EDGE('',*,*,#10184,.F.);
#14507=ORIENTED_EDGE('',*,*,#10185,.T.);
#14508=ORIENTED_EDGE('',*,*,#10181,.T.);
#14509=ORIENTED_EDGE('',*,*,#10186,.T.);
#14510=ORIENTED_EDGE('',*,*,#10187,.F.);
#14511=ORIENTED_EDGE('',*,*,#10188,.T.);
#14512=ORIENTED_EDGE('',*,*,#10184,.T.);
#14513=ORIENTED_EDGE('',*,*,#10189,.T.);
#14514=ORIENTED_EDGE('',*,*,#10190,.F.);
#14515=ORIENTED_EDGE('',*,*,#10191,.T.);
#14516=ORIENTED_EDGE('',*,*,#10187,.T.);
#14517=ORIENTED_EDGE('',*,*,#10192,.T.);
#14518=ORIENTED_EDGE('',*,*,#10193,.F.);
#14519=ORIENTED_EDGE('',*,*,#10194,.T.);
#14520=ORIENTED_EDGE('',*,*,#10190,.T.);
#14521=ORIENTED_EDGE('',*,*,#10195,.T.);
#14522=ORIENTED_EDGE('',*,*,#10196,.F.);
#14523=ORIENTED_EDGE('',*,*,#10197,.T.);
#14524=ORIENTED_EDGE('',*,*,#10193,.T.);
#14525=ORIENTED_EDGE('',*,*,#10198,.T.);
#14526=ORIENTED_EDGE('',*,*,#10199,.F.);
#14527=ORIENTED_EDGE('',*,*,#10200,.T.);
#14528=ORIENTED_EDGE('',*,*,#10196,.T.);
#14529=ORIENTED_EDGE('',*,*,#10201,.T.);
#14530=ORIENTED_EDGE('',*,*,#10202,.F.);
#14531=ORIENTED_EDGE('',*,*,#10203,.T.);
#14532=ORIENTED_EDGE('',*,*,#10199,.T.);
#14533=ORIENTED_EDGE('',*,*,#10204,.T.);
#14534=ORIENTED_EDGE('',*,*,#10205,.F.);
#14535=ORIENTED_EDGE('',*,*,#10206,.T.);
#14536=ORIENTED_EDGE('',*,*,#10202,.T.);
#14537=ORIENTED_EDGE('',*,*,#10207,.T.);
#14538=ORIENTED_EDGE('',*,*,#10208,.F.);
#14539=ORIENTED_EDGE('',*,*,#10209,.T.);
#14540=ORIENTED_EDGE('',*,*,#10205,.T.);
#14541=ORIENTED_EDGE('',*,*,#10210,.T.);
#14542=ORIENTED_EDGE('',*,*,#10211,.F.);
#14543=ORIENTED_EDGE('',*,*,#10212,.T.);
#14544=ORIENTED_EDGE('',*,*,#10208,.T.);
#14545=ORIENTED_EDGE('',*,*,#10213,.T.);
#14546=ORIENTED_EDGE('',*,*,#10214,.F.);
#14547=ORIENTED_EDGE('',*,*,#10215,.T.);
#14548=ORIENTED_EDGE('',*,*,#10211,.T.);
#14549=ORIENTED_EDGE('',*,*,#10216,.T.);
#14550=ORIENTED_EDGE('',*,*,#10217,.F.);
#14551=ORIENTED_EDGE('',*,*,#10218,.T.);
#14552=ORIENTED_EDGE('',*,*,#10214,.T.);
#14553=ORIENTED_EDGE('',*,*,#10219,.T.);
#14554=ORIENTED_EDGE('',*,*,#10220,.F.);
#14555=ORIENTED_EDGE('',*,*,#10221,.T.);
#14556=ORIENTED_EDGE('',*,*,#10217,.T.);
#14557=ORIENTED_EDGE('',*,*,#10222,.T.);
#14558=ORIENTED_EDGE('',*,*,#10223,.F.);
#14559=ORIENTED_EDGE('',*,*,#10224,.T.);
#14560=ORIENTED_EDGE('',*,*,#10220,.T.);
#14561=ORIENTED_EDGE('',*,*,#10225,.T.);
#14562=ORIENTED_EDGE('',*,*,#10226,.F.);
#14563=ORIENTED_EDGE('',*,*,#10227,.T.);
#14564=ORIENTED_EDGE('',*,*,#10223,.T.);
#14565=ORIENTED_EDGE('',*,*,#10228,.T.);
#14566=ORIENTED_EDGE('',*,*,#10229,.F.);
#14567=ORIENTED_EDGE('',*,*,#10230,.T.);
#14568=ORIENTED_EDGE('',*,*,#10226,.T.);
#14569=ORIENTED_EDGE('',*,*,#10231,.T.);
#14570=ORIENTED_EDGE('',*,*,#10232,.F.);
#14571=ORIENTED_EDGE('',*,*,#10233,.T.);
#14572=ORIENTED_EDGE('',*,*,#10229,.T.);
#14573=ORIENTED_EDGE('',*,*,#10234,.T.);
#14574=ORIENTED_EDGE('',*,*,#10235,.F.);
#14575=ORIENTED_EDGE('',*,*,#10236,.T.);
#14576=ORIENTED_EDGE('',*,*,#10232,.T.);
#14577=ORIENTED_EDGE('',*,*,#10237,.T.);
#14578=ORIENTED_EDGE('',*,*,#10238,.F.);
#14579=ORIENTED_EDGE('',*,*,#10239,.T.);
#14580=ORIENTED_EDGE('',*,*,#10235,.T.);
#14581=ORIENTED_EDGE('',*,*,#10240,.T.);
#14582=ORIENTED_EDGE('',*,*,#10241,.F.);
#14583=ORIENTED_EDGE('',*,*,#10242,.T.);
#14584=ORIENTED_EDGE('',*,*,#10238,.T.);
#14585=ORIENTED_EDGE('',*,*,#10243,.T.);
#14586=ORIENTED_EDGE('',*,*,#10244,.F.);
#14587=ORIENTED_EDGE('',*,*,#10245,.T.);
#14588=ORIENTED_EDGE('',*,*,#10241,.T.);
#14589=ORIENTED_EDGE('',*,*,#10246,.T.);
#14590=ORIENTED_EDGE('',*,*,#10247,.F.);
#14591=ORIENTED_EDGE('',*,*,#10248,.T.);
#14592=ORIENTED_EDGE('',*,*,#10244,.T.);
#14593=ORIENTED_EDGE('',*,*,#10249,.T.);
#14594=ORIENTED_EDGE('',*,*,#10250,.F.);
#14595=ORIENTED_EDGE('',*,*,#10251,.T.);
#14596=ORIENTED_EDGE('',*,*,#10247,.T.);
#14597=ORIENTED_EDGE('',*,*,#10252,.T.);
#14598=ORIENTED_EDGE('',*,*,#10253,.F.);
#14599=ORIENTED_EDGE('',*,*,#10254,.T.);
#14600=ORIENTED_EDGE('',*,*,#10250,.T.);
#14601=ORIENTED_EDGE('',*,*,#10255,.T.);
#14602=ORIENTED_EDGE('',*,*,#10256,.F.);
#14603=ORIENTED_EDGE('',*,*,#10257,.T.);
#14604=ORIENTED_EDGE('',*,*,#10253,.T.);
#14605=ORIENTED_EDGE('',*,*,#10258,.T.);
#14606=ORIENTED_EDGE('',*,*,#10259,.F.);
#14607=ORIENTED_EDGE('',*,*,#10260,.T.);
#14608=ORIENTED_EDGE('',*,*,#10256,.T.);
#14609=ORIENTED_EDGE('',*,*,#10261,.T.);
#14610=ORIENTED_EDGE('',*,*,#10262,.F.);
#14611=ORIENTED_EDGE('',*,*,#10263,.T.);
#14612=ORIENTED_EDGE('',*,*,#10259,.T.);
#14613=ORIENTED_EDGE('',*,*,#10264,.T.);
#14614=ORIENTED_EDGE('',*,*,#10265,.F.);
#14615=ORIENTED_EDGE('',*,*,#10266,.T.);
#14616=ORIENTED_EDGE('',*,*,#10262,.T.);
#14617=ORIENTED_EDGE('',*,*,#10267,.T.);
#14618=ORIENTED_EDGE('',*,*,#10268,.F.);
#14619=ORIENTED_EDGE('',*,*,#10269,.T.);
#14620=ORIENTED_EDGE('',*,*,#10265,.T.);
#14621=ORIENTED_EDGE('',*,*,#10270,.T.);
#14622=ORIENTED_EDGE('',*,*,#10271,.F.);
#14623=ORIENTED_EDGE('',*,*,#10272,.T.);
#14624=ORIENTED_EDGE('',*,*,#10268,.T.);
#14625=ORIENTED_EDGE('',*,*,#10273,.T.);
#14626=ORIENTED_EDGE('',*,*,#10274,.F.);
#14627=ORIENTED_EDGE('',*,*,#10275,.T.);
#14628=ORIENTED_EDGE('',*,*,#10271,.T.);
#14629=ORIENTED_EDGE('',*,*,#10276,.T.);
#14630=ORIENTED_EDGE('',*,*,#10277,.F.);
#14631=ORIENTED_EDGE('',*,*,#10278,.T.);
#14632=ORIENTED_EDGE('',*,*,#10274,.T.);
#14633=ORIENTED_EDGE('',*,*,#10279,.T.);
#14634=ORIENTED_EDGE('',*,*,#10280,.F.);
#14635=ORIENTED_EDGE('',*,*,#10281,.T.);
#14636=ORIENTED_EDGE('',*,*,#10277,.T.);
#14637=ORIENTED_EDGE('',*,*,#10282,.T.);
#14638=ORIENTED_EDGE('',*,*,#10283,.F.);
#14639=ORIENTED_EDGE('',*,*,#10284,.T.);
#14640=ORIENTED_EDGE('',*,*,#10280,.T.);
#14641=ORIENTED_EDGE('',*,*,#10285,.T.);
#14642=ORIENTED_EDGE('',*,*,#10286,.F.);
#14643=ORIENTED_EDGE('',*,*,#10287,.T.);
#14644=ORIENTED_EDGE('',*,*,#10283,.T.);
#14645=ORIENTED_EDGE('',*,*,#10288,.T.);
#14646=ORIENTED_EDGE('',*,*,#10289,.F.);
#14647=ORIENTED_EDGE('',*,*,#10290,.T.);
#14648=ORIENTED_EDGE('',*,*,#10286,.T.);
#14649=ORIENTED_EDGE('',*,*,#10291,.T.);
#14650=ORIENTED_EDGE('',*,*,#10292,.F.);
#14651=ORIENTED_EDGE('',*,*,#10293,.T.);
#14652=ORIENTED_EDGE('',*,*,#10289,.T.);
#14653=ORIENTED_EDGE('',*,*,#10294,.T.);
#14654=ORIENTED_EDGE('',*,*,#10295,.F.);
#14655=ORIENTED_EDGE('',*,*,#10296,.T.);
#14656=ORIENTED_EDGE('',*,*,#10292,.T.);
#14657=ORIENTED_EDGE('',*,*,#10297,.T.);
#14658=ORIENTED_EDGE('',*,*,#10298,.F.);
#14659=ORIENTED_EDGE('',*,*,#10299,.T.);
#14660=ORIENTED_EDGE('',*,*,#10295,.T.);
#14661=ORIENTED_EDGE('',*,*,#10300,.T.);
#14662=ORIENTED_EDGE('',*,*,#10301,.F.);
#14663=ORIENTED_EDGE('',*,*,#10302,.T.);
#14664=ORIENTED_EDGE('',*,*,#10298,.T.);
#14665=ORIENTED_EDGE('',*,*,#10303,.T.);
#14666=ORIENTED_EDGE('',*,*,#10304,.F.);
#14667=ORIENTED_EDGE('',*,*,#10305,.T.);
#14668=ORIENTED_EDGE('',*,*,#10301,.T.);
#14669=ORIENTED_EDGE('',*,*,#10306,.T.);
#14670=ORIENTED_EDGE('',*,*,#10307,.F.);
#14671=ORIENTED_EDGE('',*,*,#10308,.T.);
#14672=ORIENTED_EDGE('',*,*,#10304,.T.);
#14673=ORIENTED_EDGE('',*,*,#10309,.T.);
#14674=ORIENTED_EDGE('',*,*,#10310,.F.);
#14675=ORIENTED_EDGE('',*,*,#10311,.T.);
#14676=ORIENTED_EDGE('',*,*,#10307,.T.);
#14677=ORIENTED_EDGE('',*,*,#10312,.T.);
#14678=ORIENTED_EDGE('',*,*,#10313,.F.);
#14679=ORIENTED_EDGE('',*,*,#10314,.T.);
#14680=ORIENTED_EDGE('',*,*,#10310,.T.);
#14681=ORIENTED_EDGE('',*,*,#10315,.T.);
#14682=ORIENTED_EDGE('',*,*,#10316,.F.);
#14683=ORIENTED_EDGE('',*,*,#10317,.T.);
#14684=ORIENTED_EDGE('',*,*,#10313,.T.);
#14685=ORIENTED_EDGE('',*,*,#10318,.T.);
#14686=ORIENTED_EDGE('',*,*,#10319,.F.);
#14687=ORIENTED_EDGE('',*,*,#10320,.T.);
#14688=ORIENTED_EDGE('',*,*,#10316,.T.);
#14689=ORIENTED_EDGE('',*,*,#10321,.T.);
#14690=ORIENTED_EDGE('',*,*,#10322,.F.);
#14691=ORIENTED_EDGE('',*,*,#10323,.T.);
#14692=ORIENTED_EDGE('',*,*,#10319,.T.);
#14693=ORIENTED_EDGE('',*,*,#10324,.T.);
#14694=ORIENTED_EDGE('',*,*,#10325,.F.);
#14695=ORIENTED_EDGE('',*,*,#10326,.T.);
#14696=ORIENTED_EDGE('',*,*,#10322,.T.);
#14697=ORIENTED_EDGE('',*,*,#10327,.T.);
#14698=ORIENTED_EDGE('',*,*,#10328,.F.);
#14699=ORIENTED_EDGE('',*,*,#10329,.T.);
#14700=ORIENTED_EDGE('',*,*,#10325,.T.);
#14701=ORIENTED_EDGE('',*,*,#10330,.T.);
#14702=ORIENTED_EDGE('',*,*,#10331,.F.);
#14703=ORIENTED_EDGE('',*,*,#10332,.T.);
#14704=ORIENTED_EDGE('',*,*,#10328,.T.);
#14705=ORIENTED_EDGE('',*,*,#10333,.T.);
#14706=ORIENTED_EDGE('',*,*,#10334,.F.);
#14707=ORIENTED_EDGE('',*,*,#10335,.T.);
#14708=ORIENTED_EDGE('',*,*,#10331,.T.);
#14709=ORIENTED_EDGE('',*,*,#10336,.T.);
#14710=ORIENTED_EDGE('',*,*,#10337,.F.);
#14711=ORIENTED_EDGE('',*,*,#10338,.T.);
#14712=ORIENTED_EDGE('',*,*,#10334,.T.);
#14713=ORIENTED_EDGE('',*,*,#10339,.T.);
#14714=ORIENTED_EDGE('',*,*,#10340,.F.);
#14715=ORIENTED_EDGE('',*,*,#10341,.T.);
#14716=ORIENTED_EDGE('',*,*,#10337,.T.);
#14717=ORIENTED_EDGE('',*,*,#10342,.T.);
#14718=ORIENTED_EDGE('',*,*,#10343,.F.);
#14719=ORIENTED_EDGE('',*,*,#10344,.T.);
#14720=ORIENTED_EDGE('',*,*,#10340,.T.);
#14721=ORIENTED_EDGE('',*,*,#10345,.T.);
#14722=ORIENTED_EDGE('',*,*,#10346,.F.);
#14723=ORIENTED_EDGE('',*,*,#10347,.T.);
#14724=ORIENTED_EDGE('',*,*,#10343,.T.);
#14725=ORIENTED_EDGE('',*,*,#10348,.T.);
#14726=ORIENTED_EDGE('',*,*,#10349,.F.);
#14727=ORIENTED_EDGE('',*,*,#10350,.T.);
#14728=ORIENTED_EDGE('',*,*,#10346,.T.);
#14729=ORIENTED_EDGE('',*,*,#10351,.T.);
#14730=ORIENTED_EDGE('',*,*,#10352,.F.);
#14731=ORIENTED_EDGE('',*,*,#10353,.T.);
#14732=ORIENTED_EDGE('',*,*,#10349,.T.);
#14733=ORIENTED_EDGE('',*,*,#10354,.T.);
#14734=ORIENTED_EDGE('',*,*,#10355,.F.);
#14735=ORIENTED_EDGE('',*,*,#10356,.T.);
#14736=ORIENTED_EDGE('',*,*,#10352,.T.);
#14737=ORIENTED_EDGE('',*,*,#10357,.T.);
#14738=ORIENTED_EDGE('',*,*,#10358,.F.);
#14739=ORIENTED_EDGE('',*,*,#10359,.T.);
#14740=ORIENTED_EDGE('',*,*,#10355,.T.);
#14741=ORIENTED_EDGE('',*,*,#10360,.T.);
#14742=ORIENTED_EDGE('',*,*,#10361,.F.);
#14743=ORIENTED_EDGE('',*,*,#10362,.T.);
#14744=ORIENTED_EDGE('',*,*,#10358,.T.);
#14745=ORIENTED_EDGE('',*,*,#10363,.T.);
#14746=ORIENTED_EDGE('',*,*,#10364,.F.);
#14747=ORIENTED_EDGE('',*,*,#10365,.T.);
#14748=ORIENTED_EDGE('',*,*,#10361,.T.);
#14749=ORIENTED_EDGE('',*,*,#10366,.T.);
#14750=ORIENTED_EDGE('',*,*,#10367,.F.);
#14751=ORIENTED_EDGE('',*,*,#10368,.T.);
#14752=ORIENTED_EDGE('',*,*,#10364,.T.);
#14753=ORIENTED_EDGE('',*,*,#10369,.T.);
#14754=ORIENTED_EDGE('',*,*,#10370,.F.);
#14755=ORIENTED_EDGE('',*,*,#10371,.T.);
#14756=ORIENTED_EDGE('',*,*,#10367,.T.);
#14757=ORIENTED_EDGE('',*,*,#10372,.T.);
#14758=ORIENTED_EDGE('',*,*,#10373,.F.);
#14759=ORIENTED_EDGE('',*,*,#10374,.T.);
#14760=ORIENTED_EDGE('',*,*,#10370,.T.);
#14761=ORIENTED_EDGE('',*,*,#10375,.T.);
#14762=ORIENTED_EDGE('',*,*,#10376,.F.);
#14763=ORIENTED_EDGE('',*,*,#10377,.T.);
#14764=ORIENTED_EDGE('',*,*,#10373,.T.);
#14765=ORIENTED_EDGE('',*,*,#10378,.T.);
#14766=ORIENTED_EDGE('',*,*,#10379,.F.);
#14767=ORIENTED_EDGE('',*,*,#10380,.T.);
#14768=ORIENTED_EDGE('',*,*,#10381,.F.);
#14769=ORIENTED_EDGE('',*,*,#10382,.F.);
#14770=ORIENTED_EDGE('',*,*,#10383,.T.);
#14771=ORIENTED_EDGE('',*,*,#10379,.T.);
#14772=ORIENTED_EDGE('',*,*,#10384,.F.);
#14773=ORIENTED_EDGE('',*,*,#10385,.F.);
#14774=ORIENTED_EDGE('',*,*,#10386,.F.);
#14775=ORIENTED_EDGE('',*,*,#10387,.T.);
#14776=ORIENTED_EDGE('',*,*,#10382,.T.);
#14777=ORIENTED_EDGE('',*,*,#10388,.F.);
#14778=ORIENTED_EDGE('',*,*,#10389,.F.);
#14779=ORIENTED_EDGE('',*,*,#10390,.T.);
#14780=ORIENTED_EDGE('',*,*,#10386,.T.);
#14781=ORIENTED_EDGE('',*,*,#10391,.F.);
#14782=ORIENTED_EDGE('',*,*,#10392,.F.);
#14783=ORIENTED_EDGE('',*,*,#10393,.T.);
#14784=ORIENTED_EDGE('',*,*,#10389,.T.);
#14785=ORIENTED_EDGE('',*,*,#10394,.F.);
#14786=ORIENTED_EDGE('',*,*,#10395,.F.);
#14787=ORIENTED_EDGE('',*,*,#10396,.T.);
#14788=ORIENTED_EDGE('',*,*,#10392,.T.);
#14789=ORIENTED_EDGE('',*,*,#10397,.F.);
#14790=ORIENTED_EDGE('',*,*,#10398,.F.);
#14791=ORIENTED_EDGE('',*,*,#10399,.T.);
#14792=ORIENTED_EDGE('',*,*,#10395,.T.);
#14793=ORIENTED_EDGE('',*,*,#10400,.F.);
#14794=ORIENTED_EDGE('',*,*,#10401,.F.);
#14795=ORIENTED_EDGE('',*,*,#10402,.T.);
#14796=ORIENTED_EDGE('',*,*,#10398,.T.);
#14797=ORIENTED_EDGE('',*,*,#10403,.F.);
#14798=ORIENTED_EDGE('',*,*,#10404,.F.);
#14799=ORIENTED_EDGE('',*,*,#10405,.T.);
#14800=ORIENTED_EDGE('',*,*,#10401,.T.);
#14801=ORIENTED_EDGE('',*,*,#10406,.F.);
#14802=ORIENTED_EDGE('',*,*,#10407,.F.);
#14803=ORIENTED_EDGE('',*,*,#10408,.T.);
#14804=ORIENTED_EDGE('',*,*,#10404,.T.);
#14805=ORIENTED_EDGE('',*,*,#10409,.F.);
#14806=ORIENTED_EDGE('',*,*,#10410,.F.);
#14807=ORIENTED_EDGE('',*,*,#10411,.T.);
#14808=ORIENTED_EDGE('',*,*,#10407,.T.);
#14809=ORIENTED_EDGE('',*,*,#10412,.F.);
#14810=ORIENTED_EDGE('',*,*,#10413,.F.);
#14811=ORIENTED_EDGE('',*,*,#10414,.T.);
#14812=ORIENTED_EDGE('',*,*,#10410,.T.);
#14813=ORIENTED_EDGE('',*,*,#10415,.F.);
#14814=ORIENTED_EDGE('',*,*,#10416,.F.);
#14815=ORIENTED_EDGE('',*,*,#10417,.T.);
#14816=ORIENTED_EDGE('',*,*,#10413,.T.);
#14817=ORIENTED_EDGE('',*,*,#10418,.F.);
#14818=ORIENTED_EDGE('',*,*,#10419,.F.);
#14819=ORIENTED_EDGE('',*,*,#10420,.T.);
#14820=ORIENTED_EDGE('',*,*,#10416,.T.);
#14821=ORIENTED_EDGE('',*,*,#10421,.F.);
#14822=ORIENTED_EDGE('',*,*,#10422,.F.);
#14823=ORIENTED_EDGE('',*,*,#10423,.T.);
#14824=ORIENTED_EDGE('',*,*,#10419,.T.);
#14825=ORIENTED_EDGE('',*,*,#10424,.F.);
#14826=ORIENTED_EDGE('',*,*,#10425,.F.);
#14827=ORIENTED_EDGE('',*,*,#10426,.T.);
#14828=ORIENTED_EDGE('',*,*,#10422,.T.);
#14829=ORIENTED_EDGE('',*,*,#10427,.F.);
#14830=ORIENTED_EDGE('',*,*,#10428,.F.);
#14831=ORIENTED_EDGE('',*,*,#10429,.T.);
#14832=ORIENTED_EDGE('',*,*,#10425,.T.);
#14833=ORIENTED_EDGE('',*,*,#10430,.F.);
#14834=ORIENTED_EDGE('',*,*,#10431,.F.);
#14835=ORIENTED_EDGE('',*,*,#10432,.T.);
#14836=ORIENTED_EDGE('',*,*,#10428,.T.);
#14837=ORIENTED_EDGE('',*,*,#10433,.F.);
#14838=ORIENTED_EDGE('',*,*,#10434,.F.);
#14839=ORIENTED_EDGE('',*,*,#10435,.T.);
#14840=ORIENTED_EDGE('',*,*,#10431,.T.);
#14841=ORIENTED_EDGE('',*,*,#10436,.F.);
#14842=ORIENTED_EDGE('',*,*,#10437,.F.);
#14843=ORIENTED_EDGE('',*,*,#10438,.T.);
#14844=ORIENTED_EDGE('',*,*,#10434,.T.);
#14845=ORIENTED_EDGE('',*,*,#10439,.F.);
#14846=ORIENTED_EDGE('',*,*,#10440,.F.);
#14847=ORIENTED_EDGE('',*,*,#10441,.T.);
#14848=ORIENTED_EDGE('',*,*,#10437,.T.);
#14849=ORIENTED_EDGE('',*,*,#10442,.F.);
#14850=ORIENTED_EDGE('',*,*,#10443,.F.);
#14851=ORIENTED_EDGE('',*,*,#10444,.T.);
#14852=ORIENTED_EDGE('',*,*,#10440,.T.);
#14853=ORIENTED_EDGE('',*,*,#10445,.F.);
#14854=ORIENTED_EDGE('',*,*,#10446,.F.);
#14855=ORIENTED_EDGE('',*,*,#10447,.T.);
#14856=ORIENTED_EDGE('',*,*,#10443,.T.);
#14857=ORIENTED_EDGE('',*,*,#10448,.F.);
#14858=ORIENTED_EDGE('',*,*,#10449,.F.);
#14859=ORIENTED_EDGE('',*,*,#10450,.T.);
#14860=ORIENTED_EDGE('',*,*,#10446,.T.);
#14861=ORIENTED_EDGE('',*,*,#10451,.F.);
#14862=ORIENTED_EDGE('',*,*,#10452,.F.);
#14863=ORIENTED_EDGE('',*,*,#10453,.T.);
#14864=ORIENTED_EDGE('',*,*,#10449,.T.);
#14865=ORIENTED_EDGE('',*,*,#10454,.F.);
#14866=ORIENTED_EDGE('',*,*,#10455,.F.);
#14867=ORIENTED_EDGE('',*,*,#10456,.T.);
#14868=ORIENTED_EDGE('',*,*,#10452,.T.);
#14869=ORIENTED_EDGE('',*,*,#10457,.F.);
#14870=ORIENTED_EDGE('',*,*,#10458,.F.);
#14871=ORIENTED_EDGE('',*,*,#10459,.T.);
#14872=ORIENTED_EDGE('',*,*,#10455,.T.);
#14873=ORIENTED_EDGE('',*,*,#10460,.F.);
#14874=ORIENTED_EDGE('',*,*,#10461,.F.);
#14875=ORIENTED_EDGE('',*,*,#10462,.T.);
#14876=ORIENTED_EDGE('',*,*,#10458,.T.);
#14877=ORIENTED_EDGE('',*,*,#10463,.F.);
#14878=ORIENTED_EDGE('',*,*,#10464,.F.);
#14879=ORIENTED_EDGE('',*,*,#10465,.T.);
#14880=ORIENTED_EDGE('',*,*,#10461,.T.);
#14881=ORIENTED_EDGE('',*,*,#10466,.F.);
#14882=ORIENTED_EDGE('',*,*,#10467,.F.);
#14883=ORIENTED_EDGE('',*,*,#10468,.T.);
#14884=ORIENTED_EDGE('',*,*,#10464,.T.);
#14885=ORIENTED_EDGE('',*,*,#10469,.F.);
#14886=ORIENTED_EDGE('',*,*,#10470,.F.);
#14887=ORIENTED_EDGE('',*,*,#10471,.T.);
#14888=ORIENTED_EDGE('',*,*,#10467,.T.);
#14889=ORIENTED_EDGE('',*,*,#10472,.F.);
#14890=ORIENTED_EDGE('',*,*,#10473,.F.);
#14891=ORIENTED_EDGE('',*,*,#10474,.T.);
#14892=ORIENTED_EDGE('',*,*,#10470,.T.);
#14893=ORIENTED_EDGE('',*,*,#10475,.F.);
#14894=ORIENTED_EDGE('',*,*,#10476,.F.);
#14895=ORIENTED_EDGE('',*,*,#10477,.T.);
#14896=ORIENTED_EDGE('',*,*,#10473,.T.);
#14897=ORIENTED_EDGE('',*,*,#10478,.F.);
#14898=ORIENTED_EDGE('',*,*,#10479,.F.);
#14899=ORIENTED_EDGE('',*,*,#10480,.T.);
#14900=ORIENTED_EDGE('',*,*,#10476,.T.);
#14901=ORIENTED_EDGE('',*,*,#10481,.F.);
#14902=ORIENTED_EDGE('',*,*,#10482,.F.);
#14903=ORIENTED_EDGE('',*,*,#10483,.T.);
#14904=ORIENTED_EDGE('',*,*,#10479,.T.);
#14905=ORIENTED_EDGE('',*,*,#10484,.F.);
#14906=ORIENTED_EDGE('',*,*,#10485,.F.);
#14907=ORIENTED_EDGE('',*,*,#10486,.T.);
#14908=ORIENTED_EDGE('',*,*,#10482,.T.);
#14909=ORIENTED_EDGE('',*,*,#10487,.F.);
#14910=ORIENTED_EDGE('',*,*,#10488,.F.);
#14911=ORIENTED_EDGE('',*,*,#10489,.T.);
#14912=ORIENTED_EDGE('',*,*,#10485,.T.);
#14913=ORIENTED_EDGE('',*,*,#10490,.F.);
#14914=ORIENTED_EDGE('',*,*,#10491,.F.);
#14915=ORIENTED_EDGE('',*,*,#10492,.T.);
#14916=ORIENTED_EDGE('',*,*,#10488,.T.);
#14917=ORIENTED_EDGE('',*,*,#10493,.F.);
#14918=ORIENTED_EDGE('',*,*,#10494,.F.);
#14919=ORIENTED_EDGE('',*,*,#10495,.T.);
#14920=ORIENTED_EDGE('',*,*,#10491,.T.);
#14921=ORIENTED_EDGE('',*,*,#10496,.F.);
#14922=ORIENTED_EDGE('',*,*,#10497,.F.);
#14923=ORIENTED_EDGE('',*,*,#10498,.T.);
#14924=ORIENTED_EDGE('',*,*,#10494,.T.);
#14925=ORIENTED_EDGE('',*,*,#10499,.F.);
#14926=ORIENTED_EDGE('',*,*,#10500,.F.);
#14927=ORIENTED_EDGE('',*,*,#10501,.T.);
#14928=ORIENTED_EDGE('',*,*,#10497,.T.);
#14929=ORIENTED_EDGE('',*,*,#10502,.F.);
#14930=ORIENTED_EDGE('',*,*,#10503,.F.);
#14931=ORIENTED_EDGE('',*,*,#10504,.T.);
#14932=ORIENTED_EDGE('',*,*,#10500,.T.);
#14933=ORIENTED_EDGE('',*,*,#10505,.F.);
#14934=ORIENTED_EDGE('',*,*,#10506,.F.);
#14935=ORIENTED_EDGE('',*,*,#10507,.T.);
#14936=ORIENTED_EDGE('',*,*,#10503,.T.);
#14937=ORIENTED_EDGE('',*,*,#10508,.F.);
#14938=ORIENTED_EDGE('',*,*,#10509,.F.);
#14939=ORIENTED_EDGE('',*,*,#10510,.T.);
#14940=ORIENTED_EDGE('',*,*,#10506,.T.);
#14941=ORIENTED_EDGE('',*,*,#10511,.F.);
#14942=ORIENTED_EDGE('',*,*,#10512,.F.);
#14943=ORIENTED_EDGE('',*,*,#10513,.T.);
#14944=ORIENTED_EDGE('',*,*,#10509,.T.);
#14945=ORIENTED_EDGE('',*,*,#10514,.F.);
#14946=ORIENTED_EDGE('',*,*,#10515,.F.);
#14947=ORIENTED_EDGE('',*,*,#10516,.T.);
#14948=ORIENTED_EDGE('',*,*,#10512,.T.);
#14949=ORIENTED_EDGE('',*,*,#10517,.F.);
#14950=ORIENTED_EDGE('',*,*,#10518,.F.);
#14951=ORIENTED_EDGE('',*,*,#10519,.T.);
#14952=ORIENTED_EDGE('',*,*,#10515,.T.);
#14953=ORIENTED_EDGE('',*,*,#10520,.F.);
#14954=ORIENTED_EDGE('',*,*,#10521,.F.);
#14955=ORIENTED_EDGE('',*,*,#10522,.T.);
#14956=ORIENTED_EDGE('',*,*,#10518,.T.);
#14957=ORIENTED_EDGE('',*,*,#10523,.F.);
#14958=ORIENTED_EDGE('',*,*,#10524,.F.);
#14959=ORIENTED_EDGE('',*,*,#10525,.T.);
#14960=ORIENTED_EDGE('',*,*,#10521,.T.);
#14961=ORIENTED_EDGE('',*,*,#10526,.F.);
#14962=ORIENTED_EDGE('',*,*,#10527,.F.);
#14963=ORIENTED_EDGE('',*,*,#10528,.T.);
#14964=ORIENTED_EDGE('',*,*,#10524,.T.);
#14965=ORIENTED_EDGE('',*,*,#10529,.F.);
#14966=ORIENTED_EDGE('',*,*,#10530,.F.);
#14967=ORIENTED_EDGE('',*,*,#10531,.T.);
#14968=ORIENTED_EDGE('',*,*,#10527,.T.);
#14969=ORIENTED_EDGE('',*,*,#10532,.F.);
#14970=ORIENTED_EDGE('',*,*,#10533,.F.);
#14971=ORIENTED_EDGE('',*,*,#10534,.T.);
#14972=ORIENTED_EDGE('',*,*,#10530,.T.);
#14973=ORIENTED_EDGE('',*,*,#10535,.F.);
#14974=ORIENTED_EDGE('',*,*,#10536,.F.);
#14975=ORIENTED_EDGE('',*,*,#10537,.T.);
#14976=ORIENTED_EDGE('',*,*,#10533,.T.);
#14977=ORIENTED_EDGE('',*,*,#10538,.F.);
#14978=ORIENTED_EDGE('',*,*,#10539,.F.);
#14979=ORIENTED_EDGE('',*,*,#10540,.T.);
#14980=ORIENTED_EDGE('',*,*,#10536,.T.);
#14981=ORIENTED_EDGE('',*,*,#10541,.F.);
#14982=ORIENTED_EDGE('',*,*,#10542,.F.);
#14983=ORIENTED_EDGE('',*,*,#10543,.T.);
#14984=ORIENTED_EDGE('',*,*,#10539,.T.);
#14985=ORIENTED_EDGE('',*,*,#10544,.F.);
#14986=ORIENTED_EDGE('',*,*,#10545,.F.);
#14987=ORIENTED_EDGE('',*,*,#10546,.T.);
#14988=ORIENTED_EDGE('',*,*,#10542,.T.);
#14989=ORIENTED_EDGE('',*,*,#10547,.F.);
#14990=ORIENTED_EDGE('',*,*,#10548,.F.);
#14991=ORIENTED_EDGE('',*,*,#10549,.T.);
#14992=ORIENTED_EDGE('',*,*,#10545,.T.);
#14993=ORIENTED_EDGE('',*,*,#10550,.F.);
#14994=ORIENTED_EDGE('',*,*,#10551,.F.);
#14995=ORIENTED_EDGE('',*,*,#10552,.T.);
#14996=ORIENTED_EDGE('',*,*,#10548,.T.);
#14997=ORIENTED_EDGE('',*,*,#10553,.F.);
#14998=ORIENTED_EDGE('',*,*,#10554,.F.);
#14999=ORIENTED_EDGE('',*,*,#10555,.T.);
#15000=ORIENTED_EDGE('',*,*,#10551,.T.);
#15001=ORIENTED_EDGE('',*,*,#10556,.F.);
#15002=ORIENTED_EDGE('',*,*,#10557,.F.);
#15003=ORIENTED_EDGE('',*,*,#10558,.T.);
#15004=ORIENTED_EDGE('',*,*,#10554,.T.);
#15005=ORIENTED_EDGE('',*,*,#10559,.F.);
#15006=ORIENTED_EDGE('',*,*,#10560,.F.);
#15007=ORIENTED_EDGE('',*,*,#10561,.T.);
#15008=ORIENTED_EDGE('',*,*,#10557,.T.);
#15009=ORIENTED_EDGE('',*,*,#10562,.F.);
#15010=ORIENTED_EDGE('',*,*,#10563,.F.);
#15011=ORIENTED_EDGE('',*,*,#10564,.T.);
#15012=ORIENTED_EDGE('',*,*,#10560,.T.);
#15013=ORIENTED_EDGE('',*,*,#10565,.F.);
#15014=ORIENTED_EDGE('',*,*,#10566,.F.);
#15015=ORIENTED_EDGE('',*,*,#10567,.T.);
#15016=ORIENTED_EDGE('',*,*,#10563,.T.);
#15017=ORIENTED_EDGE('',*,*,#10568,.F.);
#15018=ORIENTED_EDGE('',*,*,#10569,.F.);
#15019=ORIENTED_EDGE('',*,*,#10570,.T.);
#15020=ORIENTED_EDGE('',*,*,#10566,.T.);
#15021=ORIENTED_EDGE('',*,*,#10571,.F.);
#15022=ORIENTED_EDGE('',*,*,#10572,.F.);
#15023=ORIENTED_EDGE('',*,*,#10573,.T.);
#15024=ORIENTED_EDGE('',*,*,#10569,.T.);
#15025=ORIENTED_EDGE('',*,*,#10574,.F.);
#15026=ORIENTED_EDGE('',*,*,#10575,.F.);
#15027=ORIENTED_EDGE('',*,*,#10576,.T.);
#15028=ORIENTED_EDGE('',*,*,#10572,.T.);
#15029=ORIENTED_EDGE('',*,*,#10577,.F.);
#15030=ORIENTED_EDGE('',*,*,#10578,.F.);
#15031=ORIENTED_EDGE('',*,*,#10579,.T.);
#15032=ORIENTED_EDGE('',*,*,#10575,.T.);
#15033=ORIENTED_EDGE('',*,*,#10580,.F.);
#15034=ORIENTED_EDGE('',*,*,#10581,.F.);
#15035=ORIENTED_EDGE('',*,*,#10582,.T.);
#15036=ORIENTED_EDGE('',*,*,#10578,.T.);
#15037=ORIENTED_EDGE('',*,*,#10583,.F.);
#15038=ORIENTED_EDGE('',*,*,#10584,.F.);
#15039=ORIENTED_EDGE('',*,*,#10585,.T.);
#15040=ORIENTED_EDGE('',*,*,#10581,.T.);
#15041=ORIENTED_EDGE('',*,*,#10586,.F.);
#15042=ORIENTED_EDGE('',*,*,#10587,.F.);
#15043=ORIENTED_EDGE('',*,*,#10588,.T.);
#15044=ORIENTED_EDGE('',*,*,#10584,.T.);
#15045=ORIENTED_EDGE('',*,*,#10589,.F.);
#15046=ORIENTED_EDGE('',*,*,#10590,.F.);
#15047=ORIENTED_EDGE('',*,*,#10591,.T.);
#15048=ORIENTED_EDGE('',*,*,#10587,.T.);
#15049=ORIENTED_EDGE('',*,*,#10592,.F.);
#15050=ORIENTED_EDGE('',*,*,#10593,.F.);
#15051=ORIENTED_EDGE('',*,*,#10594,.T.);
#15052=ORIENTED_EDGE('',*,*,#10590,.T.);
#15053=ORIENTED_EDGE('',*,*,#10595,.F.);
#15054=ORIENTED_EDGE('',*,*,#10596,.F.);
#15055=ORIENTED_EDGE('',*,*,#10597,.T.);
#15056=ORIENTED_EDGE('',*,*,#10593,.T.);
#15057=ORIENTED_EDGE('',*,*,#10598,.F.);
#15058=ORIENTED_EDGE('',*,*,#10599,.F.);
#15059=ORIENTED_EDGE('',*,*,#10600,.T.);
#15060=ORIENTED_EDGE('',*,*,#10596,.T.);
#15061=ORIENTED_EDGE('',*,*,#10601,.F.);
#15062=ORIENTED_EDGE('',*,*,#10602,.F.);
#15063=ORIENTED_EDGE('',*,*,#10603,.T.);
#15064=ORIENTED_EDGE('',*,*,#10599,.T.);
#15065=ORIENTED_EDGE('',*,*,#10604,.F.);
#15066=ORIENTED_EDGE('',*,*,#10605,.F.);
#15067=ORIENTED_EDGE('',*,*,#10606,.T.);
#15068=ORIENTED_EDGE('',*,*,#10602,.T.);
#15069=ORIENTED_EDGE('',*,*,#10607,.F.);
#15070=ORIENTED_EDGE('',*,*,#10608,.F.);
#15071=ORIENTED_EDGE('',*,*,#10609,.T.);
#15072=ORIENTED_EDGE('',*,*,#10605,.T.);
#15073=ORIENTED_EDGE('',*,*,#10610,.F.);
#15074=ORIENTED_EDGE('',*,*,#10611,.F.);
#15075=ORIENTED_EDGE('',*,*,#10612,.T.);
#15076=ORIENTED_EDGE('',*,*,#10608,.T.);
#15077=ORIENTED_EDGE('',*,*,#10613,.F.);
#15078=ORIENTED_EDGE('',*,*,#10614,.F.);
#15079=ORIENTED_EDGE('',*,*,#10615,.T.);
#15080=ORIENTED_EDGE('',*,*,#10611,.T.);
#15081=ORIENTED_EDGE('',*,*,#10616,.F.);
#15082=ORIENTED_EDGE('',*,*,#10617,.F.);
#15083=ORIENTED_EDGE('',*,*,#10618,.T.);
#15084=ORIENTED_EDGE('',*,*,#10614,.T.);
#15085=ORIENTED_EDGE('',*,*,#10619,.F.);
#15086=ORIENTED_EDGE('',*,*,#10620,.F.);
#15087=ORIENTED_EDGE('',*,*,#10621,.T.);
#15088=ORIENTED_EDGE('',*,*,#10617,.T.);
#15089=ORIENTED_EDGE('',*,*,#10622,.F.);
#15090=ORIENTED_EDGE('',*,*,#10623,.F.);
#15091=ORIENTED_EDGE('',*,*,#10624,.T.);
#15092=ORIENTED_EDGE('',*,*,#10620,.T.);
#15093=ORIENTED_EDGE('',*,*,#10625,.F.);
#15094=ORIENTED_EDGE('',*,*,#10626,.F.);
#15095=ORIENTED_EDGE('',*,*,#10627,.T.);
#15096=ORIENTED_EDGE('',*,*,#10623,.T.);
#15097=ORIENTED_EDGE('',*,*,#10628,.F.);
#15098=ORIENTED_EDGE('',*,*,#10629,.F.);
#15099=ORIENTED_EDGE('',*,*,#10630,.T.);
#15100=ORIENTED_EDGE('',*,*,#10626,.T.);
#15101=ORIENTED_EDGE('',*,*,#10631,.F.);
#15102=ORIENTED_EDGE('',*,*,#10632,.F.);
#15103=ORIENTED_EDGE('',*,*,#10633,.T.);
#15104=ORIENTED_EDGE('',*,*,#10629,.T.);
#15105=ORIENTED_EDGE('',*,*,#10634,.F.);
#15106=ORIENTED_EDGE('',*,*,#10635,.F.);
#15107=ORIENTED_EDGE('',*,*,#10636,.T.);
#15108=ORIENTED_EDGE('',*,*,#10632,.T.);
#15109=ORIENTED_EDGE('',*,*,#10637,.F.);
#15110=ORIENTED_EDGE('',*,*,#10638,.F.);
#15111=ORIENTED_EDGE('',*,*,#10639,.T.);
#15112=ORIENTED_EDGE('',*,*,#10635,.T.);
#15113=ORIENTED_EDGE('',*,*,#10640,.F.);
#15114=ORIENTED_EDGE('',*,*,#10641,.F.);
#15115=ORIENTED_EDGE('',*,*,#10642,.T.);
#15116=ORIENTED_EDGE('',*,*,#10638,.T.);
#15117=ORIENTED_EDGE('',*,*,#10643,.F.);
#15118=ORIENTED_EDGE('',*,*,#10644,.F.);
#15119=ORIENTED_EDGE('',*,*,#10645,.F.);
#15120=ORIENTED_EDGE('',*,*,#10378,.F.);
#15121=ORIENTED_EDGE('',*,*,#10375,.F.);
#15122=ORIENTED_EDGE('',*,*,#10372,.F.);
#15123=ORIENTED_EDGE('',*,*,#10369,.F.);
#15124=ORIENTED_EDGE('',*,*,#10366,.F.);
#15125=ORIENTED_EDGE('',*,*,#10363,.F.);
#15126=ORIENTED_EDGE('',*,*,#10360,.F.);
#15127=ORIENTED_EDGE('',*,*,#10357,.F.);
#15128=ORIENTED_EDGE('',*,*,#10354,.F.);
#15129=ORIENTED_EDGE('',*,*,#10351,.F.);
#15130=ORIENTED_EDGE('',*,*,#10348,.F.);
#15131=ORIENTED_EDGE('',*,*,#10345,.F.);
#15132=ORIENTED_EDGE('',*,*,#10342,.F.);
#15133=ORIENTED_EDGE('',*,*,#10339,.F.);
#15134=ORIENTED_EDGE('',*,*,#10336,.F.);
#15135=ORIENTED_EDGE('',*,*,#10333,.F.);
#15136=ORIENTED_EDGE('',*,*,#10330,.F.);
#15137=ORIENTED_EDGE('',*,*,#10327,.F.);
#15138=ORIENTED_EDGE('',*,*,#10324,.F.);
#15139=ORIENTED_EDGE('',*,*,#10321,.F.);
#15140=ORIENTED_EDGE('',*,*,#10318,.F.);
#15141=ORIENTED_EDGE('',*,*,#10315,.F.);
#15142=ORIENTED_EDGE('',*,*,#10312,.F.);
#15143=ORIENTED_EDGE('',*,*,#10309,.F.);
#15144=ORIENTED_EDGE('',*,*,#10306,.F.);
#15145=ORIENTED_EDGE('',*,*,#10303,.F.);
#15146=ORIENTED_EDGE('',*,*,#10300,.F.);
#15147=ORIENTED_EDGE('',*,*,#10297,.F.);
#15148=ORIENTED_EDGE('',*,*,#10294,.F.);
#15149=ORIENTED_EDGE('',*,*,#10291,.F.);
#15150=ORIENTED_EDGE('',*,*,#10288,.F.);
#15151=ORIENTED_EDGE('',*,*,#10285,.F.);
#15152=ORIENTED_EDGE('',*,*,#10282,.F.);
#15153=ORIENTED_EDGE('',*,*,#10279,.F.);
#15154=ORIENTED_EDGE('',*,*,#10276,.F.);
#15155=ORIENTED_EDGE('',*,*,#10273,.F.);
#15156=ORIENTED_EDGE('',*,*,#10270,.F.);
#15157=ORIENTED_EDGE('',*,*,#10267,.F.);
#15158=ORIENTED_EDGE('',*,*,#10264,.F.);
#15159=ORIENTED_EDGE('',*,*,#10261,.F.);
#15160=ORIENTED_EDGE('',*,*,#10258,.F.);
#15161=ORIENTED_EDGE('',*,*,#10255,.F.);
#15162=ORIENTED_EDGE('',*,*,#10252,.F.);
#15163=ORIENTED_EDGE('',*,*,#10249,.F.);
#15164=ORIENTED_EDGE('',*,*,#10246,.F.);
#15165=ORIENTED_EDGE('',*,*,#10243,.F.);
#15166=ORIENTED_EDGE('',*,*,#10240,.F.);
#15167=ORIENTED_EDGE('',*,*,#10237,.F.);
#15168=ORIENTED_EDGE('',*,*,#10234,.F.);
#15169=ORIENTED_EDGE('',*,*,#10231,.F.);
#15170=ORIENTED_EDGE('',*,*,#10228,.F.);
#15171=ORIENTED_EDGE('',*,*,#10225,.F.);
#15172=ORIENTED_EDGE('',*,*,#10222,.F.);
#15173=ORIENTED_EDGE('',*,*,#10219,.F.);
#15174=ORIENTED_EDGE('',*,*,#10216,.F.);
#15175=ORIENTED_EDGE('',*,*,#10213,.F.);
#15176=ORIENTED_EDGE('',*,*,#10210,.F.);
#15177=ORIENTED_EDGE('',*,*,#10207,.F.);
#15178=ORIENTED_EDGE('',*,*,#10204,.F.);
#15179=ORIENTED_EDGE('',*,*,#10201,.F.);
#15180=ORIENTED_EDGE('',*,*,#10198,.F.);
#15181=ORIENTED_EDGE('',*,*,#10195,.F.);
#15182=ORIENTED_EDGE('',*,*,#10192,.F.);
#15183=ORIENTED_EDGE('',*,*,#10189,.F.);
#15184=ORIENTED_EDGE('',*,*,#10186,.F.);
#15185=ORIENTED_EDGE('',*,*,#10183,.F.);
#15186=ORIENTED_EDGE('',*,*,#10180,.F.);
#15187=ORIENTED_EDGE('',*,*,#10177,.F.);
#15188=ORIENTED_EDGE('',*,*,#10174,.F.);
#15189=ORIENTED_EDGE('',*,*,#10171,.F.);
#15190=ORIENTED_EDGE('',*,*,#10168,.F.);
#15191=ORIENTED_EDGE('',*,*,#10165,.F.);
#15192=ORIENTED_EDGE('',*,*,#10162,.F.);
#15193=ORIENTED_EDGE('',*,*,#10159,.F.);
#15194=ORIENTED_EDGE('',*,*,#10156,.F.);
#15195=ORIENTED_EDGE('',*,*,#10153,.F.);
#15196=ORIENTED_EDGE('',*,*,#10150,.F.);
#15197=ORIENTED_EDGE('',*,*,#10147,.F.);
#15198=ORIENTED_EDGE('',*,*,#10144,.F.);
#15199=ORIENTED_EDGE('',*,*,#10141,.F.);
#15200=ORIENTED_EDGE('',*,*,#10138,.F.);
#15201=ORIENTED_EDGE('',*,*,#10135,.F.);
#15202=ORIENTED_EDGE('',*,*,#10132,.F.);
#15203=ORIENTED_EDGE('',*,*,#10129,.F.);
#15204=ORIENTED_EDGE('',*,*,#10126,.F.);
#15205=ORIENTED_EDGE('',*,*,#10123,.F.);
#15206=ORIENTED_EDGE('',*,*,#10120,.F.);
#15207=ORIENTED_EDGE('',*,*,#10117,.F.);
#15208=ORIENTED_EDGE('',*,*,#10646,.F.);
#15209=ORIENTED_EDGE('',*,*,#10647,.T.);
#15210=ORIENTED_EDGE('',*,*,#10643,.T.);
#15211=ORIENTED_EDGE('',*,*,#10640,.T.);
#15212=ORIENTED_EDGE('',*,*,#10637,.T.);
#15213=ORIENTED_EDGE('',*,*,#10634,.T.);
#15214=ORIENTED_EDGE('',*,*,#10631,.T.);
#15215=ORIENTED_EDGE('',*,*,#10628,.T.);
#15216=ORIENTED_EDGE('',*,*,#10625,.T.);
#15217=ORIENTED_EDGE('',*,*,#10622,.T.);
#15218=ORIENTED_EDGE('',*,*,#10619,.T.);
#15219=ORIENTED_EDGE('',*,*,#10616,.T.);
#15220=ORIENTED_EDGE('',*,*,#10613,.T.);
#15221=ORIENTED_EDGE('',*,*,#10610,.T.);
#15222=ORIENTED_EDGE('',*,*,#10607,.T.);
#15223=ORIENTED_EDGE('',*,*,#10604,.T.);
#15224=ORIENTED_EDGE('',*,*,#10601,.T.);
#15225=ORIENTED_EDGE('',*,*,#10598,.T.);
#15226=ORIENTED_EDGE('',*,*,#10595,.T.);
#15227=ORIENTED_EDGE('',*,*,#10592,.T.);
#15228=ORIENTED_EDGE('',*,*,#10589,.T.);
#15229=ORIENTED_EDGE('',*,*,#10586,.T.);
#15230=ORIENTED_EDGE('',*,*,#10583,.T.);
#15231=ORIENTED_EDGE('',*,*,#10580,.T.);
#15232=ORIENTED_EDGE('',*,*,#10577,.T.);
#15233=ORIENTED_EDGE('',*,*,#10574,.T.);
#15234=ORIENTED_EDGE('',*,*,#10571,.T.);
#15235=ORIENTED_EDGE('',*,*,#10568,.T.);
#15236=ORIENTED_EDGE('',*,*,#10565,.T.);
#15237=ORIENTED_EDGE('',*,*,#10562,.T.);
#15238=ORIENTED_EDGE('',*,*,#10559,.T.);
#15239=ORIENTED_EDGE('',*,*,#10556,.T.);
#15240=ORIENTED_EDGE('',*,*,#10553,.T.);
#15241=ORIENTED_EDGE('',*,*,#10550,.T.);
#15242=ORIENTED_EDGE('',*,*,#10547,.T.);
#15243=ORIENTED_EDGE('',*,*,#10544,.T.);
#15244=ORIENTED_EDGE('',*,*,#10541,.T.);
#15245=ORIENTED_EDGE('',*,*,#10538,.T.);
#15246=ORIENTED_EDGE('',*,*,#10535,.T.);
#15247=ORIENTED_EDGE('',*,*,#10532,.T.);
#15248=ORIENTED_EDGE('',*,*,#10529,.T.);
#15249=ORIENTED_EDGE('',*,*,#10526,.T.);
#15250=ORIENTED_EDGE('',*,*,#10523,.T.);
#15251=ORIENTED_EDGE('',*,*,#10520,.T.);
#15252=ORIENTED_EDGE('',*,*,#10517,.T.);
#15253=ORIENTED_EDGE('',*,*,#10514,.T.);
#15254=ORIENTED_EDGE('',*,*,#10511,.T.);
#15255=ORIENTED_EDGE('',*,*,#10508,.T.);
#15256=ORIENTED_EDGE('',*,*,#10505,.T.);
#15257=ORIENTED_EDGE('',*,*,#10502,.T.);
#15258=ORIENTED_EDGE('',*,*,#10499,.T.);
#15259=ORIENTED_EDGE('',*,*,#10496,.T.);
#15260=ORIENTED_EDGE('',*,*,#10493,.T.);
#15261=ORIENTED_EDGE('',*,*,#10490,.T.);
#15262=ORIENTED_EDGE('',*,*,#10487,.T.);
#15263=ORIENTED_EDGE('',*,*,#10484,.T.);
#15264=ORIENTED_EDGE('',*,*,#10481,.T.);
#15265=ORIENTED_EDGE('',*,*,#10478,.T.);
#15266=ORIENTED_EDGE('',*,*,#10475,.T.);
#15267=ORIENTED_EDGE('',*,*,#10472,.T.);
#15268=ORIENTED_EDGE('',*,*,#10469,.T.);
#15269=ORIENTED_EDGE('',*,*,#10466,.T.);
#15270=ORIENTED_EDGE('',*,*,#10463,.T.);
#15271=ORIENTED_EDGE('',*,*,#10460,.T.);
#15272=ORIENTED_EDGE('',*,*,#10457,.T.);
#15273=ORIENTED_EDGE('',*,*,#10454,.T.);
#15274=ORIENTED_EDGE('',*,*,#10451,.T.);
#15275=ORIENTED_EDGE('',*,*,#10448,.T.);
#15276=ORIENTED_EDGE('',*,*,#10445,.T.);
#15277=ORIENTED_EDGE('',*,*,#10442,.T.);
#15278=ORIENTED_EDGE('',*,*,#10439,.T.);
#15279=ORIENTED_EDGE('',*,*,#10436,.T.);
#15280=ORIENTED_EDGE('',*,*,#10433,.T.);
#15281=ORIENTED_EDGE('',*,*,#10430,.T.);
#15282=ORIENTED_EDGE('',*,*,#10427,.T.);
#15283=ORIENTED_EDGE('',*,*,#10424,.T.);
#15284=ORIENTED_EDGE('',*,*,#10421,.T.);
#15285=ORIENTED_EDGE('',*,*,#10418,.T.);
#15286=ORIENTED_EDGE('',*,*,#10415,.T.);
#15287=ORIENTED_EDGE('',*,*,#10412,.T.);
#15288=ORIENTED_EDGE('',*,*,#10409,.T.);
#15289=ORIENTED_EDGE('',*,*,#10406,.T.);
#15290=ORIENTED_EDGE('',*,*,#10403,.T.);
#15291=ORIENTED_EDGE('',*,*,#10400,.T.);
#15292=ORIENTED_EDGE('',*,*,#10397,.T.);
#15293=ORIENTED_EDGE('',*,*,#10394,.T.);
#15294=ORIENTED_EDGE('',*,*,#10391,.T.);
#15295=ORIENTED_EDGE('',*,*,#10388,.T.);
#15296=ORIENTED_EDGE('',*,*,#10385,.T.);
#15297=ORIENTED_EDGE('',*,*,#10648,.T.);
#15298=ORIENTED_EDGE('',*,*,#10649,.T.);
#15299=ORIENTED_EDGE('',*,*,#10650,.T.);
#15300=ORIENTED_EDGE('',*,*,#10651,.T.);
#15301=ORIENTED_EDGE('',*,*,#10646,.T.);
#15302=ORIENTED_EDGE('',*,*,#10641,.T.);
#15303=ORIENTED_EDGE('',*,*,#10647,.F.);
#15304=ORIENTED_EDGE('',*,*,#10651,.F.);
#15305=ORIENTED_EDGE('',*,*,#10652,.T.);
#15306=ORIENTED_EDGE('',*,*,#10653,.F.);
#15307=ORIENTED_EDGE('',*,*,#10380,.F.);
#15308=ORIENTED_EDGE('',*,*,#10383,.F.);
#15309=ORIENTED_EDGE('',*,*,#10387,.F.);
#15310=ORIENTED_EDGE('',*,*,#10390,.F.);
#15311=ORIENTED_EDGE('',*,*,#10393,.F.);
#15312=ORIENTED_EDGE('',*,*,#10396,.F.);
#15313=ORIENTED_EDGE('',*,*,#10399,.F.);
#15314=ORIENTED_EDGE('',*,*,#10402,.F.);
#15315=ORIENTED_EDGE('',*,*,#10405,.F.);
#15316=ORIENTED_EDGE('',*,*,#10408,.F.);
#15317=ORIENTED_EDGE('',*,*,#10411,.F.);
#15318=ORIENTED_EDGE('',*,*,#10414,.F.);
#15319=ORIENTED_EDGE('',*,*,#10417,.F.);
#15320=ORIENTED_EDGE('',*,*,#10420,.F.);
#15321=ORIENTED_EDGE('',*,*,#10423,.F.);
#15322=ORIENTED_EDGE('',*,*,#10426,.F.);
#15323=ORIENTED_EDGE('',*,*,#10429,.F.);
#15324=ORIENTED_EDGE('',*,*,#10432,.F.);
#15325=ORIENTED_EDGE('',*,*,#10435,.F.);
#15326=ORIENTED_EDGE('',*,*,#10438,.F.);
#15327=ORIENTED_EDGE('',*,*,#10441,.F.);
#15328=ORIENTED_EDGE('',*,*,#10444,.F.);
#15329=ORIENTED_EDGE('',*,*,#10447,.F.);
#15330=ORIENTED_EDGE('',*,*,#10450,.F.);
#15331=ORIENTED_EDGE('',*,*,#10453,.F.);
#15332=ORIENTED_EDGE('',*,*,#10456,.F.);
#15333=ORIENTED_EDGE('',*,*,#10459,.F.);
#15334=ORIENTED_EDGE('',*,*,#10462,.F.);
#15335=ORIENTED_EDGE('',*,*,#10465,.F.);
#15336=ORIENTED_EDGE('',*,*,#10468,.F.);
#15337=ORIENTED_EDGE('',*,*,#10471,.F.);
#15338=ORIENTED_EDGE('',*,*,#10474,.F.);
#15339=ORIENTED_EDGE('',*,*,#10477,.F.);
#15340=ORIENTED_EDGE('',*,*,#10480,.F.);
#15341=ORIENTED_EDGE('',*,*,#10483,.F.);
#15342=ORIENTED_EDGE('',*,*,#10486,.F.);
#15343=ORIENTED_EDGE('',*,*,#10489,.F.);
#15344=ORIENTED_EDGE('',*,*,#10492,.F.);
#15345=ORIENTED_EDGE('',*,*,#10495,.F.);
#15346=ORIENTED_EDGE('',*,*,#10498,.F.);
#15347=ORIENTED_EDGE('',*,*,#10501,.F.);
#15348=ORIENTED_EDGE('',*,*,#10504,.F.);
#15349=ORIENTED_EDGE('',*,*,#10507,.F.);
#15350=ORIENTED_EDGE('',*,*,#10510,.F.);
#15351=ORIENTED_EDGE('',*,*,#10513,.F.);
#15352=ORIENTED_EDGE('',*,*,#10516,.F.);
#15353=ORIENTED_EDGE('',*,*,#10519,.F.);
#15354=ORIENTED_EDGE('',*,*,#10522,.F.);
#15355=ORIENTED_EDGE('',*,*,#10525,.F.);
#15356=ORIENTED_EDGE('',*,*,#10528,.F.);
#15357=ORIENTED_EDGE('',*,*,#10531,.F.);
#15358=ORIENTED_EDGE('',*,*,#10534,.F.);
#15359=ORIENTED_EDGE('',*,*,#10537,.F.);
#15360=ORIENTED_EDGE('',*,*,#10540,.F.);
#15361=ORIENTED_EDGE('',*,*,#10543,.F.);
#15362=ORIENTED_EDGE('',*,*,#10546,.F.);
#15363=ORIENTED_EDGE('',*,*,#10549,.F.);
#15364=ORIENTED_EDGE('',*,*,#10552,.F.);
#15365=ORIENTED_EDGE('',*,*,#10555,.F.);
#15366=ORIENTED_EDGE('',*,*,#10558,.F.);
#15367=ORIENTED_EDGE('',*,*,#10561,.F.);
#15368=ORIENTED_EDGE('',*,*,#10564,.F.);
#15369=ORIENTED_EDGE('',*,*,#10567,.F.);
#15370=ORIENTED_EDGE('',*,*,#10570,.F.);
#15371=ORIENTED_EDGE('',*,*,#10573,.F.);
#15372=ORIENTED_EDGE('',*,*,#10576,.F.);
#15373=ORIENTED_EDGE('',*,*,#10579,.F.);
#15374=ORIENTED_EDGE('',*,*,#10582,.F.);
#15375=ORIENTED_EDGE('',*,*,#10585,.F.);
#15376=ORIENTED_EDGE('',*,*,#10588,.F.);
#15377=ORIENTED_EDGE('',*,*,#10591,.F.);
#15378=ORIENTED_EDGE('',*,*,#10594,.F.);
#15379=ORIENTED_EDGE('',*,*,#10597,.F.);
#15380=ORIENTED_EDGE('',*,*,#10600,.F.);
#15381=ORIENTED_EDGE('',*,*,#10603,.F.);
#15382=ORIENTED_EDGE('',*,*,#10606,.F.);
#15383=ORIENTED_EDGE('',*,*,#10609,.F.);
#15384=ORIENTED_EDGE('',*,*,#10612,.F.);
#15385=ORIENTED_EDGE('',*,*,#10615,.F.);
#15386=ORIENTED_EDGE('',*,*,#10618,.F.);
#15387=ORIENTED_EDGE('',*,*,#10621,.F.);
#15388=ORIENTED_EDGE('',*,*,#10624,.F.);
#15389=ORIENTED_EDGE('',*,*,#10627,.F.);
#15390=ORIENTED_EDGE('',*,*,#10630,.F.);
#15391=ORIENTED_EDGE('',*,*,#10633,.F.);
#15392=ORIENTED_EDGE('',*,*,#10636,.F.);
#15393=ORIENTED_EDGE('',*,*,#10639,.F.);
#15394=ORIENTED_EDGE('',*,*,#10642,.F.);
#15395=ORIENTED_EDGE('',*,*,#10652,.F.);
#15396=ORIENTED_EDGE('',*,*,#10650,.F.);
#15397=ORIENTED_EDGE('',*,*,#10115,.F.);
#15398=ORIENTED_EDGE('',*,*,#10119,.F.);
#15399=ORIENTED_EDGE('',*,*,#10122,.F.);
#15400=ORIENTED_EDGE('',*,*,#10125,.F.);
#15401=ORIENTED_EDGE('',*,*,#10128,.F.);
#15402=ORIENTED_EDGE('',*,*,#10131,.F.);
#15403=ORIENTED_EDGE('',*,*,#10134,.F.);
#15404=ORIENTED_EDGE('',*,*,#10137,.F.);
#15405=ORIENTED_EDGE('',*,*,#10140,.F.);
#15406=ORIENTED_EDGE('',*,*,#10143,.F.);
#15407=ORIENTED_EDGE('',*,*,#10146,.F.);
#15408=ORIENTED_EDGE('',*,*,#10149,.F.);
#15409=ORIENTED_EDGE('',*,*,#10152,.F.);
#15410=ORIENTED_EDGE('',*,*,#10155,.F.);
#15411=ORIENTED_EDGE('',*,*,#10158,.F.);
#15412=ORIENTED_EDGE('',*,*,#10161,.F.);
#15413=ORIENTED_EDGE('',*,*,#10164,.F.);
#15414=ORIENTED_EDGE('',*,*,#10167,.F.);
#15415=ORIENTED_EDGE('',*,*,#10170,.F.);
#15416=ORIENTED_EDGE('',*,*,#10173,.F.);
#15417=ORIENTED_EDGE('',*,*,#10176,.F.);
#15418=ORIENTED_EDGE('',*,*,#10179,.F.);
#15419=ORIENTED_EDGE('',*,*,#10182,.F.);
#15420=ORIENTED_EDGE('',*,*,#10185,.F.);
#15421=ORIENTED_EDGE('',*,*,#10188,.F.);
#15422=ORIENTED_EDGE('',*,*,#10191,.F.);
#15423=ORIENTED_EDGE('',*,*,#10194,.F.);
#15424=ORIENTED_EDGE('',*,*,#10197,.F.);
#15425=ORIENTED_EDGE('',*,*,#10200,.F.);
#15426=ORIENTED_EDGE('',*,*,#10203,.F.);
#15427=ORIENTED_EDGE('',*,*,#10206,.F.);
#15428=ORIENTED_EDGE('',*,*,#10209,.F.);
#15429=ORIENTED_EDGE('',*,*,#10212,.F.);
#15430=ORIENTED_EDGE('',*,*,#10215,.F.);
#15431=ORIENTED_EDGE('',*,*,#10218,.F.);
#15432=ORIENTED_EDGE('',*,*,#10221,.F.);
#15433=ORIENTED_EDGE('',*,*,#10224,.F.);
#15434=ORIENTED_EDGE('',*,*,#10227,.F.);
#15435=ORIENTED_EDGE('',*,*,#10230,.F.);
#15436=ORIENTED_EDGE('',*,*,#10233,.F.);
#15437=ORIENTED_EDGE('',*,*,#10236,.F.);
#15438=ORIENTED_EDGE('',*,*,#10239,.F.);
#15439=ORIENTED_EDGE('',*,*,#10242,.F.);
#15440=ORIENTED_EDGE('',*,*,#10245,.F.);
#15441=ORIENTED_EDGE('',*,*,#10248,.F.);
#15442=ORIENTED_EDGE('',*,*,#10251,.F.);
#15443=ORIENTED_EDGE('',*,*,#10254,.F.);
#15444=ORIENTED_EDGE('',*,*,#10257,.F.);
#15445=ORIENTED_EDGE('',*,*,#10260,.F.);
#15446=ORIENTED_EDGE('',*,*,#10263,.F.);
#15447=ORIENTED_EDGE('',*,*,#10266,.F.);
#15448=ORIENTED_EDGE('',*,*,#10269,.F.);
#15449=ORIENTED_EDGE('',*,*,#10272,.F.);
#15450=ORIENTED_EDGE('',*,*,#10275,.F.);
#15451=ORIENTED_EDGE('',*,*,#10278,.F.);
#15452=ORIENTED_EDGE('',*,*,#10281,.F.);
#15453=ORIENTED_EDGE('',*,*,#10284,.F.);
#15454=ORIENTED_EDGE('',*,*,#10287,.F.);
#15455=ORIENTED_EDGE('',*,*,#10290,.F.);
#15456=ORIENTED_EDGE('',*,*,#10293,.F.);
#15457=ORIENTED_EDGE('',*,*,#10296,.F.);
#15458=ORIENTED_EDGE('',*,*,#10299,.F.);
#15459=ORIENTED_EDGE('',*,*,#10302,.F.);
#15460=ORIENTED_EDGE('',*,*,#10305,.F.);
#15461=ORIENTED_EDGE('',*,*,#10308,.F.);
#15462=ORIENTED_EDGE('',*,*,#10311,.F.);
#15463=ORIENTED_EDGE('',*,*,#10314,.F.);
#15464=ORIENTED_EDGE('',*,*,#10317,.F.);
#15465=ORIENTED_EDGE('',*,*,#10320,.F.);
#15466=ORIENTED_EDGE('',*,*,#10323,.F.);
#15467=ORIENTED_EDGE('',*,*,#10326,.F.);
#15468=ORIENTED_EDGE('',*,*,#10329,.F.);
#15469=ORIENTED_EDGE('',*,*,#10332,.F.);
#15470=ORIENTED_EDGE('',*,*,#10335,.F.);
#15471=ORIENTED_EDGE('',*,*,#10338,.F.);
#15472=ORIENTED_EDGE('',*,*,#10341,.F.);
#15473=ORIENTED_EDGE('',*,*,#10344,.F.);
#15474=ORIENTED_EDGE('',*,*,#10347,.F.);
#15475=ORIENTED_EDGE('',*,*,#10350,.F.);
#15476=ORIENTED_EDGE('',*,*,#10353,.F.);
#15477=ORIENTED_EDGE('',*,*,#10356,.F.);
#15478=ORIENTED_EDGE('',*,*,#10359,.F.);
#15479=ORIENTED_EDGE('',*,*,#10362,.F.);
#15480=ORIENTED_EDGE('',*,*,#10365,.F.);
#15481=ORIENTED_EDGE('',*,*,#10368,.F.);
#15482=ORIENTED_EDGE('',*,*,#10371,.F.);
#15483=ORIENTED_EDGE('',*,*,#10374,.F.);
#15484=ORIENTED_EDGE('',*,*,#10377,.F.);
#15485=ORIENTED_EDGE('',*,*,#10654,.F.);
#15486=ORIENTED_EDGE('',*,*,#10655,.F.);
#15487=ORIENTED_EDGE('',*,*,#10656,.F.);
#15488=ORIENTED_EDGE('',*,*,#10657,.F.);
#15489=ORIENTED_EDGE('',*,*,#10658,.F.);
#15490=ORIENTED_EDGE('',*,*,#10659,.F.);
#15491=ORIENTED_EDGE('',*,*,#10660,.T.);
#15492=ORIENTED_EDGE('',*,*,#10661,.F.);
#15493=ORIENTED_EDGE('',*,*,#10660,.F.);
#15494=ORIENTED_EDGE('',*,*,#10662,.F.);
#15495=ORIENTED_EDGE('',*,*,#10663,.F.);
#15496=ORIENTED_EDGE('',*,*,#10658,.T.);
#15497=ORIENTED_EDGE('',*,*,#10664,.F.);
#15498=ORIENTED_EDGE('',*,*,#10665,.T.);
#15499=ORIENTED_EDGE('',*,*,#10666,.T.);
#15500=ORIENTED_EDGE('',*,*,#10657,.T.);
#15501=ORIENTED_EDGE('',*,*,#10667,.F.);
#15502=ORIENTED_EDGE('',*,*,#10668,.T.);
#15503=ORIENTED_EDGE('',*,*,#10664,.T.);
#15504=ORIENTED_EDGE('',*,*,#10656,.T.);
#15505=ORIENTED_EDGE('',*,*,#10669,.F.);
#15506=ORIENTED_EDGE('',*,*,#10670,.T.);
#15507=ORIENTED_EDGE('',*,*,#10667,.T.);
#15508=ORIENTED_EDGE('',*,*,#10670,.F.);
#15509=ORIENTED_EDGE('',*,*,#10671,.F.);
#15510=ORIENTED_EDGE('',*,*,#10672,.F.);
#15511=ORIENTED_EDGE('',*,*,#10673,.F.);
#15512=ORIENTED_EDGE('',*,*,#10665,.F.);
#15513=ORIENTED_EDGE('',*,*,#10668,.F.);
#15514=ORIENTED_EDGE('',*,*,#10674,.T.);
#15515=ORIENTED_EDGE('',*,*,#10644,.T.);
#15516=ORIENTED_EDGE('',*,*,#10384,.T.);
#15517=ORIENTED_EDGE('',*,*,#10381,.T.);
#15518=ORIENTED_EDGE('',*,*,#10653,.T.);
#15519=ORIENTED_EDGE('',*,*,#10655,.T.);
#15520=ORIENTED_EDGE('',*,*,#10675,.F.);
#15521=ORIENTED_EDGE('',*,*,#10671,.T.);
#15522=ORIENTED_EDGE('',*,*,#10669,.T.);
#15523=ORIENTED_EDGE('',*,*,#10663,.T.);
#15524=ORIENTED_EDGE('',*,*,#10676,.F.);
#15525=ORIENTED_EDGE('',*,*,#10672,.T.);
#15526=ORIENTED_EDGE('',*,*,#10675,.T.);
#15527=ORIENTED_EDGE('',*,*,#10662,.T.);
#15528=ORIENTED_EDGE('',*,*,#10659,.T.);
#15529=ORIENTED_EDGE('',*,*,#10666,.F.);
#15530=ORIENTED_EDGE('',*,*,#10673,.T.);
#15531=ORIENTED_EDGE('',*,*,#10676,.T.);
#15532=ORIENTED_EDGE('',*,*,#10661,.T.);
#15533=ORIENTED_EDGE('',*,*,#10677,.F.);
#15534=ORIENTED_EDGE('',*,*,#10648,.F.);
#15535=ORIENTED_EDGE('',*,*,#10116,.F.);
#15536=ORIENTED_EDGE('',*,*,#10649,.F.);
#15537=ORIENTED_EDGE('',*,*,#10678,.T.);
#15538=ORIENTED_EDGE('',*,*,#10677,.T.);
#15539=ORIENTED_EDGE('',*,*,#10678,.F.);
#15540=ORIENTED_EDGE('',*,*,#10376,.T.);
#15541=ORIENTED_EDGE('',*,*,#10645,.T.);
#15542=ORIENTED_EDGE('',*,*,#10674,.F.);
#15543=ORIENTED_EDGE('',*,*,#10654,.T.);
#15544=ORIENTED_EDGE('',*,*,#10679,.T.);
#15545=ORIENTED_EDGE('',*,*,#10680,.T.);
#15546=ORIENTED_EDGE('',*,*,#10681,.T.);
#15547=ORIENTED_EDGE('',*,*,#10682,.T.);
#15548=ORIENTED_EDGE('',*,*,#10683,.T.);
#15549=ORIENTED_EDGE('',*,*,#10684,.T.);
#15550=ORIENTED_EDGE('',*,*,#10685,.T.);
#15551=ORIENTED_EDGE('',*,*,#10686,.T.);
#15552=ORIENTED_EDGE('',*,*,#10687,.T.);
#15553=ORIENTED_EDGE('',*,*,#10688,.T.);
#15554=ORIENTED_EDGE('',*,*,#10689,.T.);
#15555=ORIENTED_EDGE('',*,*,#10690,.T.);
#15556=ORIENTED_EDGE('',*,*,#10691,.T.);
#15557=ORIENTED_EDGE('',*,*,#10692,.T.);
#15558=ORIENTED_EDGE('',*,*,#10693,.T.);
#15559=ORIENTED_EDGE('',*,*,#10680,.F.);
#15560=ORIENTED_EDGE('',*,*,#10689,.F.);
#15561=ORIENTED_EDGE('',*,*,#10694,.T.);
#15562=ORIENTED_EDGE('',*,*,#10695,.T.);
#15563=ORIENTED_EDGE('',*,*,#10696,.T.);
#15564=ORIENTED_EDGE('',*,*,#10697,.T.);
#15565=ORIENTED_EDGE('',*,*,#10698,.T.);
#15566=ORIENTED_EDGE('',*,*,#10687,.F.);
#15567=ORIENTED_EDGE('',*,*,#10699,.T.);
#15568=ORIENTED_EDGE('',*,*,#10700,.T.);
#15569=ORIENTED_EDGE('',*,*,#10701,.T.);
#15570=ORIENTED_EDGE('',*,*,#10702,.T.);
#15571=ORIENTED_EDGE('',*,*,#10703,.T.);
#15572=ORIENTED_EDGE('',*,*,#10688,.F.);
#15573=ORIENTED_EDGE('',*,*,#10703,.F.);
#15574=ORIENTED_EDGE('',*,*,#10694,.F.);
#15575=ORIENTED_EDGE('',*,*,#10686,.F.);
#15576=ORIENTED_EDGE('',*,*,#10704,.F.);
#15577=ORIENTED_EDGE('',*,*,#10699,.F.);
#15578=ORIENTED_EDGE('',*,*,#10684,.F.);
#15579=ORIENTED_EDGE('',*,*,#10705,.F.);
#15580=ORIENTED_EDGE('',*,*,#10706,.F.);
#15581=ORIENTED_EDGE('',*,*,#10682,.F.);
#15582=ORIENTED_EDGE('',*,*,#10707,.F.);
#15583=ORIENTED_EDGE('',*,*,#10708,.F.);
#15584=ORIENTED_EDGE('',*,*,#10692,.F.);
#15585=ORIENTED_EDGE('',*,*,#10709,.F.);
#15586=ORIENTED_EDGE('',*,*,#10710,.F.);
#15587=ORIENTED_EDGE('',*,*,#10690,.F.);
#15588=ORIENTED_EDGE('',*,*,#10698,.F.);
#15589=ORIENTED_EDGE('',*,*,#10711,.F.);
#15590=ORIENTED_EDGE('',*,*,#10685,.F.);
#15591=ORIENTED_EDGE('',*,*,#10706,.T.);
#15592=ORIENTED_EDGE('',*,*,#10712,.T.);
#15593=ORIENTED_EDGE('',*,*,#10713,.T.);
#15594=ORIENTED_EDGE('',*,*,#10714,.T.);
#15595=ORIENTED_EDGE('',*,*,#10704,.T.);
#15596=ORIENTED_EDGE('',*,*,#10679,.F.);
#15597=ORIENTED_EDGE('',*,*,#10715,.T.);
#15598=ORIENTED_EDGE('',*,*,#10716,.F.);
#15599=ORIENTED_EDGE('',*,*,#10700,.F.);
#15600=ORIENTED_EDGE('',*,*,#10714,.F.);
#15601=ORIENTED_EDGE('',*,*,#10712,.F.);
#15602=ORIENTED_EDGE('',*,*,#10717,.F.);
#15603=ORIENTED_EDGE('',*,*,#10718,.F.);
#15604=ORIENTED_EDGE('',*,*,#10719,.F.);
#15605=ORIENTED_EDGE('',*,*,#10695,.F.);
#15606=ORIENTED_EDGE('',*,*,#10702,.F.);
#15607=ORIENTED_EDGE('',*,*,#10720,.F.);
#15608=ORIENTED_EDGE('',*,*,#10721,.F.);
#15609=ORIENTED_EDGE('',*,*,#10722,.F.);
#15610=ORIENTED_EDGE('',*,*,#10723,.F.);
#15611=ORIENTED_EDGE('',*,*,#10724,.F.);
#15612=ORIENTED_EDGE('',*,*,#10697,.F.);
#15613=ORIENTED_EDGE('',*,*,#10725,.F.);
#15614=ORIENTED_EDGE('',*,*,#10726,.F.);
#15615=ORIENTED_EDGE('',*,*,#10727,.F.);
#15616=ORIENTED_EDGE('',*,*,#10691,.F.);
#15617=ORIENTED_EDGE('',*,*,#10711,.T.);
#15618=ORIENTED_EDGE('',*,*,#10724,.T.);
#15619=ORIENTED_EDGE('',*,*,#10728,.T.);
#15620=ORIENTED_EDGE('',*,*,#10726,.T.);
#15621=ORIENTED_EDGE('',*,*,#10709,.T.);
#15622=ORIENTED_EDGE('',*,*,#10729,.T.);
#15623=ORIENTED_EDGE('',*,*,#10730,.T.);
#15624=ORIENTED_EDGE('',*,*,#10727,.T.);
#15625=ORIENTED_EDGE('',*,*,#10731,.T.);
#15626=ORIENTED_EDGE('',*,*,#10693,.F.);
#15627=ORIENTED_EDGE('',*,*,#10710,.T.);
#15628=ORIENTED_EDGE('',*,*,#10725,.T.);
#15629=ORIENTED_EDGE('',*,*,#10732,.T.);
#15630=ORIENTED_EDGE('',*,*,#10721,.T.);
#15631=ORIENTED_EDGE('',*,*,#10707,.T.);
#15632=ORIENTED_EDGE('',*,*,#10681,.F.);
#15633=ORIENTED_EDGE('',*,*,#10733,.T.);
#15634=ORIENTED_EDGE('',*,*,#10734,.T.);
#15635=ORIENTED_EDGE('',*,*,#10723,.T.);
#15636=ORIENTED_EDGE('',*,*,#10735,.T.);
#15637=ORIENTED_EDGE('',*,*,#10736,.T.);
#15638=ORIENTED_EDGE('',*,*,#10737,.T.);
#15639=ORIENTED_EDGE('',*,*,#10722,.T.);
#15640=ORIENTED_EDGE('',*,*,#10738,.T.);
#15641=ORIENTED_EDGE('',*,*,#10683,.F.);
#15642=ORIENTED_EDGE('',*,*,#10708,.T.);
#15643=ORIENTED_EDGE('',*,*,#10720,.T.);
#15644=ORIENTED_EDGE('',*,*,#10739,.T.);
#15645=ORIENTED_EDGE('',*,*,#10717,.T.);
#15646=ORIENTED_EDGE('',*,*,#10705,.T.);
#15647=ORIENTED_EDGE('',*,*,#10740,.T.);
#15648=ORIENTED_EDGE('',*,*,#10741,.T.);
#15649=ORIENTED_EDGE('',*,*,#10719,.T.);
#15650=ORIENTED_EDGE('',*,*,#10742,.T.);
#15651=ORIENTED_EDGE('',*,*,#10743,.T.);
#15652=ORIENTED_EDGE('',*,*,#10744,.T.);
#15653=ORIENTED_EDGE('',*,*,#10718,.T.);
#15654=ORIENTED_EDGE('',*,*,#10745,.T.);
#15655=ORIENTED_EDGE('',*,*,#10746,.T.);
#15656=ORIENTED_EDGE('',*,*,#10747,.T.);
#15657=ORIENTED_EDGE('',*,*,#10716,.T.);
#15658=ORIENTED_EDGE('',*,*,#10748,.T.);
#15659=ORIENTED_EDGE('',*,*,#10735,.F.);
#15660=ORIENTED_EDGE('',*,*,#10696,.F.);
#15661=ORIENTED_EDGE('',*,*,#10741,.F.);
#15662=ORIENTED_EDGE('',*,*,#10749,.T.);
#15663=ORIENTED_EDGE('',*,*,#10742,.F.);
#15664=ORIENTED_EDGE('',*,*,#10701,.F.);
#15665=ORIENTED_EDGE('',*,*,#10747,.F.);
#15666=ORIENTED_EDGE('',*,*,#10750,.T.);
#15667=ORIENTED_EDGE('',*,*,#10748,.F.);
#15668=ORIENTED_EDGE('',*,*,#10713,.F.);
#15669=ORIENTED_EDGE('',*,*,#10744,.F.);
#15670=ORIENTED_EDGE('',*,*,#10751,.T.);
#15671=ORIENTED_EDGE('',*,*,#10752,.F.);
#15672=ORIENTED_EDGE('',*,*,#10753,.T.);
#15673=ORIENTED_EDGE('',*,*,#10754,.F.);
#15674=ORIENTED_EDGE('',*,*,#10729,.F.);
#15675=ORIENTED_EDGE('',*,*,#10755,.F.);
#15676=ORIENTED_EDGE('',*,*,#10733,.F.);
#15677=ORIENTED_EDGE('',*,*,#10749,.F.);
#15678=ORIENTED_EDGE('',*,*,#10740,.F.);
#15679=ORIENTED_EDGE('',*,*,#10750,.F.);
#15680=ORIENTED_EDGE('',*,*,#10746,.F.);
#15681=ORIENTED_EDGE('',*,*,#10751,.F.);
#15682=ORIENTED_EDGE('',*,*,#10743,.F.);
#15683=ORIENTED_EDGE('',*,*,#10756,.F.);
#15684=ORIENTED_EDGE('',*,*,#10736,.F.);
#15685=ORIENTED_EDGE('',*,*,#10757,.F.);
#15686=ORIENTED_EDGE('',*,*,#10753,.F.);
#15687=ORIENTED_EDGE('',*,*,#10758,.F.);
#15688=ORIENTED_EDGE('',*,*,#10759,.T.);
#15689=ORIENTED_EDGE('',*,*,#10760,.T.);
#15690=ORIENTED_EDGE('',*,*,#10759,.F.);
#15691=ORIENTED_EDGE('',*,*,#10760,.F.);
#15692=ORIENTED_EDGE('',*,*,#10761,.T.);
#15693=ORIENTED_EDGE('',*,*,#10762,.T.);
#15694=ORIENTED_EDGE('',*,*,#10761,.F.);
#15695=ORIENTED_EDGE('',*,*,#10762,.F.);
#15696=ORIENTED_EDGE('',*,*,#10763,.T.);
#15697=ORIENTED_EDGE('',*,*,#10715,.F.);
#15698=ORIENTED_EDGE('',*,*,#10763,.F.);
#15699=ORIENTED_EDGE('',*,*,#10737,.F.);
#15700=ORIENTED_EDGE('',*,*,#10756,.T.);
#15701=ORIENTED_EDGE('',*,*,#10745,.F.);
#15702=ORIENTED_EDGE('',*,*,#10739,.F.);
#15703=ORIENTED_EDGE('',*,*,#10730,.F.);
#15704=ORIENTED_EDGE('',*,*,#10754,.T.);
#15705=ORIENTED_EDGE('',*,*,#10757,.T.);
#15706=ORIENTED_EDGE('',*,*,#10738,.F.);
#15707=ORIENTED_EDGE('',*,*,#10732,.F.);
#15708=ORIENTED_EDGE('',*,*,#10734,.F.);
#15709=ORIENTED_EDGE('',*,*,#10755,.T.);
#15710=ORIENTED_EDGE('',*,*,#10731,.F.);
#15711=ORIENTED_EDGE('',*,*,#10728,.F.);
#15712=ORIENTED_EDGE('',*,*,#10752,.T.);
#15713=ORIENTED_EDGE('',*,*,#10758,.T.);
#15714=PLANE('',#17192);
#15715=PLANE('',#17193);
#15716=PLANE('',#17194);
#15717=PLANE('',#17200);
#15718=PLANE('',#17201);
#15719=PLANE('',#17202);
#15720=PLANE('',#17210);
#15721=PLANE('',#17221);
#15722=PLANE('',#17253);
#15723=PLANE('',#17257);
#15724=PLANE('',#17272);
#15725=PLANE('',#17280);
#15726=PLANE('',#17299);
#15727=PLANE('',#17300);
#15728=PLANE('',#17325);
#15729=PLANE('',#17337);
#15730=PLANE('',#17348);
#15731=PLANE('',#17365);
#15732=PLANE('',#17368);
#15733=PLANE('',#17393);
#15734=PLANE('',#17406);
#15735=PLANE('',#17409);
#15736=PLANE('',#17413);
#15737=PLANE('',#17417);
#15738=PLANE('',#17421);
#15739=PLANE('',#17425);
#15740=PLANE('',#17429);
#15741=PLANE('',#17433);
#15742=PLANE('',#17437);
#15743=PLANE('',#17438);
#15744=PLANE('',#17439);
#15745=PLANE('',#17440);
#15746=PLANE('',#17441);
#15747=PLANE('',#17442);
#15748=PLANE('',#17443);
#15749=PLANE('',#17444);
#15750=PLANE('',#17445);
#15751=PLANE('',#17446);
#15752=PLANE('',#17447);
#15753=PLANE('',#17457);
#15754=PLANE('',#17461);
#15755=PLANE('',#17462);
#15756=PLANE('',#17467);
#15757=PLANE('',#17469);
#15758=PLANE('',#17472);
#15759=PLANE('',#17474);
#15760=PLANE('',#17475);
#15761=PLANE('',#17480);
#15762=PLANE('',#17482);
#15763=PLANE('',#17491);
#15764=PLANE('',#17502);
#15765=PLANE('',#17512);
#15766=PLANE('',#17525);
#15767=PLANE('',#17532);
#15768=PLANE('',#17542);
#15769=PLANE('',#17551);
#15770=PLANE('',#17564);
#15771=PLANE('',#17581);
#15772=PLANE('',#17587);
#15773=PLANE('',#17610);
#15774=PLANE('',#17614);
#15775=PLANE('',#17637);
#15776=PLANE('',#17641);
#15777=PLANE('',#17645);
#15778=PLANE('',#17649);
#15779=PLANE('',#17655);
#15780=PLANE('',#17663);
#15781=PLANE('',#17669);
#15782=PLANE('',#17680);
#15783=PLANE('',#17749);
#15784=PLANE('',#17756);
#15785=PLANE('',#17761);
#15786=PLANE('',#17766);
#15787=PLANE('',#17770);
#15788=PLANE('',#17773);
#15789=PLANE('',#17789);
#15790=PLANE('',#17791);
#15791=PLANE('',#17792);
#15792=PLANE('',#17793);
#15793=PLANE('',#17794);
#15794=PLANE('',#17795);
#15795=PLANE('',#17796);
#15796=PLANE('',#17797);
#15797=PLANE('',#17798);
#15798=PLANE('',#17799);
#15799=PLANE('',#17800);
#15800=PLANE('',#17801);
#15801=PLANE('',#17802);
#15802=PLANE('',#17803);
#15803=PLANE('',#17804);
#15804=PLANE('',#17805);
#15805=PLANE('',#17814);
#15806=PLANE('',#17815);
#15807=PLANE('',#17816);
#15808=PLANE('',#17817);
#15809=PLANE('',#17823);
#15810=PLANE('',#17834);
#15811=PLANE('',#17847);
#15812=PLANE('',#17856);
#15813=PLANE('',#17861);
#15814=PLANE('',#17889);
#15815=PLANE('',#17892);
#15816=PLANE('',#17894);
#15817=PLANE('',#17921);
#15818=PLANE('',#17923);
#15819=PLANE('',#17952);
#15820=PLANE('',#17955);
#15821=PLANE('',#17957);
#15822=PLANE('',#17984);
#15823=PLANE('',#17986);
#15824=PLANE('',#18002);
#15825=PLANE('',#18003);
#15826=PLANE('',#18006);
#15827=PLANE('',#18033);
#15828=PLANE('',#18043);
#15829=PLANE('',#18044);
#15830=PLANE('',#18045);
#15831=PLANE('',#18046);
#15832=PLANE('',#18047);
#15833=PLANE('',#18048);
#15834=PLANE('',#18049);
#15835=PLANE('',#18050);
#15836=PLANE('',#18051);
#15837=PLANE('',#18052);
#15838=PLANE('',#18053);
#15839=PLANE('',#18059);
#15840=PLANE('',#18060);
#15841=PLANE('',#18061);
#15842=PLANE('',#18062);
#15843=PLANE('',#18065);
#15844=PLANE('',#18067);
#15845=PLANE('',#18073);
#15846=PLANE('',#18076);
#15847=PLANE('',#18079);
#15848=PLANE('',#18082);
#15849=PLANE('',#18085);
#15850=PLANE('',#18090);
#15851=PLANE('',#18091);
#15852=PLANE('',#18095);
#15853=PLANE('',#18097);
#15854=PLANE('',#18099);
#15855=PLANE('',#18101);
#15856=PLANE('',#18104);
#15857=PLANE('',#18106);
#15858=PLANE('',#18118);
#15859=PLANE('',#18119);
#15860=PLANE('',#18120);
#15861=PLANE('',#18121);
#15862=PLANE('',#18122);
#15863=PLANE('',#18123);
#15864=PLANE('',#18124);
#15865=PLANE('',#18126);
#15866=PLANE('',#18127);
#15867=PLANE('',#18128);
#15868=PLANE('',#18129);
#15869=PLANE('',#18130);
#15870=PLANE('',#18131);
#15871=PLANE('',#18132);
#15872=PLANE('',#18138);
#15873=PLANE('',#18139);
#15874=PLANE('',#18140);
#15875=PLANE('',#18141);
#15876=PLANE('',#18142);
#15877=PLANE('',#18143);
#15878=PLANE('',#18144);
#15879=PLANE('',#18145);
#15880=PLANE('',#18146);
#15881=PLANE('',#18147);
#15882=PLANE('',#18148);
#15883=PLANE('',#18149);
#15884=PLANE('',#18150);
#15885=PLANE('',#18151);
#15886=PLANE('',#18152);
#15887=PLANE('',#18153);
#15888=PLANE('',#18154);
#15889=PLANE('',#18155);
#15890=PLANE('',#18156);
#15891=PLANE('',#18157);
#15892=PLANE('',#18158);
#15893=PLANE('',#18159);
#15894=PLANE('',#18173);
#15895=PLANE('',#18180);
#15896=PLANE('',#18181);
#15897=PLANE('',#18183);
#15898=PLANE('',#18189);
#15899=PLANE('',#18191);
#15900=PLANE('',#18194);
#15901=PLANE('',#18195);
#15902=PLANE('',#18196);
#15903=PLANE('',#18201);
#15904=PLANE('',#18209);
#15905=PLANE('',#18217);
#15906=PLANE('',#18222);
#15907=PLANE('',#18234);
#15908=PLANE('',#18238);
#15909=PLANE('',#18242);
#15910=PLANE('',#18246);
#15911=PLANE('',#18250);
#15912=PLANE('',#18254);
#15913=PLANE('',#18258);
#15914=PLANE('',#18262);
#15915=PLANE('',#18268);
#15916=PLANE('',#18271);
#15917=PLANE('',#18274);
#15918=PLANE('',#18277);
#15919=PLANE('',#18284);
#15920=PLANE('',#18285);
#15921=PLANE('',#18289);
#15922=PLANE('',#18293);
#15923=PLANE('',#18297);
#15924=PLANE('',#18301);
#15925=PLANE('',#18304);
#15926=PLANE('',#18307);
#15927=PLANE('',#18310);
#15928=PLANE('',#18314);
#15929=PLANE('',#18316);
#15930=PLANE('',#18318);
#15931=PLANE('',#18320);
#15932=PLANE('',#18362);
#15933=PLANE('',#18363);
#15934=PLANE('',#18371);
#15935=PLANE('',#18374);
#15936=PLANE('',#18467);
#15937=PLANE('',#18474);
#15938=PLANE('',#18475);
#15939=PLANE('',#18476);
#15940=PLANE('',#18477);
#15941=PLANE('',#18479);
#15942=PLANE('',#18480);
#15943=PLANE('',#18481);
#15944=PLANE('',#18482);
#15945=PLANE('',#18483);
#15946=PLANE('',#18667);
#15947=PLANE('',#18674);
#15948=PLANE('',#18675);
#15949=PLANE('',#18676);
#15950=PLANE('',#18677);
#15951=PLANE('',#18679);
#15952=PLANE('',#18680);
#15953=PLANE('',#18681);
#15954=PLANE('',#18682);
#15955=PLANE('',#18683);
#15956=PLANE('',#18702);
#15957=PLANE('',#18704);
#15958=PLANE('',#18705);
#15959=PLANE('',#18706);
#15960=PLANE('',#18707);
#15961=PLANE('',#18708);
#15962=PLANE('',#18709);
#15963=PLANE('',#18710);
#15964=PLANE('',#18711);
#15965=PLANE('',#18712);
#15966=PLANE('',#18713);
#15967=PLANE('',#18714);
#15968=PLANE('',#18715);
#15969=PLANE('',#18716);
#15970=PLANE('',#18717);
#15971=PLANE('',#18718);
#15972=PLANE('',#18727);
#15973=PLANE('',#18728);
#15974=PLANE('',#18729);
#15975=PLANE('',#18730);
#15976=ADVANCED_FACE('',(#1805),#15714,.T.);
#15977=ADVANCED_FACE('',(#1806),#15715,.T.);
#15978=ADVANCED_FACE('',(#1807),#15716,.T.);
#15979=ADVANCED_FACE('',(#1808),#1226,.F.);
#15980=ADVANCED_FACE('',(#1809),#15717,.T.);
#15981=ADVANCED_FACE('',(#1810),#15718,.T.);
#15982=ADVANCED_FACE('',(#1811),#15719,.T.);
#15983=ADVANCED_FACE('',(#1812),#1227,.F.);
#15984=ADVANCED_FACE('',(#1813),#564,.F.);
#15985=ADVANCED_FACE('',(#1814,#414,#415,#416),#15720,.F.);
#15986=ADVANCED_FACE('',(#1815),#565,.F.);
#15987=ADVANCED_FACE('',(#1816),#566,.F.);
#15988=ADVANCED_FACE('',(#1817,#417,#418,#419),#15721,.T.);
#15989=ADVANCED_FACE('',(#1818),#1228,.F.);
#15990=ADVANCED_FACE('',(#1819),#567,.F.);
#15991=ADVANCED_FACE('',(#1820),#1229,.F.);
#15992=ADVANCED_FACE('',(#1821),#367,.T.);
#15993=ADVANCED_FACE('',(#1822),#568,.T.);
#15994=ADVANCED_FACE('',(#1823),#368,.T.);
#15995=ADVANCED_FACE('',(#1824),#569,.T.);
#15996=ADVANCED_FACE('',(#1825),#369,.T.);
#15997=ADVANCED_FACE('',(#1826),#570,.T.);
#15998=ADVANCED_FACE('',(#1827,#420,#421,#422,#423,#424,#425),#15722,.T.);
#15999=ADVANCED_FACE('',(#1828),#370,.T.);
#16000=ADVANCED_FACE('',(#1829,#426,#427,#428),#15723,.T.);
#16001=ADVANCED_FACE('',(#1830),#371,.T.);
#16002=ADVANCED_FACE('',(#1831),#1230,.T.);
#16003=ADVANCED_FACE('',(#1832),#372,.T.);
#16004=ADVANCED_FACE('',(#1833,#429,#430,#431),#15724,.T.);
#16005=ADVANCED_FACE('',(#1834),#373,.T.);
#16006=ADVANCED_FACE('',(#1835),#374,.T.);
#16007=ADVANCED_FACE('',(#1836,#432,#433,#434,#435,#436,#437,#438),#15725,
 .T.);
#16008=ADVANCED_FACE('',(#1837),#375,.T.);
#16009=ADVANCED_FACE('',(#1838),#1231,.T.);
#16010=ADVANCED_FACE('',(#1839),#376,.T.);
#16011=ADVANCED_FACE('',(#1840),#1232,.T.);
#16012=ADVANCED_FACE('',(#1841),#15726,.T.);
#16013=ADVANCED_FACE('',(#1842),#15727,.F.);
#16014=ADVANCED_FACE('',(#1843),#1233,.T.);
#16015=ADVANCED_FACE('',(#1844),#377,.T.);
#16016=ADVANCED_FACE('',(#1845),#1234,.T.);
#16017=ADVANCED_FACE('',(#1846),#378,.T.);
#16018=ADVANCED_FACE('',(#1847),#1235,.T.);
#16019=ADVANCED_FACE('',(#1848),#379,.T.);
#16020=ADVANCED_FACE('',(#1849),#1236,.T.);
#16021=ADVANCED_FACE('',(#1850),#380,.T.);
#16022=ADVANCED_FACE('',(#1851),#1237,.T.);
#16023=ADVANCED_FACE('',(#1852),#15728,.T.);
#16024=ADVANCED_FACE('',(#1853),#1238,.T.);
#16025=ADVANCED_FACE('',(#1854),#1239,.T.);
#16026=ADVANCED_FACE('',(#1855),#1240,.T.);
#16027=ADVANCED_FACE('',(#1856),#381,.T.);
#16028=ADVANCED_FACE('',(#1857),#382,.T.);
#16029=ADVANCED_FACE('',(#1858),#15729,.F.);
#16030=ADVANCED_FACE('',(#1859),#383,.T.);
#16031=ADVANCED_FACE('',(#1860),#571,.F.);
#16032=ADVANCED_FACE('',(#1861),#337,.F.);
#16033=ADVANCED_FACE('',(#1862),#1241,.T.);
#16034=ADVANCED_FACE('',(#1863),#1242,.T.);
#16035=ADVANCED_FACE('',(#1864),#338,.F.);
#16036=ADVANCED_FACE('',(#1865),#15730,.F.);
#16037=ADVANCED_FACE('',(#1866),#1243,.F.);
#16038=ADVANCED_FACE('',(#1867),#384,.T.);
#16039=ADVANCED_FACE('',(#1868),#1244,.T.);
#16040=ADVANCED_FACE('',(#1869),#385,.T.);
#16041=ADVANCED_FACE('',(#1870),#1245,.T.);
#16042=ADVANCED_FACE('',(#1871),#15731,.T.);
#16043=ADVANCED_FACE('',(#1872),#1246,.T.);
#16044=ADVANCED_FACE('',(#1873),#15732,.T.);
#16045=ADVANCED_FACE('',(#1874),#386,.T.);
#16046=ADVANCED_FACE('',(#1875),#387,.T.);
#16047=ADVANCED_FACE('',(#1876),#1247,.T.);
#16048=ADVANCED_FACE('',(#1877),#388,.T.);
#16049=ADVANCED_FACE('',(#1878),#1248,.T.);
#16050=ADVANCED_FACE('',(#1879),#389,.T.);
#16051=ADVANCED_FACE('',(#1880),#1249,.T.);
#16052=ADVANCED_FACE('',(#1881),#390,.T.);
#16053=ADVANCED_FACE('',(#1882),#1250,.T.);
#16054=ADVANCED_FACE('',(#1883),#1251,.T.);
#16055=ADVANCED_FACE('',(#1884),#15733,.T.);
#16056=ADVANCED_FACE('',(#1885),#1252,.T.);
#16057=ADVANCED_FACE('',(#1886),#1253,.T.);
#16058=ADVANCED_FACE('',(#1887),#391,.T.);
#16059=ADVANCED_FACE('',(#1888),#1254,.T.);
#16060=ADVANCED_FACE('',(#1889),#392,.T.);
#16061=ADVANCED_FACE('',(#1890),#15734,.T.);
#16062=ADVANCED_FACE('',(#1891),#15735,.T.);
#16063=ADVANCED_FACE('',(#1892),#393,.T.);
#16064=ADVANCED_FACE('',(#1893),#15736,.T.);
#16065=ADVANCED_FACE('',(#1894),#1255,.T.);
#16066=ADVANCED_FACE('',(#1895),#15737,.T.);
#16067=ADVANCED_FACE('',(#1896),#1256,.T.);
#16068=ADVANCED_FACE('',(#1897),#15738,.T.);
#16069=ADVANCED_FACE('',(#1898),#1257,.T.);
#16070=ADVANCED_FACE('',(#1899),#15739,.T.);
#16071=ADVANCED_FACE('',(#1900),#1258,.T.);
#16072=ADVANCED_FACE('',(#1901),#15740,.T.);
#16073=ADVANCED_FACE('',(#1902),#1259,.T.);
#16074=ADVANCED_FACE('',(#1903),#15741,.T.);
#16075=ADVANCED_FACE('',(#1904),#1260,.T.);
#16076=ADVANCED_FACE('',(#1905),#15742,.T.);
#16077=ADVANCED_FACE('',(#1906),#15743,.T.);
#16078=ADVANCED_FACE('',(#1907),#15744,.T.);
#16079=ADVANCED_FACE('',(#1908),#15745,.T.);
#16080=ADVANCED_FACE('',(#1909),#15746,.T.);
#16081=ADVANCED_FACE('',(#1910),#15747,.T.);
#16082=ADVANCED_FACE('',(#1911),#15748,.T.);
#16083=ADVANCED_FACE('',(#1912),#15749,.T.);
#16084=ADVANCED_FACE('',(#1913),#15750,.F.);
#16085=ADVANCED_FACE('',(#1914),#15751,.F.);
#16086=ADVANCED_FACE('',(#1915),#15752,.T.);
#16087=ADVANCED_FACE('',(#1916),#1261,.F.);
#16088=ADVANCED_FACE('',(#1917),#1262,.F.);
#16089=ADVANCED_FACE('',(#1918),#1263,.F.);
#16090=ADVANCED_FACE('',(#1919),#1264,.F.);
#16091=ADVANCED_FACE('',(#1920),#1265,.F.);
#16092=ADVANCED_FACE('',(#1921),#1266,.F.);
#16093=ADVANCED_FACE('',(#1922),#1267,.F.);
#16094=ADVANCED_FACE('',(#1923,#439),#15753,.F.);
#16095=ADVANCED_FACE('',(#1924),#1268,.F.);
#16096=ADVANCED_FACE('',(#1925,#440),#15754,.F.);
#16097=ADVANCED_FACE('',(#1926,#441),#15755,.F.);
#16098=ADVANCED_FACE('',(#1927),#1269,.F.);
#16099=ADVANCED_FACE('',(#1928),#572,.F.);
#16100=ADVANCED_FACE('',(#1929),#15756,.F.);
#16101=ADVANCED_FACE('',(#1930),#1270,.T.);
#16102=ADVANCED_FACE('',(#1931),#15757,.T.);
#16103=ADVANCED_FACE('',(#1932),#1271,.T.);
#16104=ADVANCED_FACE('',(#1933),#1272,.T.);
#16105=ADVANCED_FACE('',(#1934),#15758,.T.);
#16106=ADVANCED_FACE('',(#1935),#1273,.T.);
#16107=ADVANCED_FACE('',(#1936),#15759,.T.);
#16108=ADVANCED_FACE('',(#1937),#15760,.T.);
#16109=ADVANCED_FACE('',(#1938),#1274,.T.);
#16110=ADVANCED_FACE('',(#1939),#1275,.T.);
#16111=ADVANCED_FACE('',(#1940),#1276,.T.);
#16112=ADVANCED_FACE('',(#1941),#1277,.T.);
#16113=ADVANCED_FACE('',(#1942),#15761,.T.);
#16114=ADVANCED_FACE('',(#1943),#1278,.T.);
#16115=ADVANCED_FACE('',(#1944),#15762,.T.);
#16116=ADVANCED_FACE('',(#1945),#1279,.T.);
#16117=ADVANCED_FACE('',(#1946),#1280,.T.);
#16118=ADVANCED_FACE('',(#1947),#573,.T.);
#16119=ADVANCED_FACE('',(#1948),#574,.T.);
#16120=ADVANCED_FACE('',(#1949,#442),#15763,.F.);
#16121=ADVANCED_FACE('',(#1950),#575,.T.);
#16122=ADVANCED_FACE('',(#1951),#1281,.T.);
#16123=ADVANCED_FACE('',(#1952),#576,.T.);
#16124=ADVANCED_FACE('',(#1953,#443),#1282,.T.);
#16125=ADVANCED_FACE('',(#1954,#444,#445,#446,#447,#448,#449,#450),#15764,
 .T.);
#16126=ADVANCED_FACE('',(#1955),#1283,.F.);
#16127=ADVANCED_FACE('',(#1956),#15765,.F.);
#16128=ADVANCED_FACE('',(#1957),#1284,.F.);
#16129=ADVANCED_FACE('',(#1958),#1285,.F.);
#16130=ADVANCED_FACE('',(#1959),#1286,.F.);
#16131=ADVANCED_FACE('',(#1960),#1287,.F.);
#16132=ADVANCED_FACE('',(#1961),#1288,.F.);
#16133=ADVANCED_FACE('',(#1962),#1289,.F.);
#16134=ADVANCED_FACE('',(#1963,#451),#15766,.T.);
#16135=ADVANCED_FACE('',(#1964),#577,.F.);
#16136=ADVANCED_FACE('',(#1965),#578,.F.);
#16137=ADVANCED_FACE('',(#1966,#452,#453,#454,#455,#456,#457,#458),#15767,
 .T.);
#16138=ADVANCED_FACE('',(#1967),#579,.T.);
#16139=ADVANCED_FACE('',(#1968),#1290,.F.);
#16140=ADVANCED_FACE('',(#1969),#580,.T.);
#16141=ADVANCED_FACE('',(#1970),#581,.T.);
#16142=ADVANCED_FACE('',(#1971,#459),#15768,.T.);
#16143=ADVANCED_FACE('',(#1972),#582,.T.);
#16144=ADVANCED_FACE('',(#1973),#583,.T.);
#16145=ADVANCED_FACE('',(#1974,#460,#461,#462,#463,#464,#465,#466),#15769,
 .T.);
#16146=ADVANCED_FACE('',(#1975,#467),#1291,.T.);
#16147=ADVANCED_FACE('',(#1976),#1292,.T.);
#16148=ADVANCED_FACE('',(#1977),#1293,.F.);
#16149=ADVANCED_FACE('',(#1978),#15770,.T.);
#16150=ADVANCED_FACE('',(#1979),#1294,.F.);
#16151=ADVANCED_FACE('',(#1980),#1295,.F.);
#16152=ADVANCED_FACE('',(#1981),#1296,.F.);
#16153=ADVANCED_FACE('',(#1982),#1297,.F.);
#16154=ADVANCED_FACE('',(#1983),#1298,.F.);
#16155=ADVANCED_FACE('',(#1984),#1299,.F.);
#16156=ADVANCED_FACE('',(#1985),#1300,.F.);
#16157=ADVANCED_FACE('',(#1986),#584,.T.);
#16158=ADVANCED_FACE('',(#1987,#468,#469,#470,#471,#472,#473,#474),#15771,
 .T.);
#16159=ADVANCED_FACE('',(#1988),#585,.F.);
#16160=ADVANCED_FACE('',(#1989),#586,.F.);
#16161=ADVANCED_FACE('',(#1990,#475),#15772,.T.);
#16162=ADVANCED_FACE('',(#1991),#1301,.F.);
#16163=ADVANCED_FACE('',(#1992),#1302,.F.);
#16164=ADVANCED_FACE('',(#1993),#1303,.F.);
#16165=ADVANCED_FACE('',(#1994),#1304,.F.);
#16166=ADVANCED_FACE('',(#1995),#1305,.F.);
#16167=ADVANCED_FACE('',(#1996),#1306,.F.);
#16168=ADVANCED_FACE('',(#1997),#1307,.F.);
#16169=ADVANCED_FACE('',(#1998,#476,#477,#478,#479,#480,#481,#482),#15773,
 .T.);
#16170=ADVANCED_FACE('',(#1999),#1308,.T.);
#16171=ADVANCED_FACE('',(#2000,#483,#484,#485,#486,#487,#488,#489),#15774,
 .T.);
#16172=ADVANCED_FACE('',(#2001),#1309,.F.);
#16173=ADVANCED_FACE('',(#2002),#1310,.F.);
#16174=ADVANCED_FACE('',(#2003),#1311,.F.);
#16175=ADVANCED_FACE('',(#2004),#1312,.F.);
#16176=ADVANCED_FACE('',(#2005),#1313,.F.);
#16177=ADVANCED_FACE('',(#2006),#1314,.F.);
#16178=ADVANCED_FACE('',(#2007),#1315,.F.);
#16179=ADVANCED_FACE('',(#2008,#490),#15775,.T.);
#16180=ADVANCED_FACE('',(#2009),#587,.F.);
#16181=ADVANCED_FACE('',(#2010,#491,#492,#493,#494,#495,#496,#497),#15776,
 .T.);
#16182=ADVANCED_FACE('',(#2011),#1316,.T.);
#16183=ADVANCED_FACE('',(#2012,#498,#499,#500,#501,#502,#503,#504),#15777,
 .T.);
#16184=ADVANCED_FACE('',(#2013),#588,.F.);
#16185=ADVANCED_FACE('',(#2014,#505),#15778,.T.);
#16186=ADVANCED_FACE('',(#2015),#589,.T.);
#16187=ADVANCED_FACE('',(#2016,#506),#15779,.T.);
#16188=ADVANCED_FACE('',(#2017),#590,.T.);
#16189=ADVANCED_FACE('',(#2018),#1317,.F.);
#16190=ADVANCED_FACE('',(#2019),#1318,.T.);
#16191=ADVANCED_FACE('',(#2020,#507),#15780,.T.);
#16192=ADVANCED_FACE('',(#2021),#591,.T.);
#16193=ADVANCED_FACE('',(#2022,#508),#15781,.T.);
#16194=ADVANCED_FACE('',(#2023),#592,.T.);
#16195=ADVANCED_FACE('',(#2024),#593,.F.);
#16196=ADVANCED_FACE('',(#2025),#1319,.F.);
#16197=ADVANCED_FACE('',(#2026,#509),#15782,.T.);
#16198=ADVANCED_FACE('',(#2027),#594,.F.);
#16199=ADVANCED_FACE('',(#2028),#1320,.T.);
#16200=ADVANCED_FACE('',(#2029),#1321,.T.);
#16201=ADVANCED_FACE('',(#2030),#1322,.T.);
#16202=ADVANCED_FACE('',(#2031),#1323,.T.);
#16203=ADVANCED_FACE('',(#2032),#1324,.T.);
#16204=ADVANCED_FACE('',(#2033),#1325,.T.);
#16205=ADVANCED_FACE('',(#2034),#1326,.T.);
#16206=ADVANCED_FACE('',(#2035),#1327,.T.);
#16207=ADVANCED_FACE('',(#2036),#1328,.T.);
#16208=ADVANCED_FACE('',(#2037),#1329,.T.);
#16209=ADVANCED_FACE('',(#2038),#1330,.T.);
#16210=ADVANCED_FACE('',(#2039),#1331,.T.);
#16211=ADVANCED_FACE('',(#2040),#1332,.T.);
#16212=ADVANCED_FACE('',(#2041),#1333,.T.);
#16213=ADVANCED_FACE('',(#2042),#1334,.T.);
#16214=ADVANCED_FACE('',(#2043),#1335,.T.);
#16215=ADVANCED_FACE('',(#2044),#1336,.T.);
#16216=ADVANCED_FACE('',(#2045),#1337,.T.);
#16217=ADVANCED_FACE('',(#2046),#1338,.T.);
#16218=ADVANCED_FACE('',(#2047),#1339,.T.);
#16219=ADVANCED_FACE('',(#2048),#1340,.T.);
#16220=ADVANCED_FACE('',(#2049),#1341,.T.);
#16221=ADVANCED_FACE('',(#2050),#1342,.T.);
#16222=ADVANCED_FACE('',(#2051),#1343,.T.);
#16223=ADVANCED_FACE('',(#2052),#1344,.T.);
#16224=ADVANCED_FACE('',(#2053),#1345,.T.);
#16225=ADVANCED_FACE('',(#2054),#1346,.T.);
#16226=ADVANCED_FACE('',(#2055),#1347,.T.);
#16227=ADVANCED_FACE('',(#2056),#1348,.T.);
#16228=ADVANCED_FACE('',(#2057),#1349,.T.);
#16229=ADVANCED_FACE('',(#2058),#1350,.T.);
#16230=ADVANCED_FACE('',(#2059),#1351,.T.);
#16231=ADVANCED_FACE('',(#2060),#1352,.T.);
#16232=ADVANCED_FACE('',(#2061),#1353,.T.);
#16233=ADVANCED_FACE('',(#2062),#1354,.T.);
#16234=ADVANCED_FACE('',(#2063),#1355,.T.);
#16235=ADVANCED_FACE('',(#2064),#1356,.T.);
#16236=ADVANCED_FACE('',(#2065),#1357,.T.);
#16237=ADVANCED_FACE('',(#2066),#1358,.T.);
#16238=ADVANCED_FACE('',(#2067),#1359,.T.);
#16239=ADVANCED_FACE('',(#2068),#1360,.T.);
#16240=ADVANCED_FACE('',(#2069),#1361,.T.);
#16241=ADVANCED_FACE('',(#2070),#1362,.T.);
#16242=ADVANCED_FACE('',(#2071),#1363,.T.);
#16243=ADVANCED_FACE('',(#2072),#1364,.T.);
#16244=ADVANCED_FACE('',(#2073),#1365,.T.);
#16245=ADVANCED_FACE('',(#2074),#1366,.T.);
#16246=ADVANCED_FACE('',(#2075),#1367,.T.);
#16247=ADVANCED_FACE('',(#2076),#1368,.T.);
#16248=ADVANCED_FACE('',(#2077),#1369,.T.);
#16249=ADVANCED_FACE('',(#2078),#1370,.T.);
#16250=ADVANCED_FACE('',(#2079),#1371,.T.);
#16251=ADVANCED_FACE('',(#2080),#1372,.T.);
#16252=ADVANCED_FACE('',(#2081),#1373,.T.);
#16253=ADVANCED_FACE('',(#2082),#1374,.T.);
#16254=ADVANCED_FACE('',(#2083),#1375,.T.);
#16255=ADVANCED_FACE('',(#2084),#1376,.T.);
#16256=ADVANCED_FACE('',(#2085),#1377,.T.);
#16257=ADVANCED_FACE('',(#2086),#1378,.T.);
#16258=ADVANCED_FACE('',(#2087),#1379,.T.);
#16259=ADVANCED_FACE('',(#2088),#1380,.T.);
#16260=ADVANCED_FACE('',(#2089),#15783,.F.);
#16261=ADVANCED_FACE('',(#2090),#339,.F.);
#16262=ADVANCED_FACE('',(#2091),#1381,.T.);
#16263=ADVANCED_FACE('',(#2092),#340,.F.);
#16264=ADVANCED_FACE('',(#2093),#1382,.T.);
#16265=ADVANCED_FACE('',(#2094),#341,.F.);
#16266=ADVANCED_FACE('',(#2095),#15784,.T.);
#16267=ADVANCED_FACE('',(#2096),#1383,.T.);
#16268=ADVANCED_FACE('',(#2097),#342,.F.);
#16269=ADVANCED_FACE('',(#2098),#15785,.T.);
#16270=ADVANCED_FACE('',(#2099),#595,.T.);
#16271=ADVANCED_FACE('',(#2100),#1384,.T.);
#16272=ADVANCED_FACE('',(#2101,#510),#15786,.T.);
#16273=ADVANCED_FACE('',(#2102),#1385,.T.);
#16274=ADVANCED_FACE('',(#2103,#511),#15787,.T.);
#16275=ADVANCED_FACE('',(#2104),#596,.T.);
#16276=ADVANCED_FACE('',(#2105),#15788,.T.);
#16277=ADVANCED_FACE('',(#2106),#597,.T.);
#16278=ADVANCED_FACE('',(#2107),#343,.T.);
#16279=ADVANCED_FACE('',(#2108),#344,.T.);
#16280=ADVANCED_FACE('',(#2109),#598,.T.);
#16281=ADVANCED_FACE('',(#2110),#599,.T.);
#16282=ADVANCED_FACE('',(#2111),#600,.T.);
#16283=ADVANCED_FACE('',(#2112),#601,.T.);
#16284=ADVANCED_FACE('',(#2113),#602,.T.);
#16285=ADVANCED_FACE('',(#2114),#603,.T.);
#16286=ADVANCED_FACE('',(#2115),#345,.T.);
#16287=ADVANCED_FACE('',(#2116,#512),#15789,.T.);
#16288=ADVANCED_FACE('',(#2117),#15790,.T.);
#16289=ADVANCED_FACE('',(#2118),#15791,.T.);
#16290=ADVANCED_FACE('',(#2119),#15792,.T.);
#16291=ADVANCED_FACE('',(#2120),#15793,.T.);
#16292=ADVANCED_FACE('',(#2121),#15794,.T.);
#16293=ADVANCED_FACE('',(#2122),#15795,.T.);
#16294=ADVANCED_FACE('',(#2123),#346,.T.);
#16295=ADVANCED_FACE('',(#2124),#15796,.T.);
#16296=ADVANCED_FACE('',(#2125),#347,.T.);
#16297=ADVANCED_FACE('',(#2126),#15797,.T.);
#16298=ADVANCED_FACE('',(#2127),#15798,.T.);
#16299=ADVANCED_FACE('',(#2128),#348,.T.);
#16300=ADVANCED_FACE('',(#2129),#15799,.T.);
#16301=ADVANCED_FACE('',(#2130),#15800,.T.);
#16302=ADVANCED_FACE('',(#2131),#15801,.T.);
#16303=ADVANCED_FACE('',(#2132),#15802,.T.);
#16304=ADVANCED_FACE('',(#2133),#15803,.T.);
#16305=ADVANCED_FACE('',(#2134),#15804,.T.);
#16306=ADVANCED_FACE('',(#2135),#604,.T.);
#16307=ADVANCED_FACE('',(#2136),#605,.F.);
#16308=ADVANCED_FACE('',(#2137),#1386,.F.);
#16309=ADVANCED_FACE('',(#2138),#606,.F.);
#16310=ADVANCED_FACE('',(#2139),#15805,.T.);
#16311=ADVANCED_FACE('',(#2140),#15806,.T.);
#16312=ADVANCED_FACE('',(#2141),#15807,.T.);
#16313=ADVANCED_FACE('',(#2142,#513),#15808,.F.);
#16314=ADVANCED_FACE('',(#2143),#607,.F.);
#16315=ADVANCED_FACE('',(#2144,#514),#15809,.F.);
#16316=ADVANCED_FACE('',(#2145),#1387,.F.);
#16317=ADVANCED_FACE('',(#2146),#608,.F.);
#16318=ADVANCED_FACE('',(#2147,#515),#15810,.T.);
#16319=ADVANCED_FACE('',(#2148),#1388,.F.);
#16320=ADVANCED_FACE('',(#2149),#394,.T.);
#16321=ADVANCED_FACE('',(#2150),#1389,.T.);
#16322=ADVANCED_FACE('',(#2151),#395,.T.);
#16323=ADVANCED_FACE('',(#2152,#516),#15811,.T.);
#16324=ADVANCED_FACE('',(#2153),#396,.T.);
#16325=ADVANCED_FACE('',(#2154),#1390,.T.);
#16326=ADVANCED_FACE('',(#2155,#517),#15812,.T.);
#16327=ADVANCED_FACE('',(#2156),#397,.T.);
#16328=ADVANCED_FACE('',(#2157,#518),#15813,.T.);
#16329=ADVANCED_FACE('',(#2158),#1391,.T.);
#16330=ADVANCED_FACE('',(#2159),#398,.T.);
#16331=ADVANCED_FACE('',(#2160),#1392,.T.);
#16332=ADVANCED_FACE('',(#2161),#399,.T.);
#16333=ADVANCED_FACE('',(#2162),#1393,.T.);
#16334=ADVANCED_FACE('',(#2163),#400,.T.);
#16335=ADVANCED_FACE('',(#2164),#1394,.T.);
#16336=ADVANCED_FACE('',(#2165),#401,.T.);
#16337=ADVANCED_FACE('',(#2166),#1395,.T.);
#16338=ADVANCED_FACE('',(#2167),#15814,.T.);
#16339=ADVANCED_FACE('',(#2168),#1396,.T.);
#16340=ADVANCED_FACE('',(#2169,#519),#15815,.T.);
#16341=ADVANCED_FACE('',(#2170,#520,#521,#522),#15816,.T.);
#16342=ADVANCED_FACE('',(#2171),#1397,.T.);
#16343=ADVANCED_FACE('',(#2172),#402,.T.);
#16344=ADVANCED_FACE('',(#2173),#1398,.T.);
#16345=ADVANCED_FACE('',(#2174),#403,.T.);
#16346=ADVANCED_FACE('',(#2175),#1399,.T.);
#16347=ADVANCED_FACE('',(#2176),#404,.T.);
#16348=ADVANCED_FACE('',(#2177),#1400,.T.);
#16349=ADVANCED_FACE('',(#2178),#405,.T.);
#16350=ADVANCED_FACE('',(#2179),#1401,.T.);
#16351=ADVANCED_FACE('',(#2180),#15817,.T.);
#16352=ADVANCED_FACE('',(#2181),#1402,.T.);
#16353=ADVANCED_FACE('',(#2182,#523,#524),#15818,.F.);
#16354=ADVANCED_FACE('',(#2183),#1403,.T.);
#16355=ADVANCED_FACE('',(#2184),#406,.T.);
#16356=ADVANCED_FACE('',(#2185),#1404,.T.);
#16357=ADVANCED_FACE('',(#2186),#407,.T.);
#16358=ADVANCED_FACE('',(#2187),#1405,.T.);
#16359=ADVANCED_FACE('',(#2188),#408,.T.);
#16360=ADVANCED_FACE('',(#2189),#1406,.T.);
#16361=ADVANCED_FACE('',(#2190),#409,.T.);
#16362=ADVANCED_FACE('',(#2191),#1407,.T.);
#16363=ADVANCED_FACE('',(#2192),#15819,.T.);
#16364=ADVANCED_FACE('',(#2193),#1408,.T.);
#16365=ADVANCED_FACE('',(#2194,#525),#15820,.T.);
#16366=ADVANCED_FACE('',(#2195,#526,#527,#528),#15821,.T.);
#16367=ADVANCED_FACE('',(#2196),#1409,.T.);
#16368=ADVANCED_FACE('',(#2197),#410,.T.);
#16369=ADVANCED_FACE('',(#2198),#1410,.T.);
#16370=ADVANCED_FACE('',(#2199),#411,.T.);
#16371=ADVANCED_FACE('',(#2200),#1411,.T.);
#16372=ADVANCED_FACE('',(#2201),#412,.T.);
#16373=ADVANCED_FACE('',(#2202),#1412,.T.);
#16374=ADVANCED_FACE('',(#2203),#413,.T.);
#16375=ADVANCED_FACE('',(#2204),#1413,.T.);
#16376=ADVANCED_FACE('',(#2205),#15822,.T.);
#16377=ADVANCED_FACE('',(#2206),#1414,.T.);
#16378=ADVANCED_FACE('',(#2207,#529,#530),#15823,.F.);
#16379=ADVANCED_FACE('',(#2208),#349,.F.);
#16380=ADVANCED_FACE('',(#2209),#350,.F.);
#16381=ADVANCED_FACE('',(#2210),#351,.F.);
#16382=ADVANCED_FACE('',(#2211),#352,.F.);
#16383=ADVANCED_FACE('',(#2212),#1415,.F.);
#16384=ADVANCED_FACE('',(#2213),#1416,.F.);
#16385=ADVANCED_FACE('',(#2214),#1417,.F.);
#16386=ADVANCED_FACE('',(#2215),#1418,.F.);
#16387=ADVANCED_FACE('',(#2216),#1419,.F.);
#16388=ADVANCED_FACE('',(#2217),#1420,.F.);
#16389=ADVANCED_FACE('',(#2218),#1421,.F.);
#16390=ADVANCED_FACE('',(#2219,#531),#15824,.F.);
#16391=ADVANCED_FACE('',(#2220,#532),#15825,.T.);
#16392=ADVANCED_FACE('',(#2221),#1422,.T.);
#16393=ADVANCED_FACE('',(#2222,#533),#15826,.T.);
#16394=ADVANCED_FACE('',(#2223),#1423,.T.);
#16395=ADVANCED_FACE('',(#2224),#1424,.T.);
#16396=ADVANCED_FACE('',(#2225),#1425,.T.);
#16397=ADVANCED_FACE('',(#2226),#1426,.T.);
#16398=ADVANCED_FACE('',(#2227),#1427,.T.);
#16399=ADVANCED_FACE('',(#2228),#1428,.T.);
#16400=ADVANCED_FACE('',(#2229),#1429,.T.);
#16401=ADVANCED_FACE('',(#2230),#1430,.T.);
#16402=ADVANCED_FACE('',(#2231),#1431,.T.);
#16403=ADVANCED_FACE('',(#2232),#1432,.T.);
#16404=ADVANCED_FACE('',(#2233),#1433,.T.);
#16405=ADVANCED_FACE('',(#2234),#1434,.T.);
#16406=ADVANCED_FACE('',(#2235),#1435,.T.);
#16407=ADVANCED_FACE('',(#2236),#1436,.T.);
#16408=ADVANCED_FACE('',(#2237),#609,.T.);
#16409=ADVANCED_FACE('',(#2238),#1437,.T.);
#16410=ADVANCED_FACE('',(#2239,#534),#15827,.T.);
#16411=ADVANCED_FACE('',(#2240),#610,.T.);
#16412=ADVANCED_FACE('',(#2241),#611,.T.);
#16413=ADVANCED_FACE('',(#2242),#612,.T.);
#16414=ADVANCED_FACE('',(#2243,#535),#15828,.T.);
#16415=ADVANCED_FACE('',(#2244),#15829,.T.);
#16416=ADVANCED_FACE('',(#2245),#15830,.T.);
#16417=ADVANCED_FACE('',(#2246),#15831,.T.);
#16418=ADVANCED_FACE('',(#2247),#15832,.T.);
#16419=ADVANCED_FACE('',(#2248),#15833,.T.);
#16420=ADVANCED_FACE('',(#2249),#15834,.T.);
#16421=ADVANCED_FACE('',(#2250),#15835,.F.);
#16422=ADVANCED_FACE('',(#2251),#15836,.F.);
#16423=ADVANCED_FACE('',(#2252),#15837,.F.);
#16424=ADVANCED_FACE('',(#2253),#15838,.F.);
#16425=ADVANCED_FACE('',(#2254),#353,.F.);
#16426=ADVANCED_FACE('',(#2255),#1438,.T.);
#16427=ADVANCED_FACE('',(#2256),#354,.F.);
#16428=ADVANCED_FACE('',(#2257),#1439,.T.);
#16429=ADVANCED_FACE('',(#2258),#15839,.F.);
#16430=ADVANCED_FACE('',(#2259),#15840,.F.);
#16431=ADVANCED_FACE('',(#2260),#15841,.F.);
#16432=ADVANCED_FACE('',(#2261),#15842,.F.);
#16433=ADVANCED_FACE('',(#2262),#613,.T.);
#16434=ADVANCED_FACE('',(#2263),#15843,.T.);
#16435=ADVANCED_FACE('',(#2264,#536),#15844,.F.);
#16436=ADVANCED_FACE('',(#2265),#15845,.T.);
#16437=ADVANCED_FACE('',(#2266),#1440,.T.);
#16438=ADVANCED_FACE('',(#2267),#15846,.T.);
#16439=ADVANCED_FACE('',(#2268),#1441,.T.);
#16440=ADVANCED_FACE('',(#2269),#15847,.T.);
#16441=ADVANCED_FACE('',(#2270),#1442,.T.);
#16442=ADVANCED_FACE('',(#2271),#15848,.T.);
#16443=ADVANCED_FACE('',(#2272),#1443,.T.);
#16444=ADVANCED_FACE('',(#2273),#15849,.T.);
#16445=ADVANCED_FACE('',(#2274),#1444,.T.);
#16446=ADVANCED_FACE('',(#2275),#15850,.T.);
#16447=ADVANCED_FACE('',(#2276),#15851,.F.);
#16448=ADVANCED_FACE('',(#2277),#1445,.F.);
#16449=ADVANCED_FACE('',(#2278),#15852,.T.);
#16450=ADVANCED_FACE('',(#2279),#15853,.T.);
#16451=ADVANCED_FACE('',(#2280),#15854,.T.);
#16452=ADVANCED_FACE('',(#2281),#15855,.T.);
#16453=ADVANCED_FACE('',(#2282),#15856,.T.);
#16454=ADVANCED_FACE('',(#2283),#15857,.T.);
#16455=ADVANCED_FACE('',(#2284),#1446,.T.);
#16456=ADVANCED_FACE('',(#2285),#614,.T.);
#16457=ADVANCED_FACE('',(#2286,#537),#15858,.T.);
#16458=ADVANCED_FACE('',(#2287),#15859,.T.);
#16459=ADVANCED_FACE('',(#2288),#15860,.T.);
#16460=ADVANCED_FACE('',(#2289),#15861,.T.);
#16461=ADVANCED_FACE('',(#2290),#15862,.T.);
#16462=ADVANCED_FACE('',(#2291),#15863,.T.);
#16463=ADVANCED_FACE('',(#2292,#538),#15864,.T.);
#16464=ADVANCED_FACE('',(#2293),#15865,.T.);
#16465=ADVANCED_FACE('',(#2294),#15866,.T.);
#16466=ADVANCED_FACE('',(#2295),#15867,.T.);
#16467=ADVANCED_FACE('',(#2296),#15868,.T.);
#16468=ADVANCED_FACE('',(#2297),#15869,.T.);
#16469=ADVANCED_FACE('',(#2298),#15870,.T.);
#16470=ADVANCED_FACE('',(#2299),#15871,.T.);
#16471=ADVANCED_FACE('',(#2300),#615,.T.);
#16472=ADVANCED_FACE('',(#2301),#1447,.T.);
#16473=ADVANCED_FACE('',(#2302),#15872,.T.);
#16474=ADVANCED_FACE('',(#2303),#15873,.T.);
#16475=ADVANCED_FACE('',(#2304),#15874,.T.);
#16476=ADVANCED_FACE('',(#2305),#15875,.T.);
#16477=ADVANCED_FACE('',(#2306),#15876,.T.);
#16478=ADVANCED_FACE('',(#2307),#15877,.T.);
#16479=ADVANCED_FACE('',(#2308),#15878,.T.);
#16480=ADVANCED_FACE('',(#2309),#15879,.T.);
#16481=ADVANCED_FACE('',(#2310),#15880,.T.);
#16482=ADVANCED_FACE('',(#2311),#15881,.T.);
#16483=ADVANCED_FACE('',(#2312),#15882,.T.);
#16484=ADVANCED_FACE('',(#2313),#15883,.T.);
#16485=ADVANCED_FACE('',(#2314),#15884,.T.);
#16486=ADVANCED_FACE('',(#2315),#15885,.T.);
#16487=ADVANCED_FACE('',(#2316),#15886,.T.);
#16488=ADVANCED_FACE('',(#2317),#15887,.T.);
#16489=ADVANCED_FACE('',(#2318),#15888,.T.);
#16490=ADVANCED_FACE('',(#2319),#15889,.T.);
#16491=ADVANCED_FACE('',(#2320),#15890,.T.);
#16492=ADVANCED_FACE('',(#2321),#15891,.T.);
#16493=ADVANCED_FACE('',(#2322),#15892,.T.);
#16494=ADVANCED_FACE('',(#2323,#539),#15893,.F.);
#16495=ADVANCED_FACE('',(#2324),#616,.T.);
#16496=ADVANCED_FACE('',(#2325),#617,.T.);
#16497=ADVANCED_FACE('',(#2326),#1448,.T.);
#16498=ADVANCED_FACE('',(#2327),#618,.T.);
#16499=ADVANCED_FACE('',(#2328),#15894,.T.);
#16500=ADVANCED_FACE('',(#2329),#619,.T.);
#16501=ADVANCED_FACE('',(#2330),#1449,.T.);
#16502=ADVANCED_FACE('',(#2331,#540),#15895,.T.);
#16503=ADVANCED_FACE('',(#2332,#541),#15896,.F.);
#16504=ADVANCED_FACE('',(#2333,#542),#15897,.F.);
#16505=ADVANCED_FACE('',(#2334),#1450,.T.);
#16506=ADVANCED_FACE('',(#2335),#1451,.T.);
#16507=ADVANCED_FACE('',(#2336,#543),#15898,.F.);
#16508=ADVANCED_FACE('',(#2337,#544),#15899,.F.);
#16509=ADVANCED_FACE('',(#2338),#1452,.T.);
#16510=ADVANCED_FACE('',(#2339),#15900,.T.);
#16511=ADVANCED_FACE('',(#2340),#15901,.T.);
#16512=ADVANCED_FACE('',(#2341),#15902,.T.);
#16513=ADVANCED_FACE('',(#2342),#1453,.T.);
#16514=ADVANCED_FACE('',(#2343),#620,.T.);
#16515=ADVANCED_FACE('',(#2344),#15903,.T.);
#16516=ADVANCED_FACE('',(#2345),#243,.T.);
#16517=ADVANCED_FACE('',(#2346),#1454,.F.);
#16518=ADVANCED_FACE('',(#2347,#545),#15904,.T.);
#16519=ADVANCED_FACE('',(#2348),#621,.T.);
#16520=ADVANCED_FACE('',(#2349),#1455,.T.);
#16521=ADVANCED_FACE('',(#2350),#622,.T.);
#16522=ADVANCED_FACE('',(#2351,#546),#15905,.T.);
#16523=ADVANCED_FACE('',(#2352),#623,.F.);
#16524=ADVANCED_FACE('',(#2353,#547,#548,#549,#550,#551,#552),#15906,.T.);
#16525=ADVANCED_FACE('',(#2354),#1456,.F.);
#16526=ADVANCED_FACE('',(#2355),#624,.F.);
#16527=ADVANCED_FACE('',(#2356),#1457,.F.);
#16528=ADVANCED_FACE('',(#2357),#15907,.T.);
#16529=ADVANCED_FACE('',(#2358),#625,.T.);
#16530=ADVANCED_FACE('',(#2359),#15908,.T.);
#16531=ADVANCED_FACE('',(#2360),#626,.T.);
#16532=ADVANCED_FACE('',(#2361),#15909,.T.);
#16533=ADVANCED_FACE('',(#2362),#627,.T.);
#16534=ADVANCED_FACE('',(#2363),#15910,.T.);
#16535=ADVANCED_FACE('',(#2364),#628,.F.);
#16536=ADVANCED_FACE('',(#2365),#15911,.T.);
#16537=ADVANCED_FACE('',(#2366),#629,.F.);
#16538=ADVANCED_FACE('',(#2367),#15912,.T.);
#16539=ADVANCED_FACE('',(#2368),#630,.T.);
#16540=ADVANCED_FACE('',(#2369),#15913,.T.);
#16541=ADVANCED_FACE('',(#2370),#631,.T.);
#16542=ADVANCED_FACE('',(#2371),#15914,.T.);
#16543=ADVANCED_FACE('',(#2372),#632,.T.);
#16544=ADVANCED_FACE('',(#2373),#1458,.F.);
#16545=ADVANCED_FACE('',(#2374),#15915,.T.);
#16546=ADVANCED_FACE('',(#2375),#1459,.T.);
#16547=ADVANCED_FACE('',(#2376),#15916,.T.);
#16548=ADVANCED_FACE('',(#2377),#1460,.T.);
#16549=ADVANCED_FACE('',(#2378),#15917,.T.);
#16550=ADVANCED_FACE('',(#2379),#1461,.T.);
#16551=ADVANCED_FACE('',(#2380,#553,#554,#555,#556,#557,#558),#15918,.T.);
#16552=ADVANCED_FACE('',(#2381),#15919,.F.);
#16553=ADVANCED_FACE('',(#2382),#15920,.T.);
#16554=ADVANCED_FACE('',(#2383),#633,.T.);
#16555=ADVANCED_FACE('',(#2384),#15921,.T.);
#16556=ADVANCED_FACE('',(#2385),#634,.T.);
#16557=ADVANCED_FACE('',(#2386),#15922,.T.);
#16558=ADVANCED_FACE('',(#2387),#635,.T.);
#16559=ADVANCED_FACE('',(#2388),#15923,.T.);
#16560=ADVANCED_FACE('',(#2389),#636,.F.);
#16561=ADVANCED_FACE('',(#2390),#15924,.T.);
#16562=ADVANCED_FACE('',(#2391),#637,.F.);
#16563=ADVANCED_FACE('',(#2392),#15925,.T.);
#16564=ADVANCED_FACE('',(#2393),#638,.T.);
#16565=ADVANCED_FACE('',(#2394),#15926,.T.);
#16566=ADVANCED_FACE('',(#2395),#639,.T.);
#16567=ADVANCED_FACE('',(#2396),#15927,.T.);
#16568=ADVANCED_FACE('',(#2397),#640,.T.);
#16569=ADVANCED_FACE('',(#2398),#1462,.F.);
#16570=ADVANCED_FACE('',(#2399),#15928,.T.);
#16571=ADVANCED_FACE('',(#2400),#1463,.T.);
#16572=ADVANCED_FACE('',(#2401),#15929,.T.);
#16573=ADVANCED_FACE('',(#2402),#1464,.T.);
#16574=ADVANCED_FACE('',(#2403),#15930,.T.);
#16575=ADVANCED_FACE('',(#2404),#1465,.T.);
#16576=ADVANCED_FACE('',(#2405),#15931,.T.);
#16577=ADVANCED_FACE('',(#2406),#641,.F.);
#16578=ADVANCED_FACE('',(#2407),#642,.F.);
#16579=ADVANCED_FACE('',(#2408),#1466,.F.);
#16580=ADVANCED_FACE('',(#2409),#1467,.F.);
#16581=ADVANCED_FACE('',(#2410),#1468,.F.);
#16582=ADVANCED_FACE('',(#2411),#1469,.F.);
#16583=ADVANCED_FACE('',(#2412),#1470,.T.);
#16584=ADVANCED_FACE('',(#2413),#1471,.T.);
#16585=ADVANCED_FACE('',(#2414),#1472,.T.);
#16586=ADVANCED_FACE('',(#2415),#1473,.T.);
#16587=ADVANCED_FACE('',(#2416),#1474,.T.);
#16588=ADVANCED_FACE('',(#2417),#1475,.T.);
#16589=ADVANCED_FACE('',(#2418),#1476,.T.);
#16590=ADVANCED_FACE('',(#2419),#1477,.T.);
#16591=ADVANCED_FACE('',(#2420),#1478,.T.);
#16592=ADVANCED_FACE('',(#2421),#1479,.T.);
#16593=ADVANCED_FACE('',(#2422),#1480,.T.);
#16594=ADVANCED_FACE('',(#2423),#1481,.T.);
#16595=ADVANCED_FACE('',(#2424),#1482,.T.);
#16596=ADVANCED_FACE('',(#2425),#1483,.T.);
#16597=ADVANCED_FACE('',(#2426),#1484,.T.);
#16598=ADVANCED_FACE('',(#2427),#1485,.T.);
#16599=ADVANCED_FACE('',(#2428),#1486,.T.);
#16600=ADVANCED_FACE('',(#2429),#1487,.T.);
#16601=ADVANCED_FACE('',(#2430),#1488,.T.);
#16602=ADVANCED_FACE('',(#2431),#643,.T.);
#16603=ADVANCED_FACE('',(#2432),#644,.T.);
#16604=ADVANCED_FACE('',(#2433),#1489,.T.);
#16605=ADVANCED_FACE('',(#2434),#645,.T.);
#16606=ADVANCED_FACE('',(#2435),#15932,.T.);
#16607=ADVANCED_FACE('',(#2436),#15933,.F.);
#16608=ADVANCED_FACE('',(#2437),#355,.F.);
#16609=ADVANCED_FACE('',(#2438),#1490,.T.);
#16610=ADVANCED_FACE('',(#2439),#356,.F.);
#16611=ADVANCED_FACE('',(#2440),#1491,.T.);
#16612=ADVANCED_FACE('',(#2441),#646,.T.);
#16613=ADVANCED_FACE('',(#2442,#559),#15934,.T.);
#16614=ADVANCED_FACE('',(#2443),#647,.T.);
#16615=ADVANCED_FACE('',(#2444),#15935,.T.);
#16616=ADVANCED_FACE('',(#2445),#1492,.T.);
#16617=ADVANCED_FACE('',(#2446),#1493,.T.);
#16618=ADVANCED_FACE('',(#2447),#1494,.T.);
#16619=ADVANCED_FACE('',(#2448),#1495,.T.);
#16620=ADVANCED_FACE('',(#2449),#1496,.T.);
#16621=ADVANCED_FACE('',(#2450),#1497,.T.);
#16622=ADVANCED_FACE('',(#2451),#1498,.T.);
#16623=ADVANCED_FACE('',(#2452),#1499,.T.);
#16624=ADVANCED_FACE('',(#2453),#1500,.T.);
#16625=ADVANCED_FACE('',(#2454),#1501,.T.);
#16626=ADVANCED_FACE('',(#2455),#1502,.T.);
#16627=ADVANCED_FACE('',(#2456),#1503,.T.);
#16628=ADVANCED_FACE('',(#2457),#1504,.T.);
#16629=ADVANCED_FACE('',(#2458),#1505,.T.);
#16630=ADVANCED_FACE('',(#2459),#1506,.T.);
#16631=ADVANCED_FACE('',(#2460),#1507,.T.);
#16632=ADVANCED_FACE('',(#2461),#1508,.T.);
#16633=ADVANCED_FACE('',(#2462),#1509,.T.);
#16634=ADVANCED_FACE('',(#2463),#1510,.T.);
#16635=ADVANCED_FACE('',(#2464),#1511,.T.);
#16636=ADVANCED_FACE('',(#2465),#1512,.T.);
#16637=ADVANCED_FACE('',(#2466),#1513,.T.);
#16638=ADVANCED_FACE('',(#2467),#1514,.T.);
#16639=ADVANCED_FACE('',(#2468),#1515,.T.);
#16640=ADVANCED_FACE('',(#2469),#1516,.T.);
#16641=ADVANCED_FACE('',(#2470),#1517,.T.);
#16642=ADVANCED_FACE('',(#2471),#1518,.T.);
#16643=ADVANCED_FACE('',(#2472),#1519,.T.);
#16644=ADVANCED_FACE('',(#2473),#1520,.T.);
#16645=ADVANCED_FACE('',(#2474),#1521,.T.);
#16646=ADVANCED_FACE('',(#2475),#1522,.T.);
#16647=ADVANCED_FACE('',(#2476),#1523,.T.);
#16648=ADVANCED_FACE('',(#2477),#1524,.T.);
#16649=ADVANCED_FACE('',(#2478),#1525,.T.);
#16650=ADVANCED_FACE('',(#2479),#1526,.T.);
#16651=ADVANCED_FACE('',(#2480),#1527,.T.);
#16652=ADVANCED_FACE('',(#2481),#1528,.T.);
#16653=ADVANCED_FACE('',(#2482),#1529,.T.);
#16654=ADVANCED_FACE('',(#2483),#1530,.T.);
#16655=ADVANCED_FACE('',(#2484),#1531,.T.);
#16656=ADVANCED_FACE('',(#2485),#1532,.T.);
#16657=ADVANCED_FACE('',(#2486),#1533,.T.);
#16658=ADVANCED_FACE('',(#2487),#1534,.T.);
#16659=ADVANCED_FACE('',(#2488),#1535,.T.);
#16660=ADVANCED_FACE('',(#2489),#1536,.T.);
#16661=ADVANCED_FACE('',(#2490),#1537,.T.);
#16662=ADVANCED_FACE('',(#2491),#1538,.T.);
#16663=ADVANCED_FACE('',(#2492),#1539,.T.);
#16664=ADVANCED_FACE('',(#2493),#1540,.T.);
#16665=ADVANCED_FACE('',(#2494),#1541,.T.);
#16666=ADVANCED_FACE('',(#2495),#1542,.T.);
#16667=ADVANCED_FACE('',(#2496),#1543,.T.);
#16668=ADVANCED_FACE('',(#2497),#1544,.T.);
#16669=ADVANCED_FACE('',(#2498),#1545,.T.);
#16670=ADVANCED_FACE('',(#2499),#1546,.T.);
#16671=ADVANCED_FACE('',(#2500),#1547,.T.);
#16672=ADVANCED_FACE('',(#2501),#1548,.T.);
#16673=ADVANCED_FACE('',(#2502),#1549,.T.);
#16674=ADVANCED_FACE('',(#2503),#1550,.T.);
#16675=ADVANCED_FACE('',(#2504),#1551,.T.);
#16676=ADVANCED_FACE('',(#2505),#1552,.T.);
#16677=ADVANCED_FACE('',(#2506),#1553,.T.);
#16678=ADVANCED_FACE('',(#2507),#1554,.T.);
#16679=ADVANCED_FACE('',(#2508),#1555,.T.);
#16680=ADVANCED_FACE('',(#2509),#1556,.T.);
#16681=ADVANCED_FACE('',(#2510),#1557,.T.);
#16682=ADVANCED_FACE('',(#2511),#1558,.T.);
#16683=ADVANCED_FACE('',(#2512),#1559,.T.);
#16684=ADVANCED_FACE('',(#2513),#1560,.T.);
#16685=ADVANCED_FACE('',(#2514),#1561,.T.);
#16686=ADVANCED_FACE('',(#2515),#1562,.T.);
#16687=ADVANCED_FACE('',(#2516),#1563,.T.);
#16688=ADVANCED_FACE('',(#2517),#1564,.T.);
#16689=ADVANCED_FACE('',(#2518),#1565,.T.);
#16690=ADVANCED_FACE('',(#2519),#1566,.T.);
#16691=ADVANCED_FACE('',(#2520),#1567,.T.);
#16692=ADVANCED_FACE('',(#2521),#1568,.T.);
#16693=ADVANCED_FACE('',(#2522),#1569,.T.);
#16694=ADVANCED_FACE('',(#2523),#1570,.T.);
#16695=ADVANCED_FACE('',(#2524),#1571,.T.);
#16696=ADVANCED_FACE('',(#2525),#1572,.T.);
#16697=ADVANCED_FACE('',(#2526),#1573,.T.);
#16698=ADVANCED_FACE('',(#2527),#1574,.T.);
#16699=ADVANCED_FACE('',(#2528),#1575,.T.);
#16700=ADVANCED_FACE('',(#2529),#1576,.T.);
#16701=ADVANCED_FACE('',(#2530),#1577,.T.);
#16702=ADVANCED_FACE('',(#2531),#1578,.T.);
#16703=ADVANCED_FACE('',(#2532),#1579,.T.);
#16704=ADVANCED_FACE('',(#2533),#357,.F.);
#16705=ADVANCED_FACE('',(#2534),#15936,.T.);
#16706=ADVANCED_FACE('',(#2535),#1580,.T.);
#16707=ADVANCED_FACE('',(#2536),#358,.F.);
#16708=ADVANCED_FACE('',(#2537),#648,.T.);
#16709=ADVANCED_FACE('',(#2538),#15937,.T.);
#16710=ADVANCED_FACE('',(#2539),#15938,.T.);
#16711=ADVANCED_FACE('',(#2540),#15939,.T.);
#16712=ADVANCED_FACE('',(#2541,#560),#15940,.F.);
#16713=ADVANCED_FACE('',(#2542),#15941,.T.);
#16714=ADVANCED_FACE('',(#2543),#15942,.T.);
#16715=ADVANCED_FACE('',(#2544),#15943,.T.);
#16716=ADVANCED_FACE('',(#2545),#15944,.T.);
#16717=ADVANCED_FACE('',(#2546),#15945,.T.);
#16718=ADVANCED_FACE('',(#2547),#649,.T.);
#16719=ADVANCED_FACE('',(#2548),#1581,.T.);
#16720=ADVANCED_FACE('',(#2549),#1582,.T.);
#16721=ADVANCED_FACE('',(#2550),#1583,.T.);
#16722=ADVANCED_FACE('',(#2551),#1584,.T.);
#16723=ADVANCED_FACE('',(#2552),#1585,.T.);
#16724=ADVANCED_FACE('',(#2553),#1586,.T.);
#16725=ADVANCED_FACE('',(#2554),#1587,.T.);
#16726=ADVANCED_FACE('',(#2555),#1588,.T.);
#16727=ADVANCED_FACE('',(#2556),#1589,.T.);
#16728=ADVANCED_FACE('',(#2557),#1590,.T.);
#16729=ADVANCED_FACE('',(#2558),#1591,.T.);
#16730=ADVANCED_FACE('',(#2559),#1592,.T.);
#16731=ADVANCED_FACE('',(#2560),#1593,.T.);
#16732=ADVANCED_FACE('',(#2561),#1594,.T.);
#16733=ADVANCED_FACE('',(#2562),#1595,.T.);
#16734=ADVANCED_FACE('',(#2563),#1596,.T.);
#16735=ADVANCED_FACE('',(#2564),#1597,.T.);
#16736=ADVANCED_FACE('',(#2565),#1598,.T.);
#16737=ADVANCED_FACE('',(#2566),#1599,.T.);
#16738=ADVANCED_FACE('',(#2567),#1600,.T.);
#16739=ADVANCED_FACE('',(#2568),#1601,.T.);
#16740=ADVANCED_FACE('',(#2569),#1602,.T.);
#16741=ADVANCED_FACE('',(#2570),#1603,.T.);
#16742=ADVANCED_FACE('',(#2571),#1604,.T.);
#16743=ADVANCED_FACE('',(#2572),#1605,.T.);
#16744=ADVANCED_FACE('',(#2573),#1606,.T.);
#16745=ADVANCED_FACE('',(#2574),#1607,.T.);
#16746=ADVANCED_FACE('',(#2575),#1608,.T.);
#16747=ADVANCED_FACE('',(#2576),#1609,.T.);
#16748=ADVANCED_FACE('',(#2577),#1610,.T.);
#16749=ADVANCED_FACE('',(#2578),#1611,.T.);
#16750=ADVANCED_FACE('',(#2579),#1612,.T.);
#16751=ADVANCED_FACE('',(#2580),#1613,.T.);
#16752=ADVANCED_FACE('',(#2581),#1614,.T.);
#16753=ADVANCED_FACE('',(#2582),#1615,.T.);
#16754=ADVANCED_FACE('',(#2583),#1616,.T.);
#16755=ADVANCED_FACE('',(#2584),#1617,.T.);
#16756=ADVANCED_FACE('',(#2585),#1618,.T.);
#16757=ADVANCED_FACE('',(#2586),#1619,.T.);
#16758=ADVANCED_FACE('',(#2587),#1620,.T.);
#16759=ADVANCED_FACE('',(#2588),#1621,.T.);
#16760=ADVANCED_FACE('',(#2589),#1622,.T.);
#16761=ADVANCED_FACE('',(#2590),#1623,.T.);
#16762=ADVANCED_FACE('',(#2591),#1624,.T.);
#16763=ADVANCED_FACE('',(#2592),#1625,.T.);
#16764=ADVANCED_FACE('',(#2593),#1626,.T.);
#16765=ADVANCED_FACE('',(#2594),#1627,.T.);
#16766=ADVANCED_FACE('',(#2595),#1628,.T.);
#16767=ADVANCED_FACE('',(#2596),#1629,.T.);
#16768=ADVANCED_FACE('',(#2597),#1630,.T.);
#16769=ADVANCED_FACE('',(#2598),#1631,.T.);
#16770=ADVANCED_FACE('',(#2599),#1632,.T.);
#16771=ADVANCED_FACE('',(#2600),#1633,.T.);
#16772=ADVANCED_FACE('',(#2601),#1634,.T.);
#16773=ADVANCED_FACE('',(#2602),#1635,.T.);
#16774=ADVANCED_FACE('',(#2603),#1636,.T.);
#16775=ADVANCED_FACE('',(#2604),#1637,.T.);
#16776=ADVANCED_FACE('',(#2605),#1638,.T.);
#16777=ADVANCED_FACE('',(#2606),#1639,.T.);
#16778=ADVANCED_FACE('',(#2607),#1640,.T.);
#16779=ADVANCED_FACE('',(#2608),#1641,.T.);
#16780=ADVANCED_FACE('',(#2609),#1642,.T.);
#16781=ADVANCED_FACE('',(#2610),#1643,.T.);
#16782=ADVANCED_FACE('',(#2611),#1644,.T.);
#16783=ADVANCED_FACE('',(#2612),#1645,.T.);
#16784=ADVANCED_FACE('',(#2613),#1646,.T.);
#16785=ADVANCED_FACE('',(#2614),#1647,.T.);
#16786=ADVANCED_FACE('',(#2615),#1648,.T.);
#16787=ADVANCED_FACE('',(#2616),#1649,.T.);
#16788=ADVANCED_FACE('',(#2617),#1650,.T.);
#16789=ADVANCED_FACE('',(#2618),#1651,.T.);
#16790=ADVANCED_FACE('',(#2619),#1652,.T.);
#16791=ADVANCED_FACE('',(#2620),#1653,.T.);
#16792=ADVANCED_FACE('',(#2621),#1654,.T.);
#16793=ADVANCED_FACE('',(#2622),#1655,.T.);
#16794=ADVANCED_FACE('',(#2623),#1656,.T.);
#16795=ADVANCED_FACE('',(#2624),#1657,.T.);
#16796=ADVANCED_FACE('',(#2625),#1658,.T.);
#16797=ADVANCED_FACE('',(#2626),#1659,.T.);
#16798=ADVANCED_FACE('',(#2627),#1660,.T.);
#16799=ADVANCED_FACE('',(#2628),#1661,.T.);
#16800=ADVANCED_FACE('',(#2629),#1662,.T.);
#16801=ADVANCED_FACE('',(#2630),#1663,.T.);
#16802=ADVANCED_FACE('',(#2631),#1664,.T.);
#16803=ADVANCED_FACE('',(#2632),#1665,.T.);
#16804=ADVANCED_FACE('',(#2633),#1666,.T.);
#16805=ADVANCED_FACE('',(#2634),#1667,.T.);
#16806=ADVANCED_FACE('',(#2635),#1668,.T.);
#16807=ADVANCED_FACE('',(#2636),#1669,.T.);
#16808=ADVANCED_FACE('',(#2637),#1670,.T.);
#16809=ADVANCED_FACE('',(#2638),#1671,.T.);
#16810=ADVANCED_FACE('',(#2639),#1672,.T.);
#16811=ADVANCED_FACE('',(#2640),#1673,.T.);
#16812=ADVANCED_FACE('',(#2641),#1674,.T.);
#16813=ADVANCED_FACE('',(#2642),#1675,.T.);
#16814=ADVANCED_FACE('',(#2643),#1676,.T.);
#16815=ADVANCED_FACE('',(#2644),#1677,.T.);
#16816=ADVANCED_FACE('',(#2645),#1678,.T.);
#16817=ADVANCED_FACE('',(#2646),#1679,.T.);
#16818=ADVANCED_FACE('',(#2647),#1680,.T.);
#16819=ADVANCED_FACE('',(#2648),#1681,.T.);
#16820=ADVANCED_FACE('',(#2649),#1682,.T.);
#16821=ADVANCED_FACE('',(#2650),#1683,.T.);
#16822=ADVANCED_FACE('',(#2651),#1684,.T.);
#16823=ADVANCED_FACE('',(#2652),#1685,.T.);
#16824=ADVANCED_FACE('',(#2653),#1686,.T.);
#16825=ADVANCED_FACE('',(#2654),#1687,.T.);
#16826=ADVANCED_FACE('',(#2655),#1688,.T.);
#16827=ADVANCED_FACE('',(#2656),#1689,.T.);
#16828=ADVANCED_FACE('',(#2657),#1690,.T.);
#16829=ADVANCED_FACE('',(#2658),#1691,.T.);
#16830=ADVANCED_FACE('',(#2659),#1692,.T.);
#16831=ADVANCED_FACE('',(#2660),#1693,.T.);
#16832=ADVANCED_FACE('',(#2661),#1694,.T.);
#16833=ADVANCED_FACE('',(#2662),#1695,.T.);
#16834=ADVANCED_FACE('',(#2663),#1696,.T.);
#16835=ADVANCED_FACE('',(#2664),#1697,.T.);
#16836=ADVANCED_FACE('',(#2665),#1698,.T.);
#16837=ADVANCED_FACE('',(#2666),#1699,.T.);
#16838=ADVANCED_FACE('',(#2667),#1700,.T.);
#16839=ADVANCED_FACE('',(#2668),#1701,.T.);
#16840=ADVANCED_FACE('',(#2669),#1702,.T.);
#16841=ADVANCED_FACE('',(#2670),#1703,.T.);
#16842=ADVANCED_FACE('',(#2671),#1704,.T.);
#16843=ADVANCED_FACE('',(#2672),#1705,.T.);
#16844=ADVANCED_FACE('',(#2673),#1706,.T.);
#16845=ADVANCED_FACE('',(#2674),#1707,.T.);
#16846=ADVANCED_FACE('',(#2675),#1708,.T.);
#16847=ADVANCED_FACE('',(#2676),#1709,.T.);
#16848=ADVANCED_FACE('',(#2677),#1710,.T.);
#16849=ADVANCED_FACE('',(#2678),#1711,.T.);
#16850=ADVANCED_FACE('',(#2679),#1712,.T.);
#16851=ADVANCED_FACE('',(#2680),#1713,.T.);
#16852=ADVANCED_FACE('',(#2681),#1714,.T.);
#16853=ADVANCED_FACE('',(#2682),#1715,.T.);
#16854=ADVANCED_FACE('',(#2683),#1716,.T.);
#16855=ADVANCED_FACE('',(#2684),#1717,.T.);
#16856=ADVANCED_FACE('',(#2685),#1718,.T.);
#16857=ADVANCED_FACE('',(#2686),#1719,.T.);
#16858=ADVANCED_FACE('',(#2687),#1720,.T.);
#16859=ADVANCED_FACE('',(#2688),#1721,.T.);
#16860=ADVANCED_FACE('',(#2689),#1722,.T.);
#16861=ADVANCED_FACE('',(#2690),#1723,.T.);
#16862=ADVANCED_FACE('',(#2691),#1724,.T.);
#16863=ADVANCED_FACE('',(#2692),#1725,.T.);
#16864=ADVANCED_FACE('',(#2693),#1726,.T.);
#16865=ADVANCED_FACE('',(#2694),#1727,.T.);
#16866=ADVANCED_FACE('',(#2695),#1728,.T.);
#16867=ADVANCED_FACE('',(#2696),#1729,.T.);
#16868=ADVANCED_FACE('',(#2697),#1730,.T.);
#16869=ADVANCED_FACE('',(#2698),#1731,.T.);
#16870=ADVANCED_FACE('',(#2699),#1732,.T.);
#16871=ADVANCED_FACE('',(#2700),#1733,.T.);
#16872=ADVANCED_FACE('',(#2701),#1734,.T.);
#16873=ADVANCED_FACE('',(#2702),#1735,.T.);
#16874=ADVANCED_FACE('',(#2703),#1736,.T.);
#16875=ADVANCED_FACE('',(#2704),#1737,.T.);
#16876=ADVANCED_FACE('',(#2705),#1738,.T.);
#16877=ADVANCED_FACE('',(#2706),#1739,.T.);
#16878=ADVANCED_FACE('',(#2707),#1740,.T.);
#16879=ADVANCED_FACE('',(#2708),#1741,.T.);
#16880=ADVANCED_FACE('',(#2709),#1742,.T.);
#16881=ADVANCED_FACE('',(#2710),#1743,.T.);
#16882=ADVANCED_FACE('',(#2711),#1744,.T.);
#16883=ADVANCED_FACE('',(#2712),#1745,.T.);
#16884=ADVANCED_FACE('',(#2713),#1746,.T.);
#16885=ADVANCED_FACE('',(#2714),#1747,.T.);
#16886=ADVANCED_FACE('',(#2715),#1748,.T.);
#16887=ADVANCED_FACE('',(#2716),#1749,.T.);
#16888=ADVANCED_FACE('',(#2717),#1750,.T.);
#16889=ADVANCED_FACE('',(#2718),#1751,.T.);
#16890=ADVANCED_FACE('',(#2719),#1752,.T.);
#16891=ADVANCED_FACE('',(#2720),#1753,.T.);
#16892=ADVANCED_FACE('',(#2721),#1754,.T.);
#16893=ADVANCED_FACE('',(#2722),#1755,.T.);
#16894=ADVANCED_FACE('',(#2723),#1756,.T.);
#16895=ADVANCED_FACE('',(#2724),#1757,.T.);
#16896=ADVANCED_FACE('',(#2725),#359,.F.);
#16897=ADVANCED_FACE('',(#2726),#15946,.T.);
#16898=ADVANCED_FACE('',(#2727),#1758,.T.);
#16899=ADVANCED_FACE('',(#2728),#360,.F.);
#16900=ADVANCED_FACE('',(#2729),#650,.T.);
#16901=ADVANCED_FACE('',(#2730),#15947,.T.);
#16902=ADVANCED_FACE('',(#2731),#15948,.T.);
#16903=ADVANCED_FACE('',(#2732),#15949,.T.);
#16904=ADVANCED_FACE('',(#2733,#561),#15950,.F.);
#16905=ADVANCED_FACE('',(#2734),#15951,.T.);
#16906=ADVANCED_FACE('',(#2735),#15952,.T.);
#16907=ADVANCED_FACE('',(#2736),#15953,.T.);
#16908=ADVANCED_FACE('',(#2737),#15954,.T.);
#16909=ADVANCED_FACE('',(#2738),#15955,.T.);
#16910=ADVANCED_FACE('',(#2739),#651,.T.);
#16911=ADVANCED_FACE('',(#2740),#1759,.T.);
#16912=ADVANCED_FACE('',(#2741),#652,.T.);
#16913=ADVANCED_FACE('',(#2742),#361,.T.);
#16914=ADVANCED_FACE('',(#2743),#362,.T.);
#16915=ADVANCED_FACE('',(#2744),#653,.T.);
#16916=ADVANCED_FACE('',(#2745),#654,.T.);
#16917=ADVANCED_FACE('',(#2746),#655,.T.);
#16918=ADVANCED_FACE('',(#2747),#656,.T.);
#16919=ADVANCED_FACE('',(#2748),#657,.T.);
#16920=ADVANCED_FACE('',(#2749),#658,.T.);
#16921=ADVANCED_FACE('',(#2750),#363,.T.);
#16922=ADVANCED_FACE('',(#2751,#562),#15956,.T.);
#16923=ADVANCED_FACE('',(#2752),#15957,.T.);
#16924=ADVANCED_FACE('',(#2753),#15958,.T.);
#16925=ADVANCED_FACE('',(#2754),#15959,.T.);
#16926=ADVANCED_FACE('',(#2755),#15960,.T.);
#16927=ADVANCED_FACE('',(#2756),#15961,.T.);
#16928=ADVANCED_FACE('',(#2757),#15962,.T.);
#16929=ADVANCED_FACE('',(#2758),#364,.T.);
#16930=ADVANCED_FACE('',(#2759),#15963,.T.);
#16931=ADVANCED_FACE('',(#2760),#365,.T.);
#16932=ADVANCED_FACE('',(#2761),#15964,.T.);
#16933=ADVANCED_FACE('',(#2762),#15965,.T.);
#16934=ADVANCED_FACE('',(#2763),#366,.T.);
#16935=ADVANCED_FACE('',(#2764),#15966,.T.);
#16936=ADVANCED_FACE('',(#2765),#15967,.T.);
#16937=ADVANCED_FACE('',(#2766),#15968,.T.);
#16938=ADVANCED_FACE('',(#2767),#15969,.T.);
#16939=ADVANCED_FACE('',(#2768),#15970,.T.);
#16940=ADVANCED_FACE('',(#2769),#15971,.T.);
#16941=ADVANCED_FACE('',(#2770),#659,.T.);
#16942=ADVANCED_FACE('',(#2771),#660,.F.);
#16943=ADVANCED_FACE('',(#2772),#1760,.F.);
#16944=ADVANCED_FACE('',(#2773),#661,.F.);
#16945=ADVANCED_FACE('',(#2774),#15972,.T.);
#16946=ADVANCED_FACE('',(#2775),#15973,.T.);
#16947=ADVANCED_FACE('',(#2776),#15974,.T.);
#16948=ADVANCED_FACE('',(#2777,#563),#15975,.F.);
#16949=CLOSED_SHELL('',(#15976,#15977,#15978,#15979,#15980,#15981,#15982,
#15983,#15984,#15985,#15986,#15987,#15988,#15989,#15990,#15991,#15992,#15993,
#15994,#15995,#15996,#15997,#15998,#15999,#16000,#16001,#16002,#16003,#16004,
#16005,#16006,#16007,#16008,#16009,#16010,#16011,#16012,#16013,#16014,#16015,
#16016,#16017,#16018,#16019,#16020,#16021,#16022,#16023,#16024,#16025,#16026,
#16027,#16028,#16029,#16030,#16031,#16032,#16033,#16034,#16035,#16036,#16037,
#16038,#16039,#16040,#16041,#16042,#16043,#16044,#16045,#16046,#16047,#16048,
#16049,#16050,#16051,#16052,#16053,#16054,#16055,#16056,#16057,#16058,#16059,
#16060,#16061,#16062,#16063,#16064,#16065,#16066,#16067,#16068,#16069,#16070,
#16071,#16072,#16073,#16074,#16075,#16076,#16077,#16078,#16079,#16080,#16081,
#16082,#16083,#16084,#16085,#16086,#16087,#16088,#16089,#16090,#16091,#16092,
#16093,#16094,#16095,#16096,#16097,#16098,#16099,#16100,#16101,#16102,#16103,
#16104,#16105,#16106,#16107,#16108,#16109,#16110,#16111,#16112,#16113,#16114,
#16115,#16116,#16117));
#16950=CLOSED_SHELL('',(#16118,#16119,#16120,#16121,#16122,#16123,#16124,
#16125,#16126,#16127,#16128,#16129,#16130,#16131,#16132,#16133,#16134,#16135,
#16136,#16137,#16138,#16139));
#16951=CLOSED_SHELL('',(#16140,#16141,#16142,#16143,#16144,#16145,#16146,
#16147,#16148,#16149,#16150,#16151,#16152,#16153,#16154,#16155,#16156,#16157,
#16158,#16159,#16160,#16161));
#16952=CLOSED_SHELL('',(#16162,#16163,#16164,#16165,#16166,#16167,#16168,
#16169,#16170,#16171));
#16953=CLOSED_SHELL('',(#16172,#16173,#16174,#16175,#16176,#16177,#16178,
#16179,#16180,#16181,#16182,#16183,#16184,#16185));
#16954=CLOSED_SHELL('',(#16186,#16187,#16188,#16189,#16190,#16191));
#16955=CLOSED_SHELL('',(#16192,#16193,#16194,#16195,#16196,#16197,#16198,
#16199));
#16956=CLOSED_SHELL('',(#16200,#16201,#16202,#16203,#16204,#16205,#16206,
#16207,#16208,#16209,#16210,#16211,#16212,#16213,#16214,#16215,#16216,#16217,
#16218,#16219,#16220,#16221,#16222,#16223,#16224,#16225,#16226,#16227,#16228,
#16229,#16230,#16231,#16232,#16233,#16234,#16235,#16236,#16237,#16238,#16239,
#16240,#16241,#16242,#16243,#16244,#16245,#16246,#16247,#16248,#16249,#16250,
#16251,#16252,#16253,#16254,#16255,#16256,#16257,#16258,#16259,#16260,#16261,
#16262,#16263,#16264,#16265,#16266,#16267,#16268,#16269,#16270,#16271,#16272,
#16273,#16274,#16275,#16276));
#16957=CLOSED_SHELL('',(#16277,#16278,#16279,#16280,#16281,#16282,#16283,
#16284,#16285,#16286,#16287,#16288,#16289,#16290,#16291,#16292,#16293,#16294,
#16295,#16296,#16297,#16298,#16299,#16300,#16301,#16302,#16303,#16304,#16305,
#16306,#16307,#16308,#16309,#16310,#16311,#16312,#16313));
#16958=CLOSED_SHELL('',(#16314,#16315,#16316,#16317,#16318,#16319,#16320,
#16321,#16322,#16323,#16324,#16325,#16326,#16327,#16328,#16329,#16330,#16331,
#16332,#16333,#16334,#16335,#16336,#16337,#16338,#16339,#16340,#16341,#16342,
#16343,#16344,#16345,#16346,#16347,#16348,#16349,#16350,#16351,#16352,#16353,
#16354,#16355,#16356,#16357,#16358,#16359,#16360,#16361,#16362,#16363,#16364,
#16365,#16366,#16367,#16368,#16369,#16370,#16371,#16372,#16373,#16374,#16375,
#16376,#16377,#16378,#16379,#16380,#16381,#16382,#16383,#16384,#16385,#16386,
#16387,#16388,#16389,#16390,#16391,#16392,#16393,#16394,#16395));
#16959=CLOSED_SHELL('',(#16396,#16397,#16398,#16399,#16400,#16401,#16402,
#16403,#16404,#16405,#16406,#16407,#16408,#16409,#16410,#16411,#16412,#16413,
#16414,#16415,#16416,#16417,#16418,#16419,#16420,#16421,#16422,#16423,#16424,
#16425,#16426,#16427,#16428,#16429,#16430,#16431,#16432,#16433,#16434));
#16960=CLOSED_SHELL('',(#16435,#16436,#16437,#16438,#16439,#16440,#16441,
#16442,#16443,#16444,#16445,#16446,#16447,#16448,#16449,#16450,#16451,#16452,
#16453,#16454,#16455,#16456,#16457,#16458,#16459,#16460,#16461,#16462,#16463,
#16464,#16465,#16466,#16467,#16468,#16469,#16470,#16471,#16472));
#16961=CLOSED_SHELL('',(#16473,#16474,#16475,#16476,#16477,#16478,#16479,
#16480,#16481,#16482,#16483,#16484,#16485,#16486,#16487,#16488,#16489,#16490,
#16491,#16492,#16493,#16494,#16495,#16496,#16497,#16498,#16499,#16500,#16501,
#16502,#16503,#16504,#16505,#16506,#16507,#16508,#16509,#16510,#16511,#16512,
#16513,#16514,#16515));
#16962=CLOSED_SHELL('',(#16516));
#16963=CLOSED_SHELL('',(#16517,#16518,#16519,#16520,#16521,#16522));
#16964=CLOSED_SHELL('',(#16523,#16524,#16525,#16526,#16527,#16528,#16529,
#16530,#16531,#16532,#16533,#16534,#16535,#16536,#16537,#16538,#16539,#16540,
#16541,#16542,#16543,#16544,#16545,#16546,#16547,#16548,#16549,#16550,#16551,
#16552,#16553,#16554,#16555,#16556,#16557,#16558,#16559,#16560,#16561,#16562,
#16563,#16564,#16565,#16566,#16567,#16568,#16569,#16570,#16571,#16572,#16573,
#16574,#16575,#16576,#16577,#16578,#16579,#16580,#16581,#16582));
#16965=CLOSED_SHELL('',(#16583,#16584,#16585,#16586,#16587,#16588,#16589,
#16590,#16591,#16592,#16593,#16594,#16595,#16596,#16597,#16598,#16599,#16600,
#16601,#16602,#16603,#16604,#16605,#16606,#16607,#16608,#16609,#16610,#16611,
#16612,#16613,#16614,#16615));
#16966=CLOSED_SHELL('',(#16616,#16617,#16618,#16619,#16620,#16621,#16622,
#16623,#16624,#16625,#16626,#16627,#16628,#16629,#16630,#16631,#16632,#16633,
#16634,#16635,#16636,#16637,#16638,#16639,#16640,#16641,#16642,#16643,#16644,
#16645,#16646,#16647,#16648,#16649,#16650,#16651,#16652,#16653,#16654,#16655,
#16656,#16657,#16658,#16659,#16660,#16661,#16662,#16663,#16664,#16665,#16666,
#16667,#16668,#16669,#16670,#16671,#16672,#16673,#16674,#16675,#16676,#16677,
#16678,#16679,#16680,#16681,#16682,#16683,#16684,#16685,#16686,#16687,#16688,
#16689,#16690,#16691,#16692,#16693,#16694,#16695,#16696,#16697,#16698,#16699,
#16700,#16701,#16702,#16703,#16704,#16705,#16706,#16707,#16708,#16709,#16710,
#16711,#16712,#16713,#16714,#16715,#16716,#16717,#16718,#16719));
#16967=CLOSED_SHELL('',(#16720,#16721,#16722,#16723,#16724,#16725,#16726,
#16727,#16728,#16729,#16730,#16731,#16732,#16733,#16734,#16735,#16736,#16737,
#16738,#16739,#16740,#16741,#16742,#16743,#16744,#16745,#16746,#16747,#16748,
#16749,#16750,#16751,#16752,#16753,#16754,#16755,#16756,#16757,#16758,#16759,
#16760,#16761,#16762,#16763,#16764,#16765,#16766,#16767,#16768,#16769,#16770,
#16771,#16772,#16773,#16774,#16775,#16776,#16777,#16778,#16779,#16780,#16781,
#16782,#16783,#16784,#16785,#16786,#16787,#16788,#16789,#16790,#16791,#16792,
#16793,#16794,#16795,#16796,#16797,#16798,#16799,#16800,#16801,#16802,#16803,
#16804,#16805,#16806,#16807,#16808,#16809,#16810,#16811,#16812,#16813,#16814,
#16815,#16816,#16817,#16818,#16819,#16820,#16821,#16822,#16823,#16824,#16825,
#16826,#16827,#16828,#16829,#16830,#16831,#16832,#16833,#16834,#16835,#16836,
#16837,#16838,#16839,#16840,#16841,#16842,#16843,#16844,#16845,#16846,#16847,
#16848,#16849,#16850,#16851,#16852,#16853,#16854,#16855,#16856,#16857,#16858,
#16859,#16860,#16861,#16862,#16863,#16864,#16865,#16866,#16867,#16868,#16869,
#16870,#16871,#16872,#16873,#16874,#16875,#16876,#16877,#16878,#16879,#16880,
#16881,#16882,#16883,#16884,#16885,#16886,#16887,#16888,#16889,#16890,#16891,
#16892,#16893,#16894,#16895,#16896,#16897,#16898,#16899,#16900,#16901,#16902,
#16903,#16904,#16905,#16906,#16907,#16908,#16909,#16910,#16911));
#16968=CLOSED_SHELL('',(#16912,#16913,#16914,#16915,#16916,#16917,#16918,
#16919,#16920,#16921,#16922,#16923,#16924,#16925,#16926,#16927,#16928,#16929,
#16930,#16931,#16932,#16933,#16934,#16935,#16936,#16937,#16938,#16939,#16940,
#16941,#16942,#16943,#16944,#16945,#16946,#16947,#16948));
#16969=DERIVED_UNIT_ELEMENT(#17009,1.);
#16970=DERIVED_UNIT_ELEMENT(#56641,-3.);
#16971=DERIVED_UNIT_ELEMENT(#17009,1.);
#16972=DERIVED_UNIT_ELEMENT(#56641,-3.);
#16973=DERIVED_UNIT_ELEMENT(#17009,1.);
#16974=DERIVED_UNIT_ELEMENT(#56641,-3.);
#16975=DERIVED_UNIT_ELEMENT(#17009,1.);
#16976=DERIVED_UNIT_ELEMENT(#56641,-3.);
#16977=DERIVED_UNIT_ELEMENT(#17009,1.);
#16978=DERIVED_UNIT_ELEMENT(#56641,-3.);
#16979=DERIVED_UNIT_ELEMENT(#17009,1.);
#16980=DERIVED_UNIT_ELEMENT(#56641,-3.);
#16981=DERIVED_UNIT_ELEMENT(#17009,1.);
#16982=DERIVED_UNIT_ELEMENT(#56641,-3.);
#16983=DERIVED_UNIT_ELEMENT(#17009,1.);
#16984=DERIVED_UNIT_ELEMENT(#56641,-3.);
#16985=DERIVED_UNIT_ELEMENT(#17009,1.);
#16986=DERIVED_UNIT_ELEMENT(#56641,-3.);
#16987=DERIVED_UNIT_ELEMENT(#17009,1.);
#16988=DERIVED_UNIT_ELEMENT(#56641,-3.);
#16989=DERIVED_UNIT_ELEMENT(#17009,1.);
#16990=DERIVED_UNIT_ELEMENT(#56641,-3.);
#16991=DERIVED_UNIT_ELEMENT(#17009,1.);
#16992=DERIVED_UNIT_ELEMENT(#56641,-3.);
#16993=DERIVED_UNIT_ELEMENT(#17009,1.);
#16994=DERIVED_UNIT_ELEMENT(#56641,-3.);
#16995=DERIVED_UNIT_ELEMENT(#17009,1.);
#16996=DERIVED_UNIT_ELEMENT(#56641,-3.);
#16997=DERIVED_UNIT_ELEMENT(#17009,1.);
#16998=DERIVED_UNIT_ELEMENT(#56641,-3.);
#16999=DERIVED_UNIT_ELEMENT(#17009,1.);
#17000=DERIVED_UNIT_ELEMENT(#56641,-3.);
#17001=DERIVED_UNIT_ELEMENT(#17009,1.);
#17002=DERIVED_UNIT_ELEMENT(#56641,-3.);
#17003=DERIVED_UNIT_ELEMENT(#17009,1.);
#17004=DERIVED_UNIT_ELEMENT(#56641,-3.);
#17005=DERIVED_UNIT_ELEMENT(#17009,1.);
#17006=DERIVED_UNIT_ELEMENT(#56641,-3.);
#17007=DERIVED_UNIT_ELEMENT(#17009,1.);
#17008=DERIVED_UNIT_ELEMENT(#56641,-3.);
#17009=(
MASS_UNIT()
NAMED_UNIT(*)
SI_UNIT(.KILO.,.GRAM.)
);
#17010=DERIVED_UNIT((#16969,#16970));
#17011=DERIVED_UNIT((#16971,#16972));
#17012=DERIVED_UNIT((#16973,#16974));
#17013=DERIVED_UNIT((#16975,#16976));
#17014=DERIVED_UNIT((#16977,#16978));
#17015=DERIVED_UNIT((#16979,#16980));
#17016=DERIVED_UNIT((#16981,#16982));
#17017=DERIVED_UNIT((#16983,#16984));
#17018=DERIVED_UNIT((#16985,#16986));
#17019=DERIVED_UNIT((#16987,#16988));
#17020=DERIVED_UNIT((#16989,#16990));
#17021=DERIVED_UNIT((#16991,#16992));
#17022=DERIVED_UNIT((#16993,#16994));
#17023=DERIVED_UNIT((#16995,#16996));
#17024=DERIVED_UNIT((#16997,#16998));
#17025=DERIVED_UNIT((#16999,#17000));
#17026=DERIVED_UNIT((#17001,#17002));
#17027=DERIVED_UNIT((#17003,#17004));
#17028=DERIVED_UNIT((#17005,#17006));
#17029=DERIVED_UNIT((#17007,#17008));
#17030=MEASURE_REPRESENTATION_ITEM('density measure',
POSITIVE_RATIO_MEASURE(7850.),#17010);
#17031=MEASURE_REPRESENTATION_ITEM('density measure',
POSITIVE_RATIO_MEASURE(7850.),#17011);
#17032=MEASURE_REPRESENTATION_ITEM('density measure',
POSITIVE_RATIO_MEASURE(7850.),#17012);
#17033=MEASURE_REPRESENTATION_ITEM('density measure',
POSITIVE_RATIO_MEASURE(7850.),#17013);
#17034=MEASURE_REPRESENTATION_ITEM('density measure',
POSITIVE_RATIO_MEASURE(7850.),#17014);
#17035=MEASURE_REPRESENTATION_ITEM('density measure',
POSITIVE_RATIO_MEASURE(7850.),#17015);
#17036=MEASURE_REPRESENTATION_ITEM('density measure',
POSITIVE_RATIO_MEASURE(7850.),#17016);
#17037=MEASURE_REPRESENTATION_ITEM('density measure',
POSITIVE_RATIO_MEASURE(7850.),#17017);
#17038=MEASURE_REPRESENTATION_ITEM('density measure',
POSITIVE_RATIO_MEASURE(7850.),#17018);
#17039=MEASURE_REPRESENTATION_ITEM('density measure',
POSITIVE_RATIO_MEASURE(7850.),#17019);
#17040=MEASURE_REPRESENTATION_ITEM('density measure',
POSITIVE_RATIO_MEASURE(7850.),#17020);
#17041=MEASURE_REPRESENTATION_ITEM('density measure',
POSITIVE_RATIO_MEASURE(7850.),#17021);
#17042=MEASURE_REPRESENTATION_ITEM('density measure',
POSITIVE_RATIO_MEASURE(7850.),#17022);
#17043=MEASURE_REPRESENTATION_ITEM('density measure',
POSITIVE_RATIO_MEASURE(7850.),#17023);
#17044=MEASURE_REPRESENTATION_ITEM('density measure',
POSITIVE_RATIO_MEASURE(7850.),#17024);
#17045=MEASURE_REPRESENTATION_ITEM('density measure',
POSITIVE_RATIO_MEASURE(7850.),#17025);
#17046=MEASURE_REPRESENTATION_ITEM('density measure',
POSITIVE_RATIO_MEASURE(7850.),#17026);
#17047=MEASURE_REPRESENTATION_ITEM('density measure',
POSITIVE_RATIO_MEASURE(7850.),#17027);
#17048=MEASURE_REPRESENTATION_ITEM('density measure',
POSITIVE_RATIO_MEASURE(7850.),#17028);
#17049=MEASURE_REPRESENTATION_ITEM('density measure',
POSITIVE_RATIO_MEASURE(7850.),#17029);
#17050=PROPERTY_DEFINITION_REPRESENTATION(#17150,#17090);
#17051=PROPERTY_DEFINITION_REPRESENTATION(#17151,#17091);
#17052=PROPERTY_DEFINITION_REPRESENTATION(#17152,#17092);
#17053=PROPERTY_DEFINITION_REPRESENTATION(#17153,#17093);
#17054=PROPERTY_DEFINITION_REPRESENTATION(#17154,#17094);
#17055=PROPERTY_DEFINITION_REPRESENTATION(#17155,#17095);
#17056=PROPERTY_DEFINITION_REPRESENTATION(#17156,#17096);
#17057=PROPERTY_DEFINITION_REPRESENTATION(#17157,#17097);
#17058=PROPERTY_DEFINITION_REPRESENTATION(#17158,#17098);
#17059=PROPERTY_DEFINITION_REPRESENTATION(#17159,#17099);
#17060=PROPERTY_DEFINITION_REPRESENTATION(#17160,#17100);
#17061=PROPERTY_DEFINITION_REPRESENTATION(#17161,#17101);
#17062=PROPERTY_DEFINITION_REPRESENTATION(#17162,#17102);
#17063=PROPERTY_DEFINITION_REPRESENTATION(#17163,#17103);
#17064=PROPERTY_DEFINITION_REPRESENTATION(#17164,#17104);
#17065=PROPERTY_DEFINITION_REPRESENTATION(#17165,#17105);
#17066=PROPERTY_DEFINITION_REPRESENTATION(#17166,#17106);
#17067=PROPERTY_DEFINITION_REPRESENTATION(#17167,#17107);
#17068=PROPERTY_DEFINITION_REPRESENTATION(#17168,#17108);
#17069=PROPERTY_DEFINITION_REPRESENTATION(#17169,#17109);
#17070=PROPERTY_DEFINITION_REPRESENTATION(#17170,#17110);
#17071=PROPERTY_DEFINITION_REPRESENTATION(#17171,#17111);
#17072=PROPERTY_DEFINITION_REPRESENTATION(#17172,#17112);
#17073=PROPERTY_DEFINITION_REPRESENTATION(#17173,#17113);
#17074=PROPERTY_DEFINITION_REPRESENTATION(#17174,#17114);
#17075=PROPERTY_DEFINITION_REPRESENTATION(#17175,#17115);
#17076=PROPERTY_DEFINITION_REPRESENTATION(#17176,#17116);
#17077=PROPERTY_DEFINITION_REPRESENTATION(#17177,#17117);
#17078=PROPERTY_DEFINITION_REPRESENTATION(#17178,#17118);
#17079=PROPERTY_DEFINITION_REPRESENTATION(#17179,#17119);
#17080=PROPERTY_DEFINITION_REPRESENTATION(#17180,#17120);
#17081=PROPERTY_DEFINITION_REPRESENTATION(#17181,#17121);
#17082=PROPERTY_DEFINITION_REPRESENTATION(#17182,#17122);
#17083=PROPERTY_DEFINITION_REPRESENTATION(#17183,#17123);
#17084=PROPERTY_DEFINITION_REPRESENTATION(#17184,#17124);
#17085=PROPERTY_DEFINITION_REPRESENTATION(#17185,#17125);
#17086=PROPERTY_DEFINITION_REPRESENTATION(#17186,#17126);
#17087=PROPERTY_DEFINITION_REPRESENTATION(#17187,#17127);
#17088=PROPERTY_DEFINITION_REPRESENTATION(#17188,#17128);
#17089=PROPERTY_DEFINITION_REPRESENTATION(#17189,#17129);
#17090=REPRESENTATION('material name',(#17130),#56619);
#17091=REPRESENTATION('density',(#17030),#56619);
#17092=REPRESENTATION('material name',(#17131),#56620);
#17093=REPRESENTATION('density',(#17031),#56620);
#17094=REPRESENTATION('material name',(#17132),#56621);
#17095=REPRESENTATION('density',(#17032),#56621);
#17096=REPRESENTATION('material name',(#17133),#56622);
#17097=REPRESENTATION('density',(#17033),#56622);
#17098=REPRESENTATION('material name',(#17134),#56623);
#17099=REPRESENTATION('density',(#17034),#56623);
#17100=REPRESENTATION('material name',(#17135),#56624);
#17101=REPRESENTATION('density',(#17035),#56624);
#17102=REPRESENTATION('material name',(#17136),#56625);
#17103=REPRESENTATION('density',(#17036),#56625);
#17104=REPRESENTATION('material name',(#17137),#56626);
#17105=REPRESENTATION('density',(#17037),#56626);
#17106=REPRESENTATION('material name',(#17138),#56627);
#17107=REPRESENTATION('density',(#17038),#56627);
#17108=REPRESENTATION('material name',(#17139),#56628);
#17109=REPRESENTATION('density',(#17039),#56628);
#17110=REPRESENTATION('material name',(#17140),#56629);
#17111=REPRESENTATION('density',(#17040),#56629);
#17112=REPRESENTATION('material name',(#17141),#56630);
#17113=REPRESENTATION('density',(#17041),#56630);
#17114=REPRESENTATION('material name',(#17142),#56631);
#17115=REPRESENTATION('density',(#17042),#56631);
#17116=REPRESENTATION('material name',(#17143),#56632);
#17117=REPRESENTATION('density',(#17043),#56632);
#17118=REPRESENTATION('material name',(#17144),#56633);
#17119=REPRESENTATION('density',(#17044),#56633);
#17120=REPRESENTATION('material name',(#17145),#56634);
#17121=REPRESENTATION('density',(#17045),#56634);
#17122=REPRESENTATION('material name',(#17146),#56635);
#17123=REPRESENTATION('density',(#17046),#56635);
#17124=REPRESENTATION('material name',(#17147),#56636);
#17125=REPRESENTATION('density',(#17047),#56636);
#17126=REPRESENTATION('material name',(#17148),#56637);
#17127=REPRESENTATION('density',(#17048),#56637);
#17128=REPRESENTATION('material name',(#17149),#56638);
#17129=REPRESENTATION('density',(#17049),#56638);
#17130=DESCRIPTIVE_REPRESENTATION_ITEM('Steel','Steel');
#17131=DESCRIPTIVE_REPRESENTATION_ITEM('Steel','Steel');
#17132=DESCRIPTIVE_REPRESENTATION_ITEM('Steel','Steel');
#17133=DESCRIPTIVE_REPRESENTATION_ITEM('Steel','Steel');
#17134=DESCRIPTIVE_REPRESENTATION_ITEM('Steel','Steel');
#17135=DESCRIPTIVE_REPRESENTATION_ITEM('Steel','Steel');
#17136=DESCRIPTIVE_REPRESENTATION_ITEM('Steel','Steel');
#17137=DESCRIPTIVE_REPRESENTATION_ITEM('Steel','Steel');
#17138=DESCRIPTIVE_REPRESENTATION_ITEM('Steel','Steel');
#17139=DESCRIPTIVE_REPRESENTATION_ITEM('Steel','Steel');
#17140=DESCRIPTIVE_REPRESENTATION_ITEM('Steel','Steel');
#17141=DESCRIPTIVE_REPRESENTATION_ITEM('Steel','Steel');
#17142=DESCRIPTIVE_REPRESENTATION_ITEM('Steel','Steel');
#17143=DESCRIPTIVE_REPRESENTATION_ITEM('Steel','Steel');
#17144=DESCRIPTIVE_REPRESENTATION_ITEM('Steel','Steel');
#17145=DESCRIPTIVE_REPRESENTATION_ITEM('Steel','Steel');
#17146=DESCRIPTIVE_REPRESENTATION_ITEM('Steel','Steel');
#17147=DESCRIPTIVE_REPRESENTATION_ITEM('Steel','Steel');
#17148=DESCRIPTIVE_REPRESENTATION_ITEM('Steel','Steel');
#17149=DESCRIPTIVE_REPRESENTATION_ITEM('Steel','Steel');
#17150=PROPERTY_DEFINITION('material property','material name',#56767);
#17151=PROPERTY_DEFINITION('material property','density of part',#56767);
#17152=PROPERTY_DEFINITION('material property','material name',#56768);
#17153=PROPERTY_DEFINITION('material property','density of part',#56768);
#17154=PROPERTY_DEFINITION('material property','material name',#56769);
#17155=PROPERTY_DEFINITION('material property','density of part',#56769);
#17156=PROPERTY_DEFINITION('material property','material name',#56770);
#17157=PROPERTY_DEFINITION('material property','density of part',#56770);
#17158=PROPERTY_DEFINITION('material property','material name',#56771);
#17159=PROPERTY_DEFINITION('material property','density of part',#56771);
#17160=PROPERTY_DEFINITION('material property','material name',#56772);
#17161=PROPERTY_DEFINITION('material property','density of part',#56772);
#17162=PROPERTY_DEFINITION('material property','material name',#56773);
#17163=PROPERTY_DEFINITION('material property','density of part',#56773);
#17164=PROPERTY_DEFINITION('material property','material name',#56774);
#17165=PROPERTY_DEFINITION('material property','density of part',#56774);
#17166=PROPERTY_DEFINITION('material property','material name',#56775);
#17167=PROPERTY_DEFINITION('material property','density of part',#56775);
#17168=PROPERTY_DEFINITION('material property','material name',#56776);
#17169=PROPERTY_DEFINITION('material property','density of part',#56776);
#17170=PROPERTY_DEFINITION('material property','material name',#56777);
#17171=PROPERTY_DEFINITION('material property','density of part',#56777);
#17172=PROPERTY_DEFINITION('material property','material name',#56778);
#17173=PROPERTY_DEFINITION('material property','density of part',#56778);
#17174=PROPERTY_DEFINITION('material property','material name',#56779);
#17175=PROPERTY_DEFINITION('material property','density of part',#56779);
#17176=PROPERTY_DEFINITION('material property','material name',#56780);
#17177=PROPERTY_DEFINITION('material property','density of part',#56780);
#17178=PROPERTY_DEFINITION('material property','material name',#56781);
#17179=PROPERTY_DEFINITION('material property','density of part',#56781);
#17180=PROPERTY_DEFINITION('material property','material name',#56782);
#17181=PROPERTY_DEFINITION('material property','density of part',#56782);
#17182=PROPERTY_DEFINITION('material property','material name',#56783);
#17183=PROPERTY_DEFINITION('material property','density of part',#56783);
#17184=PROPERTY_DEFINITION('material property','material name',#56784);
#17185=PROPERTY_DEFINITION('material property','density of part',#56784);
#17186=PROPERTY_DEFINITION('material property','material name',#56785);
#17187=PROPERTY_DEFINITION('material property','density of part',#56785);
#17188=PROPERTY_DEFINITION('material property','material name',#56786);
#17189=PROPERTY_DEFINITION('material property','density of part',#56786);
#17190=AXIS2_PLACEMENT_3D('',#22941,#18789,#18790);
#17191=AXIS2_PLACEMENT_3D('',#22942,#18791,#18792);
#17192=AXIS2_PLACEMENT_3D('',#22943,#18793,#18794);
#17193=AXIS2_PLACEMENT_3D('',#22959,#18798,#18799);
#17194=AXIS2_PLACEMENT_3D('',#22993,#18806,#18807);
#17195=AXIS2_PLACEMENT_3D('',#23006,#18810,#18811);
#17196=AXIS2_PLACEMENT_3D('',#23008,#18812,#18813);
#17197=AXIS2_PLACEMENT_3D('',#23011,#18815,#18816);
#17198=AXIS2_PLACEMENT_3D('',#23012,#18817,#18818);
#17199=AXIS2_PLACEMENT_3D('',#23013,#18819,#18820);
#17200=AXIS2_PLACEMENT_3D('',#23014,#18821,#18822);
#17201=AXIS2_PLACEMENT_3D('',#23030,#18826,#18827);
#17202=AXIS2_PLACEMENT_3D('',#23064,#18834,#18835);
#17203=AXIS2_PLACEMENT_3D('',#23077,#18838,#18839);
#17204=AXIS2_PLACEMENT_3D('',#23079,#18840,#18841);
#17205=AXIS2_PLACEMENT_3D('',#23082,#18843,#18844);
#17206=AXIS2_PLACEMENT_3D('',#23083,#18845,#18846);
#17207=AXIS2_PLACEMENT_3D('',#23084,#18847,#18848);
#17208=AXIS2_PLACEMENT_3D('',#23085,#18849,#18850);
#17209=AXIS2_PLACEMENT_3D('',#23087,#18851,#18852);
#17210=AXIS2_PLACEMENT_3D('',#23089,#18854,#18855);
#17211=AXIS2_PLACEMENT_3D('',#23092,#18856,#18857);
#17212=AXIS2_PLACEMENT_3D('',#23096,#18859,#18860);
#17213=AXIS2_PLACEMENT_3D('',#23100,#18862,#18863);
#17214=AXIS2_PLACEMENT_3D('',#23104,#18865,#18866);
#17215=AXIS2_PLACEMENT_3D('',#23107,#18868,#18869);
#17216=AXIS2_PLACEMENT_3D('',#23109,#18870,#18871);
#17217=AXIS2_PLACEMENT_3D('',#23110,#18872,#18873);
#17218=AXIS2_PLACEMENT_3D('',#23112,#18875,#18876);
#17219=AXIS2_PLACEMENT_3D('',#23114,#18877,#18878);
#17220=AXIS2_PLACEMENT_3D('',#23117,#18880,#18881);
#17221=AXIS2_PLACEMENT_3D('',#23118,#18882,#18883);
#17222=AXIS2_PLACEMENT_3D('',#23123,#18885,#18886);
#17223=AXIS2_PLACEMENT_3D('',#23127,#18888,#18889);
#17224=AXIS2_PLACEMENT_3D('',#23131,#18891,#18892);
#17225=AXIS2_PLACEMENT_3D('',#23134,#18894,#18895);
#17226=AXIS2_PLACEMENT_3D('',#23136,#18896,#18897);
#17227=AXIS2_PLACEMENT_3D('',#23138,#18898,#18899);
#17228=AXIS2_PLACEMENT_3D('',#23139,#18900,#18901);
#17229=AXIS2_PLACEMENT_3D('',#23142,#18903,#18904);
#17230=AXIS2_PLACEMENT_3D('',#23143,#18905,#18906);
#17231=AXIS2_PLACEMENT_3D('',#23146,#18908,#18909);
#17232=AXIS2_PLACEMENT_3D('',#23147,#18910,#18911);
#17233=AXIS2_PLACEMENT_3D('',#23150,#18913,#18914);
#17234=AXIS2_PLACEMENT_3D('',#23151,#18915,#18916);
#17235=AXIS2_PLACEMENT_3D('',#23163,#18917,#18918);
#17236=AXIS2_PLACEMENT_3D('',#23173,#18919,#18920);
#17237=AXIS2_PLACEMENT_3D('',#23174,#18921,#18922);
#17238=AXIS2_PLACEMENT_3D('',#23187,#18923,#18924);
#17239=AXIS2_PLACEMENT_3D('',#23203,#18925,#18926);
#17240=AXIS2_PLACEMENT_3D('',#23215,#18927,#18928);
#17241=AXIS2_PLACEMENT_3D('',#23226,#18929,#18930);
#17242=AXIS2_PLACEMENT_3D('',#23227,#18931,#18932);
#17243=AXIS2_PLACEMENT_3D('',#23228,#18933,#18934);
#17244=AXIS2_PLACEMENT_3D('',#23246,#18935,#18936);
#17245=AXIS2_PLACEMENT_3D('',#23257,#18937,#18938);
#17246=AXIS2_PLACEMENT_3D('',#23259,#18939,#18940);
#17247=AXIS2_PLACEMENT_3D('',#23261,#18941,#18942);
#17248=AXIS2_PLACEMENT_3D('',#23263,#18943,#18944);
#17249=AXIS2_PLACEMENT_3D('',#23264,#18945,#18946);
#17250=AXIS2_PLACEMENT_3D('',#23265,#18947,#18948);
#17251=AXIS2_PLACEMENT_3D('',#23284,#18950,#18951);
#17252=AXIS2_PLACEMENT_3D('',#23315,#18952,#18953);
#17253=AXIS2_PLACEMENT_3D('',#23331,#18954,#18955);
#17254=AXIS2_PLACEMENT_3D('',#23380,#18980,#18981);
#17255=AXIS2_PLACEMENT_3D('',#23394,#18982,#18983);
#17256=AXIS2_PLACEMENT_3D('',#23411,#18984,#18985);
#17257=AXIS2_PLACEMENT_3D('',#23412,#18986,#18987);
#17258=AXIS2_PLACEMENT_3D('',#23434,#18992,#18993);
#17259=AXIS2_PLACEMENT_3D('',#23436,#18994,#18995);
#17260=AXIS2_PLACEMENT_3D('',#23438,#18996,#18997);
#17261=AXIS2_PLACEMENT_3D('',#23439,#18998,#18999);
#17262=AXIS2_PLACEMENT_3D('',#23450,#19000,#19001);
#17263=AXIS2_PLACEMENT_3D('',#23452,#19002,#19003);
#17264=AXIS2_PLACEMENT_3D('',#23459,#19004,#19005);
#17265=AXIS2_PLACEMENT_3D('',#23473,#19006,#19007);
#17266=AXIS2_PLACEMENT_3D('',#23487,#19008,#19009);
#17267=AXIS2_PLACEMENT_3D('',#23496,#19010,#19011);
#17268=AXIS2_PLACEMENT_3D('',#23505,#19013,#19014);
#17269=AXIS2_PLACEMENT_3D('',#23506,#19015,#19016);
#17270=AXIS2_PLACEMENT_3D('',#23514,#19017,#19018);
#17271=AXIS2_PLACEMENT_3D('',#23527,#19019,#19020);
#17272=AXIS2_PLACEMENT_3D('',#23536,#19021,#19022);
#17273=AXIS2_PLACEMENT_3D('',#23558,#19027,#19028);
#17274=AXIS2_PLACEMENT_3D('',#23560,#19029,#19030);
#17275=AXIS2_PLACEMENT_3D('',#23562,#19031,#19032);
#17276=AXIS2_PLACEMENT_3D('',#23563,#19033,#19034);
#17277=AXIS2_PLACEMENT_3D('',#23580,#19035,#19036);
#17278=AXIS2_PLACEMENT_3D('',#23582,#19037,#19038);
#17279=AXIS2_PLACEMENT_3D('',#23583,#19039,#19040);
#17280=AXIS2_PLACEMENT_3D('',#23584,#19041,#19042);
#17281=AXIS2_PLACEMENT_3D('',#23586,#19043,#19044);
#17282=AXIS2_PLACEMENT_3D('',#23588,#19045,#19046);
#17283=AXIS2_PLACEMENT_3D('',#23590,#19047,#19048);
#17284=AXIS2_PLACEMENT_3D('',#23592,#19049,#19050);
#17285=AXIS2_PLACEMENT_3D('',#23594,#19051,#19052);
#17286=AXIS2_PLACEMENT_3D('',#23596,#19053,#19054);
#17287=AXIS2_PLACEMENT_3D('',#23598,#19055,#19056);
#17288=AXIS2_PLACEMENT_3D('',#23599,#19057,#19058);
#17289=AXIS2_PLACEMENT_3D('',#23601,#19059,#19060);
#17290=AXIS2_PLACEMENT_3D('',#23603,#19061,#19062);
#17291=AXIS2_PLACEMENT_3D('',#23604,#19063,#19064);
#17292=AXIS2_PLACEMENT_3D('',#23605,#19065,#19066);
#17293=AXIS2_PLACEMENT_3D('',#23608,#19067,#19068);
#17294=AXIS2_PLACEMENT_3D('',#23611,#19071,#19072);
#17295=AXIS2_PLACEMENT_3D('',#23614,#19073,#19074);
#17296=AXIS2_PLACEMENT_3D('',#23615,#19075,#19076);
#17297=AXIS2_PLACEMENT_3D('',#23616,#19077,#19078);
#17298=AXIS2_PLACEMENT_3D('',#23617,#19079,#19080);
#17299=AXIS2_PLACEMENT_3D('',#23628,#19083,#19084);
#17300=AXIS2_PLACEMENT_3D('',#23639,#19091,#19092);
#17301=AXIS2_PLACEMENT_3D('',#23641,#19093,#19094);
#17302=AXIS2_PLACEMENT_3D('',#23644,#19096,#19097);
#17303=AXIS2_PLACEMENT_3D('',#23645,#19098,#19099);
#17304=AXIS2_PLACEMENT_3D('',#23646,#19100,#19101);
#17305=AXIS2_PLACEMENT_3D('',#23647,#19102,#19103);
#17306=AXIS2_PLACEMENT_3D('',#23648,#19104,#19105);
#17307=AXIS2_PLACEMENT_3D('',#23650,#19106,#19107);
#17308=AXIS2_PLACEMENT_3D('',#23651,#19108,#19109);
#17309=AXIS2_PLACEMENT_3D('',#23652,#19110,#19111);
#17310=AXIS2_PLACEMENT_3D('',#23654,#19112,#19113);
#17311=AXIS2_PLACEMENT_3D('',#23656,#19115,#19116);
#17312=AXIS2_PLACEMENT_3D('',#23658,#19117,#19118);
#17313=AXIS2_PLACEMENT_3D('',#23659,#19119,#19120);
#17314=AXIS2_PLACEMENT_3D('',#23660,#19121,#19122);
#17315=AXIS2_PLACEMENT_3D('',#23662,#19123,#19124);
#17316=AXIS2_PLACEMENT_3D('',#23664,#19126,#19127);
#17317=AXIS2_PLACEMENT_3D('',#23666,#19128,#19129);
#17318=AXIS2_PLACEMENT_3D('',#23667,#19130,#19131);
#17319=AXIS2_PLACEMENT_3D('',#23668,#19132,#19133);
#17320=AXIS2_PLACEMENT_3D('',#23670,#19134,#19135);
#17321=AXIS2_PLACEMENT_3D('',#23672,#19137,#19138);
#17322=AXIS2_PLACEMENT_3D('',#23673,#19139,#19140);
#17323=AXIS2_PLACEMENT_3D('',#23674,#19141,#19142);
#17324=AXIS2_PLACEMENT_3D('',#23677,#19144,#19145);
#17325=AXIS2_PLACEMENT_3D('',#23679,#19147,#19148);
#17326=AXIS2_PLACEMENT_3D('',#23683,#19151,#19152);
#17327=AXIS2_PLACEMENT_3D('',#23684,#19153,#19154);
#17328=AXIS2_PLACEMENT_3D('',#23685,#19155,#19156);
#17329=AXIS2_PLACEMENT_3D('',#23687,#19157,#19158);
#17330=AXIS2_PLACEMENT_3D('',#23696,#19160,#19161);
#17331=AXIS2_PLACEMENT_3D('',#23698,#19162,#19163);
#17332=AXIS2_PLACEMENT_3D('',#23701,#19165,#19166);
#17333=AXIS2_PLACEMENT_3D('',#23702,#19167,#19168);
#17334=AXIS2_PLACEMENT_3D('',#23703,#19169,#19170);
#17335=AXIS2_PLACEMENT_3D('',#23704,#19171,#19172);
#17336=AXIS2_PLACEMENT_3D('',#23705,#19173,#19174);
#17337=AXIS2_PLACEMENT_3D('',#23706,#19175,#19176);
#17338=AXIS2_PLACEMENT_3D('',#23708,#19177,#19178);
#17339=AXIS2_PLACEMENT_3D('',#23711,#19180,#19181);
#17340=AXIS2_PLACEMENT_3D('',#23712,#19182,#19183);
#17341=AXIS2_PLACEMENT_3D('',#23714,#19184,#19185);
#17342=AXIS2_PLACEMENT_3D('',#23716,#19186,#19187);
#17343=AXIS2_PLACEMENT_3D('',#23717,#19188,#19189);
#17344=AXIS2_PLACEMENT_3D('',#23718,#19190,#19191);
#17345=AXIS2_PLACEMENT_3D('',#23721,#19193,#19194);
#17346=AXIS2_PLACEMENT_3D('',#24051,#19195,#19196);
#17347=AXIS2_PLACEMENT_3D('',#24109,#19199,#19200);
#17348=AXIS2_PLACEMENT_3D('',#24408,#19203,#19204);
#17349=AXIS2_PLACEMENT_3D('',#24410,#19205,#19206);
#17350=AXIS2_PLACEMENT_3D('',#24411,#19207,#19208);
#17351=AXIS2_PLACEMENT_3D('',#24412,#19209,#19210);
#17352=AXIS2_PLACEMENT_3D('',#24414,#19211,#19212);
#17353=AXIS2_PLACEMENT_3D('',#24418,#19215,#19216);
#17354=AXIS2_PLACEMENT_3D('',#24419,#19217,#19218);
#17355=AXIS2_PLACEMENT_3D('',#24421,#19219,#19220);
#17356=AXIS2_PLACEMENT_3D('',#24423,#19221,#19222);
#17357=AXIS2_PLACEMENT_3D('',#24424,#19223,#19224);
#17358=AXIS2_PLACEMENT_3D('',#24425,#19225,#19226);
#17359=AXIS2_PLACEMENT_3D('',#24442,#19229,#19230);
#17360=AXIS2_PLACEMENT_3D('',#24444,#19232,#19233);
#17361=AXIS2_PLACEMENT_3D('',#24447,#19234,#19235);
#17362=AXIS2_PLACEMENT_3D('',#24448,#19236,#19237);
#17363=AXIS2_PLACEMENT_3D('',#24449,#19238,#19239);
#17364=AXIS2_PLACEMENT_3D('',#24450,#19240,#19241);
#17365=AXIS2_PLACEMENT_3D('',#24461,#19244,#19245);
#17366=AXIS2_PLACEMENT_3D('',#24467,#19249,#19250);
#17367=AXIS2_PLACEMENT_3D('',#24470,#19252,#19253);
#17368=AXIS2_PLACEMENT_3D('',#24471,#19254,#19255);
#17369=AXIS2_PLACEMENT_3D('',#24472,#19256,#19257);
#17370=AXIS2_PLACEMENT_3D('',#24473,#19258,#19259);
#17371=AXIS2_PLACEMENT_3D('',#24474,#19260,#19261);
#17372=AXIS2_PLACEMENT_3D('',#24475,#19262,#19263);
#17373=AXIS2_PLACEMENT_3D('',#24476,#19264,#19265);
#17374=AXIS2_PLACEMENT_3D('',#24478,#19266,#19267);
#17375=AXIS2_PLACEMENT_3D('',#24480,#19268,#19269);
#17376=AXIS2_PLACEMENT_3D('',#24481,#19270,#19271);
#17377=AXIS2_PLACEMENT_3D('',#24482,#19272,#19273);
#17378=AXIS2_PLACEMENT_3D('',#24484,#19274,#19275);
#17379=AXIS2_PLACEMENT_3D('',#24486,#19277,#19278);
#17380=AXIS2_PLACEMENT_3D('',#24488,#19279,#19280);
#17381=AXIS2_PLACEMENT_3D('',#24489,#19281,#19282);
#17382=AXIS2_PLACEMENT_3D('',#24490,#19283,#19284);
#17383=AXIS2_PLACEMENT_3D('',#24491,#19285,#19286);
#17384=AXIS2_PLACEMENT_3D('',#24493,#19288,#19289);
#17385=AXIS2_PLACEMENT_3D('',#24494,#19290,#19291);
#17386=AXIS2_PLACEMENT_3D('',#24495,#19292,#19293);
#17387=AXIS2_PLACEMENT_3D('',#24496,#19294,#19295);
#17388=AXIS2_PLACEMENT_3D('',#24497,#19296,#19297);
#17389=AXIS2_PLACEMENT_3D('',#24499,#19298,#19299);
#17390=AXIS2_PLACEMENT_3D('',#24500,#19300,#19301);
#17391=AXIS2_PLACEMENT_3D('',#24501,#19302,#19303);
#17392=AXIS2_PLACEMENT_3D('',#24503,#19305,#19306);
#17393=AXIS2_PLACEMENT_3D('',#24505,#19308,#19309);
#17394=AXIS2_PLACEMENT_3D('',#24512,#19314,#19315);
#17395=AXIS2_PLACEMENT_3D('',#24515,#19317,#19318);
#17396=AXIS2_PLACEMENT_3D('',#24516,#19319,#19320);
#17397=AXIS2_PLACEMENT_3D('',#24518,#19321,#19322);
#17398=AXIS2_PLACEMENT_3D('',#24527,#19324,#19325);
#17399=AXIS2_PLACEMENT_3D('',#24529,#19326,#19327);
#17400=AXIS2_PLACEMENT_3D('',#24530,#19328,#19329);
#17401=AXIS2_PLACEMENT_3D('',#24531,#19330,#19331);
#17402=AXIS2_PLACEMENT_3D('',#24548,#19334,#19335);
#17403=AXIS2_PLACEMENT_3D('',#24550,#19337,#19338);
#17404=AXIS2_PLACEMENT_3D('',#24551,#19339,#19340);
#17405=AXIS2_PLACEMENT_3D('',#24552,#19341,#19342);
#17406=AXIS2_PLACEMENT_3D('',#24553,#19343,#19344);
#17407=AXIS2_PLACEMENT_3D('',#24554,#19345,#19346);
#17408=AXIS2_PLACEMENT_3D('',#24555,#19347,#19348);
#17409=AXIS2_PLACEMENT_3D('',#24556,#19349,#19350);
#17410=AXIS2_PLACEMENT_3D('',#24557,#19351,#19352);
#17411=AXIS2_PLACEMENT_3D('',#24558,#19353,#19354);
#17412=AXIS2_PLACEMENT_3D('',#24559,#19355,#19356);
#17413=AXIS2_PLACEMENT_3D('',#24560,#19357,#19358);
#17414=AXIS2_PLACEMENT_3D('',#24561,#19359,#19360);
#17415=AXIS2_PLACEMENT_3D('',#24562,#19361,#19362);
#17416=AXIS2_PLACEMENT_3D('',#24563,#19363,#19364);
#17417=AXIS2_PLACEMENT_3D('',#24564,#19365,#19366);
#17418=AXIS2_PLACEMENT_3D('',#24565,#19367,#19368);
#17419=AXIS2_PLACEMENT_3D('',#24566,#19369,#19370);
#17420=AXIS2_PLACEMENT_3D('',#24567,#19371,#19372);
#17421=AXIS2_PLACEMENT_3D('',#24568,#19373,#19374);
#17422=AXIS2_PLACEMENT_3D('',#24569,#19375,#19376);
#17423=AXIS2_PLACEMENT_3D('',#24570,#19377,#19378);
#17424=AXIS2_PLACEMENT_3D('',#24571,#19379,#19380);
#17425=AXIS2_PLACEMENT_3D('',#24572,#19381,#19382);
#17426=AXIS2_PLACEMENT_3D('',#24573,#19383,#19384);
#17427=AXIS2_PLACEMENT_3D('',#24574,#19385,#19386);
#17428=AXIS2_PLACEMENT_3D('',#24575,#19387,#19388);
#17429=AXIS2_PLACEMENT_3D('',#24576,#19389,#19390);
#17430=AXIS2_PLACEMENT_3D('',#24577,#19391,#19392);
#17431=AXIS2_PLACEMENT_3D('',#24578,#19393,#19394);
#17432=AXIS2_PLACEMENT_3D('',#24579,#19395,#19396);
#17433=AXIS2_PLACEMENT_3D('',#24580,#19397,#19398);
#17434=AXIS2_PLACEMENT_3D('',#24581,#19399,#19400);
#17435=AXIS2_PLACEMENT_3D('',#24582,#19401,#19402);
#17436=AXIS2_PLACEMENT_3D('',#24583,#19403,#19404);
#17437=AXIS2_PLACEMENT_3D('',#24584,#19405,#19406);
#17438=AXIS2_PLACEMENT_3D('',#24585,#19407,#19408);
#17439=AXIS2_PLACEMENT_3D('',#24586,#19409,#19410);
#17440=AXIS2_PLACEMENT_3D('',#24587,#19411,#19412);
#17441=AXIS2_PLACEMENT_3D('',#24588,#19413,#19414);
#17442=AXIS2_PLACEMENT_3D('',#24589,#19415,#19416);
#17443=AXIS2_PLACEMENT_3D('',#24590,#19417,#19418);
#17444=AXIS2_PLACEMENT_3D('',#24591,#19419,#19420);
#17445=AXIS2_PLACEMENT_3D('',#24592,#19421,#19422);
#17446=AXIS2_PLACEMENT_3D('',#24593,#19423,#19424);
#17447=AXIS2_PLACEMENT_3D('',#24594,#19425,#19426);
#17448=AXIS2_PLACEMENT_3D('',#24595,#19427,#19428);
#17449=AXIS2_PLACEMENT_3D('',#24596,#19429,#19430);
#17450=AXIS2_PLACEMENT_3D('',#24598,#19432,#19433);
#17451=AXIS2_PLACEMENT_3D('',#24600,#19435,#19436);
#17452=AXIS2_PLACEMENT_3D('',#24602,#19438,#19439);
#17453=AXIS2_PLACEMENT_3D('',#24604,#19441,#19442);
#17454=AXIS2_PLACEMENT_3D('',#24606,#19444,#19445);
#17455=AXIS2_PLACEMENT_3D('',#24608,#19447,#19448);
#17456=AXIS2_PLACEMENT_3D('',#24611,#19450,#19451);
#17457=AXIS2_PLACEMENT_3D('',#24612,#19452,#19453);
#17458=AXIS2_PLACEMENT_3D('',#24614,#19454,#19455);
#17459=AXIS2_PLACEMENT_3D('',#24615,#19456,#19457);
#17460=AXIS2_PLACEMENT_3D('',#24618,#19459,#19460);
#17461=AXIS2_PLACEMENT_3D('',#24619,#19461,#19462);
#17462=AXIS2_PLACEMENT_3D('',#24620,#19463,#19464);
#17463=AXIS2_PLACEMENT_3D('',#24622,#19465,#19466);
#17464=AXIS2_PLACEMENT_3D('',#24623,#19467,#19468);
#17465=AXIS2_PLACEMENT_3D('',#24625,#19470,#19471);
#17466=AXIS2_PLACEMENT_3D('',#24627,#19473,#19474);
#17467=AXIS2_PLACEMENT_3D('',#24628,#19475,#19476);
#17468=AXIS2_PLACEMENT_3D('',#24629,#19477,#19478);
#17469=AXIS2_PLACEMENT_3D('',#24631,#19480,#19481);
#17470=AXIS2_PLACEMENT_3D('',#24633,#19483,#19484);
#17471=AXIS2_PLACEMENT_3D('',#24635,#19486,#19487);
#17472=AXIS2_PLACEMENT_3D('',#24638,#19490,#19491);
#17473=AXIS2_PLACEMENT_3D('',#24639,#19492,#19493);
#17474=AXIS2_PLACEMENT_3D('',#24640,#19494,#19495);
#17475=AXIS2_PLACEMENT_3D('',#24641,#19496,#19497);
#17476=AXIS2_PLACEMENT_3D('',#24642,#19498,#19499);
#17477=AXIS2_PLACEMENT_3D('',#24643,#19500,#19501);
#17478=AXIS2_PLACEMENT_3D('',#24645,#19503,#19504);
#17479=AXIS2_PLACEMENT_3D('',#24646,#19505,#19506);
#17480=AXIS2_PLACEMENT_3D('',#24647,#19507,#19508);
#17481=AXIS2_PLACEMENT_3D('',#24649,#19510,#19511);
#17482=AXIS2_PLACEMENT_3D('',#24651,#19513,#19514);
#17483=AXIS2_PLACEMENT_3D('',#24653,#19516,#19517);
#17484=AXIS2_PLACEMENT_3D('',#24654,#19518,#19519);
#17485=AXIS2_PLACEMENT_3D('',#24655,#19520,#19521);
#17486=AXIS2_PLACEMENT_3D('',#24656,#19522,#19523);
#17487=AXIS2_PLACEMENT_3D('',#24658,#19524,#19525);
#17488=AXIS2_PLACEMENT_3D('',#24661,#19527,#19528);
#17489=AXIS2_PLACEMENT_3D('',#24662,#19529,#19530);
#17490=AXIS2_PLACEMENT_3D('',#24665,#19532,#19533);
#17491=AXIS2_PLACEMENT_3D('',#24666,#19534,#19535);
#17492=AXIS2_PLACEMENT_3D('',#24668,#19536,#19537);
#17493=AXIS2_PLACEMENT_3D('',#24669,#19538,#19539);
#17494=AXIS2_PLACEMENT_3D('',#24672,#19541,#19542);
#17495=AXIS2_PLACEMENT_3D('',#24673,#19543,#19544);
#17496=AXIS2_PLACEMENT_3D('',#24717,#19546,#19547);
#17497=AXIS2_PLACEMENT_3D('',#24719,#19548,#19549);
#17498=AXIS2_PLACEMENT_3D('',#24723,#19551,#19552);
#17499=AXIS2_PLACEMENT_3D('',#24724,#19553,#19554);
#17500=AXIS2_PLACEMENT_3D('',#24725,#19555,#19556);
#17501=AXIS2_PLACEMENT_3D('',#24728,#19558,#19559);
#17502=AXIS2_PLACEMENT_3D('',#24729,#19560,#19561);
#17503=AXIS2_PLACEMENT_3D('',#24731,#19562,#19563);
#17504=AXIS2_PLACEMENT_3D('',#24733,#19564,#19565);
#17505=AXIS2_PLACEMENT_3D('',#24735,#19566,#19567);
#17506=AXIS2_PLACEMENT_3D('',#24737,#19568,#19569);
#17507=AXIS2_PLACEMENT_3D('',#24739,#19570,#19571);
#17508=AXIS2_PLACEMENT_3D('',#24741,#19572,#19573);
#17509=AXIS2_PLACEMENT_3D('',#24743,#19574,#19575);
#17510=AXIS2_PLACEMENT_3D('',#24744,#19576,#19577);
#17511=AXIS2_PLACEMENT_3D('',#24747,#19579,#19580);
#17512=AXIS2_PLACEMENT_3D('',#24748,#19581,#19582);
#17513=AXIS2_PLACEMENT_3D('',#24749,#19583,#19584);
#17514=AXIS2_PLACEMENT_3D('',#24752,#19586,#19587);
#17515=AXIS2_PLACEMENT_3D('',#24753,#19588,#19589);
#17516=AXIS2_PLACEMENT_3D('',#24756,#19591,#19592);
#17517=AXIS2_PLACEMENT_3D('',#24757,#19593,#19594);
#17518=AXIS2_PLACEMENT_3D('',#24760,#19596,#19597);
#17519=AXIS2_PLACEMENT_3D('',#24761,#19598,#19599);
#17520=AXIS2_PLACEMENT_3D('',#24764,#19601,#19602);
#17521=AXIS2_PLACEMENT_3D('',#24765,#19603,#19604);
#17522=AXIS2_PLACEMENT_3D('',#24768,#19606,#19607);
#17523=AXIS2_PLACEMENT_3D('',#24769,#19608,#19609);
#17524=AXIS2_PLACEMENT_3D('',#24772,#19611,#19612);
#17525=AXIS2_PLACEMENT_3D('',#24773,#19613,#19614);
#17526=AXIS2_PLACEMENT_3D('',#24775,#19615,#19616);
#17527=AXIS2_PLACEMENT_3D('',#24777,#19617,#19618);
#17528=AXIS2_PLACEMENT_3D('',#24778,#19619,#19620);
#17529=AXIS2_PLACEMENT_3D('',#24781,#19622,#19623);
#17530=AXIS2_PLACEMENT_3D('',#24782,#19624,#19625);
#17531=AXIS2_PLACEMENT_3D('',#24785,#19627,#19628);
#17532=AXIS2_PLACEMENT_3D('',#24786,#19629,#19630);
#17533=AXIS2_PLACEMENT_3D('',#24788,#19631,#19632);
#17534=AXIS2_PLACEMENT_3D('',#24789,#19633,#19634);
#17535=AXIS2_PLACEMENT_3D('',#24791,#19636,#19637);
#17536=AXIS2_PLACEMENT_3D('',#24793,#19639,#19640);
#17537=AXIS2_PLACEMENT_3D('',#24794,#19641,#19642);
#17538=AXIS2_PLACEMENT_3D('',#24796,#19643,#19644);
#17539=AXIS2_PLACEMENT_3D('',#24799,#19646,#19647);
#17540=AXIS2_PLACEMENT_3D('',#24800,#19648,#19649);
#17541=AXIS2_PLACEMENT_3D('',#24803,#19651,#19652);
#17542=AXIS2_PLACEMENT_3D('',#24804,#19653,#19654);
#17543=AXIS2_PLACEMENT_3D('',#24806,#19655,#19656);
#17544=AXIS2_PLACEMENT_3D('',#24807,#19657,#19658);
#17545=AXIS2_PLACEMENT_3D('',#24811,#19660,#19661);
#17546=AXIS2_PLACEMENT_3D('',#24819,#19662,#19663);
#17547=AXIS2_PLACEMENT_3D('',#24820,#19664,#19665);
#17548=AXIS2_PLACEMENT_3D('',#24823,#19666,#19667);
#17549=AXIS2_PLACEMENT_3D('',#24824,#19668,#19669);
#17550=AXIS2_PLACEMENT_3D('',#24827,#19671,#19672);
#17551=AXIS2_PLACEMENT_3D('',#24828,#19673,#19674);
#17552=AXIS2_PLACEMENT_3D('',#24830,#19675,#19676);
#17553=AXIS2_PLACEMENT_3D('',#24832,#19677,#19678);
#17554=AXIS2_PLACEMENT_3D('',#24834,#19679,#19680);
#17555=AXIS2_PLACEMENT_3D('',#24836,#19681,#19682);
#17556=AXIS2_PLACEMENT_3D('',#24838,#19683,#19684);
#17557=AXIS2_PLACEMENT_3D('',#24840,#19685,#19686);
#17558=AXIS2_PLACEMENT_3D('',#24842,#19687,#19688);
#17559=AXIS2_PLACEMENT_3D('',#24843,#19689,#19690);
#17560=AXIS2_PLACEMENT_3D('',#24845,#19691,#19692);
#17561=AXIS2_PLACEMENT_3D('',#24893,#19694,#19695);
#17562=AXIS2_PLACEMENT_3D('',#24894,#19696,#19697);
#17563=AXIS2_PLACEMENT_3D('',#24897,#19699,#19700);
#17564=AXIS2_PLACEMENT_3D('',#24898,#19701,#19702);
#17565=AXIS2_PLACEMENT_3D('',#24899,#19703,#19704);
#17566=AXIS2_PLACEMENT_3D('',#24902,#19706,#19707);
#17567=AXIS2_PLACEMENT_3D('',#24903,#19708,#19709);
#17568=AXIS2_PLACEMENT_3D('',#24906,#19711,#19712);
#17569=AXIS2_PLACEMENT_3D('',#24907,#19713,#19714);
#17570=AXIS2_PLACEMENT_3D('',#24910,#19716,#19717);
#17571=AXIS2_PLACEMENT_3D('',#24911,#19718,#19719);
#17572=AXIS2_PLACEMENT_3D('',#24914,#19721,#19722);
#17573=AXIS2_PLACEMENT_3D('',#24915,#19723,#19724);
#17574=AXIS2_PLACEMENT_3D('',#24918,#19726,#19727);
#17575=AXIS2_PLACEMENT_3D('',#24919,#19728,#19729);
#17576=AXIS2_PLACEMENT_3D('',#24922,#19731,#19732);
#17577=AXIS2_PLACEMENT_3D('',#24923,#19733,#19734);
#17578=AXIS2_PLACEMENT_3D('',#24925,#19735,#19736);
#17579=AXIS2_PLACEMENT_3D('',#24927,#19738,#19739);
#17580=AXIS2_PLACEMENT_3D('',#24929,#19740,#19741);
#17581=AXIS2_PLACEMENT_3D('',#24931,#19743,#19744);
#17582=AXIS2_PLACEMENT_3D('',#24933,#19745,#19746);
#17583=AXIS2_PLACEMENT_3D('',#24934,#19747,#19748);
#17584=AXIS2_PLACEMENT_3D('',#24937,#19750,#19751);
#17585=AXIS2_PLACEMENT_3D('',#24938,#19752,#19753);
#17586=AXIS2_PLACEMENT_3D('',#24941,#19755,#19756);
#17587=AXIS2_PLACEMENT_3D('',#24942,#19757,#19758);
#17588=AXIS2_PLACEMENT_3D('',#24943,#19759,#19760);
#17589=AXIS2_PLACEMENT_3D('',#24944,#19761,#19762);
#17590=AXIS2_PLACEMENT_3D('',#24946,#19763,#19764);
#17591=AXIS2_PLACEMENT_3D('',#24949,#19766,#19767);
#17592=AXIS2_PLACEMENT_3D('',#24950,#19768,#19769);
#17593=AXIS2_PLACEMENT_3D('',#24952,#19770,#19771);
#17594=AXIS2_PLACEMENT_3D('',#24955,#19773,#19774);
#17595=AXIS2_PLACEMENT_3D('',#24956,#19775,#19776);
#17596=AXIS2_PLACEMENT_3D('',#24958,#19777,#19778);
#17597=AXIS2_PLACEMENT_3D('',#24961,#19780,#19781);
#17598=AXIS2_PLACEMENT_3D('',#24962,#19782,#19783);
#17599=AXIS2_PLACEMENT_3D('',#24964,#19784,#19785);
#17600=AXIS2_PLACEMENT_3D('',#24967,#19787,#19788);
#17601=AXIS2_PLACEMENT_3D('',#24968,#19789,#19790);
#17602=AXIS2_PLACEMENT_3D('',#24970,#19791,#19792);
#17603=AXIS2_PLACEMENT_3D('',#24973,#19794,#19795);
#17604=AXIS2_PLACEMENT_3D('',#24974,#19796,#19797);
#17605=AXIS2_PLACEMENT_3D('',#24976,#19798,#19799);
#17606=AXIS2_PLACEMENT_3D('',#24979,#19801,#19802);
#17607=AXIS2_PLACEMENT_3D('',#24980,#19803,#19804);
#17608=AXIS2_PLACEMENT_3D('',#24982,#19805,#19806);
#17609=AXIS2_PLACEMENT_3D('',#24985,#19808,#19809);
#17610=AXIS2_PLACEMENT_3D('',#24986,#19810,#19811);
#17611=AXIS2_PLACEMENT_3D('',#24988,#19812,#19813);
#17612=AXIS2_PLACEMENT_3D('',#24989,#19814,#19815);
#17613=AXIS2_PLACEMENT_3D('',#24991,#19816,#19817);
#17614=AXIS2_PLACEMENT_3D('',#24993,#19819,#19820);
#17615=AXIS2_PLACEMENT_3D('',#24994,#19821,#19822);
#17616=AXIS2_PLACEMENT_3D('',#24995,#19823,#19824);
#17617=AXIS2_PLACEMENT_3D('',#24997,#19825,#19826);
#17618=AXIS2_PLACEMENT_3D('',#25000,#19828,#19829);
#17619=AXIS2_PLACEMENT_3D('',#25001,#19830,#19831);
#17620=AXIS2_PLACEMENT_3D('',#25003,#19832,#19833);
#17621=AXIS2_PLACEMENT_3D('',#25006,#19835,#19836);
#17622=AXIS2_PLACEMENT_3D('',#25007,#19837,#19838);
#17623=AXIS2_PLACEMENT_3D('',#25009,#19839,#19840);
#17624=AXIS2_PLACEMENT_3D('',#25012,#19842,#19843);
#17625=AXIS2_PLACEMENT_3D('',#25013,#19844,#19845);
#17626=AXIS2_PLACEMENT_3D('',#25015,#19846,#19847);
#17627=AXIS2_PLACEMENT_3D('',#25018,#19849,#19850);
#17628=AXIS2_PLACEMENT_3D('',#25019,#19851,#19852);
#17629=AXIS2_PLACEMENT_3D('',#25021,#19853,#19854);
#17630=AXIS2_PLACEMENT_3D('',#25024,#19856,#19857);
#17631=AXIS2_PLACEMENT_3D('',#25025,#19858,#19859);
#17632=AXIS2_PLACEMENT_3D('',#25027,#19860,#19861);
#17633=AXIS2_PLACEMENT_3D('',#25030,#19863,#19864);
#17634=AXIS2_PLACEMENT_3D('',#25031,#19865,#19866);
#17635=AXIS2_PLACEMENT_3D('',#25033,#19867,#19868);
#17636=AXIS2_PLACEMENT_3D('',#25036,#19870,#19871);
#17637=AXIS2_PLACEMENT_3D('',#25037,#19872,#19873);
#17638=AXIS2_PLACEMENT_3D('',#25039,#19874,#19875);
#17639=AXIS2_PLACEMENT_3D('',#25040,#19876,#19877);
#17640=AXIS2_PLACEMENT_3D('',#25043,#19879,#19880);
#17641=AXIS2_PLACEMENT_3D('',#25044,#19881,#19882);
#17642=AXIS2_PLACEMENT_3D('',#25046,#19883,#19884);
#17643=AXIS2_PLACEMENT_3D('',#25047,#19885,#19886);
#17644=AXIS2_PLACEMENT_3D('',#25049,#19887,#19888);
#17645=AXIS2_PLACEMENT_3D('',#25051,#19890,#19891);
#17646=AXIS2_PLACEMENT_3D('',#25053,#19892,#19893);
#17647=AXIS2_PLACEMENT_3D('',#25054,#19894,#19895);
#17648=AXIS2_PLACEMENT_3D('',#25057,#19897,#19898);
#17649=AXIS2_PLACEMENT_3D('',#25058,#19899,#19900);
#17650=AXIS2_PLACEMENT_3D('',#25059,#19901,#19902);
#17651=AXIS2_PLACEMENT_3D('',#25060,#19903,#19904);
#17652=AXIS2_PLACEMENT_3D('',#25063,#19905,#19906);
#17653=AXIS2_PLACEMENT_3D('',#25064,#19907,#19908);
#17654=AXIS2_PLACEMENT_3D('',#25067,#19910,#19911);
#17655=AXIS2_PLACEMENT_3D('',#25068,#19912,#19913);
#17656=AXIS2_PLACEMENT_3D('',#25070,#19914,#19915);
#17657=AXIS2_PLACEMENT_3D('',#25071,#19916,#19917);
#17658=AXIS2_PLACEMENT_3D('',#25073,#19918,#19919);
#17659=AXIS2_PLACEMENT_3D('',#25075,#19921,#19922);
#17660=AXIS2_PLACEMENT_3D('',#25077,#19923,#19924);
#17661=AXIS2_PLACEMENT_3D('',#25079,#19926,#19927);
#17662=AXIS2_PLACEMENT_3D('',#25081,#19928,#19929);
#17663=AXIS2_PLACEMENT_3D('',#25083,#19931,#19932);
#17664=AXIS2_PLACEMENT_3D('',#25084,#19933,#19934);
#17665=AXIS2_PLACEMENT_3D('',#25085,#19935,#19936);
#17666=AXIS2_PLACEMENT_3D('',#25087,#19937,#19938);
#17667=AXIS2_PLACEMENT_3D('',#25091,#19940,#19941);
#17668=AXIS2_PLACEMENT_3D('',#25092,#19942,#19943);
#17669=AXIS2_PLACEMENT_3D('',#25093,#19944,#19945);
#17670=AXIS2_PLACEMENT_3D('',#25095,#19946,#19947);
#17671=AXIS2_PLACEMENT_3D('',#25096,#19948,#19949);
#17672=AXIS2_PLACEMENT_3D('',#25099,#19951,#19952);
#17673=AXIS2_PLACEMENT_3D('',#25100,#19953,#19954);
#17674=AXIS2_PLACEMENT_3D('',#25102,#19955,#19956);
#17675=AXIS2_PLACEMENT_3D('',#25106,#19958,#19959);
#17676=AXIS2_PLACEMENT_3D('',#25107,#19960,#19961);
#17677=AXIS2_PLACEMENT_3D('',#25108,#19962,#19963);
#17678=AXIS2_PLACEMENT_3D('',#25111,#19964,#19965);
#17679=AXIS2_PLACEMENT_3D('',#25112,#19966,#19967);
#17680=AXIS2_PLACEMENT_3D('',#25114,#19969,#19970);
#17681=AXIS2_PLACEMENT_3D('',#25116,#19971,#19972);
#17682=AXIS2_PLACEMENT_3D('',#25117,#19973,#19974);
#17683=AXIS2_PLACEMENT_3D('',#25119,#19976,#19977);
#17684=AXIS2_PLACEMENT_3D('',#25121,#19979,#19980);
#17685=AXIS2_PLACEMENT_3D('',#25122,#19981,#19982);
#17686=AXIS2_PLACEMENT_3D('',#25144,#19984,#19985);
#17687=AXIS2_PLACEMENT_3D('',#25155,#19986,#19987);
#17688=AXIS2_PLACEMENT_3D('',#25239,#19989,#19990);
#17689=AXIS2_PLACEMENT_3D('',#25329,#19992,#19993);
#17690=AXIS2_PLACEMENT_3D('',#25419,#19995,#19996);
#17691=AXIS2_PLACEMENT_3D('',#25503,#19998,#19999);
#17692=AXIS2_PLACEMENT_3D('',#25593,#20001,#20002);
#17693=AXIS2_PLACEMENT_3D('',#25677,#20004,#20005);
#17694=AXIS2_PLACEMENT_3D('',#25764,#20007,#20008);
#17695=AXIS2_PLACEMENT_3D('',#25839,#20010,#20011);
#17696=AXIS2_PLACEMENT_3D('',#25923,#20013,#20014);
#17697=AXIS2_PLACEMENT_3D('',#26013,#20016,#20017);
#17698=AXIS2_PLACEMENT_3D('',#26097,#20019,#20020);
#17699=AXIS2_PLACEMENT_3D('',#26184,#20022,#20023);
#17700=AXIS2_PLACEMENT_3D('',#26274,#20025,#20026);
#17701=AXIS2_PLACEMENT_3D('',#26358,#20028,#20029);
#17702=AXIS2_PLACEMENT_3D('',#26373,#20031,#20032);
#17703=AXIS2_PLACEMENT_3D('',#26380,#20033,#20034);
#17704=AXIS2_PLACEMENT_3D('',#26417,#20036,#20037);
#17705=AXIS2_PLACEMENT_3D('',#26454,#20039,#20040);
#17706=AXIS2_PLACEMENT_3D('',#26492,#20042,#20043);
#17707=AXIS2_PLACEMENT_3D('',#26529,#20045,#20046);
#17708=AXIS2_PLACEMENT_3D('',#26566,#20048,#20049);
#17709=AXIS2_PLACEMENT_3D('',#26603,#20051,#20052);
#17710=AXIS2_PLACEMENT_3D('',#26638,#20054,#20055);
#17711=AXIS2_PLACEMENT_3D('',#26672,#20057,#20058);
#17712=AXIS2_PLACEMENT_3D('',#26709,#20060,#20061);
#17713=AXIS2_PLACEMENT_3D('',#26746,#20063,#20064);
#17714=AXIS2_PLACEMENT_3D('',#26783,#20066,#20067);
#17715=AXIS2_PLACEMENT_3D('',#26820,#20069,#20070);
#17716=AXIS2_PLACEMENT_3D('',#26858,#20072,#20073);
#17717=AXIS2_PLACEMENT_3D('',#26895,#20075,#20076);
#17718=AXIS2_PLACEMENT_3D('',#26917,#20078,#20079);
#17719=AXIS2_PLACEMENT_3D('',#26928,#20080,#20081);
#17720=AXIS2_PLACEMENT_3D('',#27012,#20083,#20084);
#17721=AXIS2_PLACEMENT_3D('',#27102,#20086,#20087);
#17722=AXIS2_PLACEMENT_3D('',#27192,#20089,#20090);
#17723=AXIS2_PLACEMENT_3D('',#27276,#20092,#20093);
#17724=AXIS2_PLACEMENT_3D('',#27366,#20095,#20096);
#17725=AXIS2_PLACEMENT_3D('',#27450,#20098,#20099);
#17726=AXIS2_PLACEMENT_3D('',#27537,#20101,#20102);
#17727=AXIS2_PLACEMENT_3D('',#27612,#20104,#20105);
#17728=AXIS2_PLACEMENT_3D('',#27696,#20107,#20108);
#17729=AXIS2_PLACEMENT_3D('',#27786,#20110,#20111);
#17730=AXIS2_PLACEMENT_3D('',#27870,#20113,#20114);
#17731=AXIS2_PLACEMENT_3D('',#27957,#20116,#20117);
#17732=AXIS2_PLACEMENT_3D('',#28047,#20119,#20120);
#17733=AXIS2_PLACEMENT_3D('',#28131,#20122,#20123);
#17734=AXIS2_PLACEMENT_3D('',#28146,#20125,#20126);
#17735=AXIS2_PLACEMENT_3D('',#28153,#20127,#20128);
#17736=AXIS2_PLACEMENT_3D('',#28190,#20130,#20131);
#17737=AXIS2_PLACEMENT_3D('',#28227,#20133,#20134);
#17738=AXIS2_PLACEMENT_3D('',#28265,#20136,#20137);
#17739=AXIS2_PLACEMENT_3D('',#28302,#20139,#20140);
#17740=AXIS2_PLACEMENT_3D('',#28339,#20142,#20143);
#17741=AXIS2_PLACEMENT_3D('',#28376,#20145,#20146);
#17742=AXIS2_PLACEMENT_3D('',#28411,#20148,#20149);
#17743=AXIS2_PLACEMENT_3D('',#28445,#20151,#20152);
#17744=AXIS2_PLACEMENT_3D('',#28482,#20154,#20155);
#17745=AXIS2_PLACEMENT_3D('',#28519,#20157,#20158);
#17746=AXIS2_PLACEMENT_3D('',#28556,#20160,#20161);
#17747=AXIS2_PLACEMENT_3D('',#28593,#20163,#20164);
#17748=AXIS2_PLACEMENT_3D('',#28631,#20166,#20167);
#17749=AXIS2_PLACEMENT_3D('',#28668,#20169,#20170);
#17750=AXIS2_PLACEMENT_3D('',#28783,#20171,#20172);
#17751=AXIS2_PLACEMENT_3D('',#28785,#20173,#20174);
#17752=AXIS2_PLACEMENT_3D('',#29835,#20175,#20176);
#17753=AXIS2_PLACEMENT_3D('',#29837,#20177,#20178);
#17754=AXIS2_PLACEMENT_3D('',#30766,#20179,#20180);
#17755=AXIS2_PLACEMENT_3D('',#30767,#20181,#20182);
#17756=AXIS2_PLACEMENT_3D('',#31818,#20183,#20184);
#17757=AXIS2_PLACEMENT_3D('',#31820,#20185,#20186);
#17758=AXIS2_PLACEMENT_3D('',#31821,#20187,#20188);
#17759=AXIS2_PLACEMENT_3D('',#31932,#20189,#20190);
#17760=AXIS2_PLACEMENT_3D('',#31933,#20191,#20192);
#17761=AXIS2_PLACEMENT_3D('',#32866,#20193,#20194);
#17762=AXIS2_PLACEMENT_3D('',#32868,#20195,#20196);
#17763=AXIS2_PLACEMENT_3D('',#32869,#20197,#20198);
#17764=AXIS2_PLACEMENT_3D('',#32871,#20200,#20201);
#17765=AXIS2_PLACEMENT_3D('',#32872,#20202,#20203);
#17766=AXIS2_PLACEMENT_3D('',#32873,#20204,#20205);
#17767=AXIS2_PLACEMENT_3D('',#32875,#20206,#20207);
#17768=AXIS2_PLACEMENT_3D('',#32876,#20208,#20209);
#17769=AXIS2_PLACEMENT_3D('',#32878,#20210,#20211);
#17770=AXIS2_PLACEMENT_3D('',#32880,#20213,#20214);
#17771=AXIS2_PLACEMENT_3D('',#32881,#20215,#20216);
#17772=AXIS2_PLACEMENT_3D('',#32883,#20217,#20218);
#17773=AXIS2_PLACEMENT_3D('',#32885,#20220,#20221);
#17774=AXIS2_PLACEMENT_3D('',#32886,#20222,#20223);
#17775=AXIS2_PLACEMENT_3D('',#32887,#20224,#20225);
#17776=AXIS2_PLACEMENT_3D('',#32889,#20226,#20227);
#17777=AXIS2_PLACEMENT_3D('',#32913,#20229,#20230);
#17778=AXIS2_PLACEMENT_3D('',#32947,#20231,#20232);
#17779=AXIS2_PLACEMENT_3D('',#32981,#20233,#20234);
#17780=AXIS2_PLACEMENT_3D('',#33015,#20235,#20236);
#17781=AXIS2_PLACEMENT_3D('',#33049,#20237,#20238);
#17782=AXIS2_PLACEMENT_3D('',#33083,#20239,#20240);
#17783=AXIS2_PLACEMENT_3D('',#33197,#20241,#20242);
#17784=AXIS2_PLACEMENT_3D('',#33198,#20243,#20244);
#17785=AXIS2_PLACEMENT_3D('',#33203,#20245,#20246);
#17786=AXIS2_PLACEMENT_3D('',#33213,#20247,#20248);
#17787=AXIS2_PLACEMENT_3D('',#33223,#20249,#20250);
#17788=AXIS2_PLACEMENT_3D('',#33233,#20251,#20252);
#17789=AXIS2_PLACEMENT_3D('',#33277,#20253,#20254);
#17790=AXIS2_PLACEMENT_3D('',#33279,#20255,#20256);
#17791=AXIS2_PLACEMENT_3D('',#33280,#20257,#20258);
#17792=AXIS2_PLACEMENT_3D('',#33282,#20260,#20261);
#17793=AXIS2_PLACEMENT_3D('',#33291,#20263,#20264);
#17794=AXIS2_PLACEMENT_3D('',#33293,#20266,#20267);
#17795=AXIS2_PLACEMENT_3D('',#33309,#20269,#20270);
#17796=AXIS2_PLACEMENT_3D('',#33318,#20272,#20273);
#17797=AXIS2_PLACEMENT_3D('',#33359,#20275,#20276);
#17798=AXIS2_PLACEMENT_3D('',#33392,#20279,#20280);
#17799=AXIS2_PLACEMENT_3D('',#33400,#20283,#20284);
#17800=AXIS2_PLACEMENT_3D('',#33433,#20287,#20288);
#17801=AXIS2_PLACEMENT_3D('',#33441,#20291,#20292);
#17802=AXIS2_PLACEMENT_3D('',#33449,#20295,#20296);
#17803=AXIS2_PLACEMENT_3D('',#33457,#20299,#20300);
#17804=AXIS2_PLACEMENT_3D('',#33461,#20301,#20302);
#17805=AXIS2_PLACEMENT_3D('',#33465,#20303,#20304);
#17806=AXIS2_PLACEMENT_3D('',#33469,#20305,#20306);
#17807=AXIS2_PLACEMENT_3D('',#33471,#20307,#20308);
#17808=AXIS2_PLACEMENT_3D('',#33486,#20310,#20311);
#17809=AXIS2_PLACEMENT_3D('',#33488,#20312,#20313);
#17810=AXIS2_PLACEMENT_3D('',#33491,#20315,#20316);
#17811=AXIS2_PLACEMENT_3D('',#33492,#20317,#20318);
#17812=AXIS2_PLACEMENT_3D('',#33495,#20320,#20321);
#17813=AXIS2_PLACEMENT_3D('',#33496,#20322,#20323);
#17814=AXIS2_PLACEMENT_3D('',#33498,#20325,#20326);
#17815=AXIS2_PLACEMENT_3D('',#33499,#20327,#20328);
#17816=AXIS2_PLACEMENT_3D('',#33500,#20329,#20330);
#17817=AXIS2_PLACEMENT_3D('',#33501,#20331,#20332);
#17818=AXIS2_PLACEMENT_3D('',#33502,#20333,#20334);
#17819=AXIS2_PLACEMENT_3D('',#33503,#20335,#20336);
#17820=AXIS2_PLACEMENT_3D('',#33505,#20337,#20338);
#17821=AXIS2_PLACEMENT_3D('',#33509,#20340,#20341);
#17822=AXIS2_PLACEMENT_3D('',#33510,#20342,#20343);
#17823=AXIS2_PLACEMENT_3D('',#33511,#20344,#20345);
#17824=AXIS2_PLACEMENT_3D('',#33513,#20346,#20347);
#17825=AXIS2_PLACEMENT_3D('',#33514,#20348,#20349);
#17826=AXIS2_PLACEMENT_3D('',#33521,#20353,#20354);
#17827=AXIS2_PLACEMENT_3D('',#33523,#20355,#20356);
#17828=AXIS2_PLACEMENT_3D('',#33524,#20357,#20358);
#17829=AXIS2_PLACEMENT_3D('',#33526,#20359,#20360);
#17830=AXIS2_PLACEMENT_3D('',#33527,#20361,#20362);
#17831=AXIS2_PLACEMENT_3D('',#33528,#20363,#20364);
#17832=AXIS2_PLACEMENT_3D('',#33530,#20365,#20366);
#17833=AXIS2_PLACEMENT_3D('',#33533,#20368,#20369);
#17834=AXIS2_PLACEMENT_3D('',#33534,#20370,#20371);
#17835=AXIS2_PLACEMENT_3D('',#33536,#20372,#20373);
#17836=AXIS2_PLACEMENT_3D('',#33537,#20374,#20375);
#17837=AXIS2_PLACEMENT_3D('',#33539,#20376,#20377);
#17838=AXIS2_PLACEMENT_3D('',#33541,#20379,#20380);
#17839=AXIS2_PLACEMENT_3D('',#33543,#20381,#20382);
#17840=AXIS2_PLACEMENT_3D('',#33544,#20383,#20384);
#17841=AXIS2_PLACEMENT_3D('',#33545,#20385,#20386);
#17842=AXIS2_PLACEMENT_3D('',#33549,#20388,#20389);
#17843=AXIS2_PLACEMENT_3D('',#33550,#20390,#20391);
#17844=AXIS2_PLACEMENT_3D('',#33551,#20392,#20393);
#17845=AXIS2_PLACEMENT_3D('',#33553,#20394,#20395);
#17846=AXIS2_PLACEMENT_3D('',#33554,#20396,#20397);
#17847=AXIS2_PLACEMENT_3D('',#33555,#20398,#20399);
#17848=AXIS2_PLACEMENT_3D('',#33557,#20400,#20401);
#17849=AXIS2_PLACEMENT_3D('',#33558,#20402,#20403);
#17850=AXIS2_PLACEMENT_3D('',#33560,#20404,#20405);
#17851=AXIS2_PLACEMENT_3D('',#33562,#20406,#20407);
#17852=AXIS2_PLACEMENT_3D('',#33564,#20408,#20409);
#17853=AXIS2_PLACEMENT_3D('',#33565,#20410,#20411);
#17854=AXIS2_PLACEMENT_3D('',#33566,#20412,#20413);
#17855=AXIS2_PLACEMENT_3D('',#33569,#20415,#20416);
#17856=AXIS2_PLACEMENT_3D('',#33570,#20417,#20418);
#17857=AXIS2_PLACEMENT_3D('',#33572,#20419,#20420);
#17858=AXIS2_PLACEMENT_3D('',#33573,#20421,#20422);
#17859=AXIS2_PLACEMENT_3D('',#33575,#20423,#20424);
#17860=AXIS2_PLACEMENT_3D('',#33576,#20425,#20426);
#17861=AXIS2_PLACEMENT_3D('',#33577,#20427,#20428);
#17862=AXIS2_PLACEMENT_3D('',#33579,#20429,#20430);
#17863=AXIS2_PLACEMENT_3D('',#33580,#20431,#20432);
#17864=AXIS2_PLACEMENT_3D('',#33583,#20433,#20434);
#17865=AXIS2_PLACEMENT_3D('',#33587,#20436,#20437);
#17866=AXIS2_PLACEMENT_3D('',#33589,#20439,#20440);
#17867=AXIS2_PLACEMENT_3D('',#33592,#20441,#20442);
#17868=AXIS2_PLACEMENT_3D('',#33593,#20443,#20444);
#17869=AXIS2_PLACEMENT_3D('',#33594,#20445,#20446);
#17870=AXIS2_PLACEMENT_3D('',#33595,#20447,#20448);
#17871=AXIS2_PLACEMENT_3D('',#33598,#20449,#20450);
#17872=AXIS2_PLACEMENT_3D('',#33601,#20453,#20454);
#17873=AXIS2_PLACEMENT_3D('',#33604,#20455,#20456);
#17874=AXIS2_PLACEMENT_3D('',#33605,#20457,#20458);
#17875=AXIS2_PLACEMENT_3D('',#33606,#20459,#20460);
#17876=AXIS2_PLACEMENT_3D('',#33607,#20461,#20462);
#17877=AXIS2_PLACEMENT_3D('',#33610,#20463,#20464);
#17878=AXIS2_PLACEMENT_3D('',#33613,#20467,#20468);
#17879=AXIS2_PLACEMENT_3D('',#33616,#20469,#20470);
#17880=AXIS2_PLACEMENT_3D('',#33617,#20471,#20472);
#17881=AXIS2_PLACEMENT_3D('',#33618,#20473,#20474);
#17882=AXIS2_PLACEMENT_3D('',#33619,#20475,#20476);
#17883=AXIS2_PLACEMENT_3D('',#33622,#20477,#20478);
#17884=AXIS2_PLACEMENT_3D('',#33625,#20481,#20482);
#17885=AXIS2_PLACEMENT_3D('',#33626,#20483,#20484);
#17886=AXIS2_PLACEMENT_3D('',#33627,#20485,#20486);
#17887=AXIS2_PLACEMENT_3D('',#33628,#20487,#20488);
#17888=AXIS2_PLACEMENT_3D('',#33632,#20490,#20491);
#17889=AXIS2_PLACEMENT_3D('',#33634,#20493,#20494);
#17890=AXIS2_PLACEMENT_3D('',#33638,#20497,#20498);
#17891=AXIS2_PLACEMENT_3D('',#33641,#20500,#20501);
#17892=AXIS2_PLACEMENT_3D('',#33642,#20502,#20503);
#17893=AXIS2_PLACEMENT_3D('',#33647,#20506,#20507);
#17894=AXIS2_PLACEMENT_3D('',#33648,#20508,#20509);
#17895=AXIS2_PLACEMENT_3D('',#33650,#20510,#20511);
#17896=AXIS2_PLACEMENT_3D('',#33652,#20512,#20513);
#17897=AXIS2_PLACEMENT_3D('',#33654,#20514,#20515);
#17898=AXIS2_PLACEMENT_3D('',#33655,#20516,#20517);
#17899=AXIS2_PLACEMENT_3D('',#33657,#20518,#20519);
#17900=AXIS2_PLACEMENT_3D('',#33660,#20521,#20522);
#17901=AXIS2_PLACEMENT_3D('',#33661,#20523,#20524);
#17902=AXIS2_PLACEMENT_3D('',#33663,#20525,#20526);
#17903=AXIS2_PLACEMENT_3D('',#33664,#20527,#20528);
#17904=AXIS2_PLACEMENT_3D('',#33665,#20529,#20530);
#17905=AXIS2_PLACEMENT_3D('',#33667,#20531,#20532);
#17906=AXIS2_PLACEMENT_3D('',#33669,#20534,#20535);
#17907=AXIS2_PLACEMENT_3D('',#33671,#20536,#20537);
#17908=AXIS2_PLACEMENT_3D('',#33672,#20538,#20539);
#17909=AXIS2_PLACEMENT_3D('',#33673,#20540,#20541);
#17910=AXIS2_PLACEMENT_3D('',#33676,#20542,#20543);
#17911=AXIS2_PLACEMENT_3D('',#33679,#20546,#20547);
#17912=AXIS2_PLACEMENT_3D('',#33682,#20548,#20549);
#17913=AXIS2_PLACEMENT_3D('',#33683,#20550,#20551);
#17914=AXIS2_PLACEMENT_3D('',#33684,#20552,#20553);
#17915=AXIS2_PLACEMENT_3D('',#33685,#20554,#20555);
#17916=AXIS2_PLACEMENT_3D('',#33688,#20556,#20557);
#17917=AXIS2_PLACEMENT_3D('',#33691,#20560,#20561);
#17918=AXIS2_PLACEMENT_3D('',#33692,#20562,#20563);
#17919=AXIS2_PLACEMENT_3D('',#33693,#20564,#20565);
#17920=AXIS2_PLACEMENT_3D('',#33694,#20566,#20567);
#17921=AXIS2_PLACEMENT_3D('',#33697,#20570,#20571);
#17922=AXIS2_PLACEMENT_3D('',#33699,#20573,#20574);
#17923=AXIS2_PLACEMENT_3D('',#33700,#20575,#20576);
#17924=AXIS2_PLACEMENT_3D('',#33702,#20577,#20578);
#17925=AXIS2_PLACEMENT_3D('',#33704,#20579,#20580);
#17926=AXIS2_PLACEMENT_3D('',#33705,#20581,#20582);
#17927=AXIS2_PLACEMENT_3D('',#33708,#20583,#20584);
#17928=AXIS2_PLACEMENT_3D('',#33712,#20586,#20587);
#17929=AXIS2_PLACEMENT_3D('',#33714,#20589,#20590);
#17930=AXIS2_PLACEMENT_3D('',#33717,#20591,#20592);
#17931=AXIS2_PLACEMENT_3D('',#33718,#20593,#20594);
#17932=AXIS2_PLACEMENT_3D('',#33719,#20595,#20596);
#17933=AXIS2_PLACEMENT_3D('',#33720,#20597,#20598);
#17934=AXIS2_PLACEMENT_3D('',#33723,#20599,#20600);
#17935=AXIS2_PLACEMENT_3D('',#33726,#20603,#20604);
#17936=AXIS2_PLACEMENT_3D('',#33729,#20605,#20606);
#17937=AXIS2_PLACEMENT_3D('',#33730,#20607,#20608);
#17938=AXIS2_PLACEMENT_3D('',#33731,#20609,#20610);
#17939=AXIS2_PLACEMENT_3D('',#33732,#20611,#20612);
#17940=AXIS2_PLACEMENT_3D('',#33735,#20613,#20614);
#17941=AXIS2_PLACEMENT_3D('',#33738,#20617,#20618);
#17942=AXIS2_PLACEMENT_3D('',#33741,#20619,#20620);
#17943=AXIS2_PLACEMENT_3D('',#33742,#20621,#20622);
#17944=AXIS2_PLACEMENT_3D('',#33743,#20623,#20624);
#17945=AXIS2_PLACEMENT_3D('',#33744,#20625,#20626);
#17946=AXIS2_PLACEMENT_3D('',#33747,#20627,#20628);
#17947=AXIS2_PLACEMENT_3D('',#33750,#20631,#20632);
#17948=AXIS2_PLACEMENT_3D('',#33751,#20633,#20634);
#17949=AXIS2_PLACEMENT_3D('',#33752,#20635,#20636);
#17950=AXIS2_PLACEMENT_3D('',#33753,#20637,#20638);
#17951=AXIS2_PLACEMENT_3D('',#33757,#20640,#20641);
#17952=AXIS2_PLACEMENT_3D('',#33759,#20643,#20644);
#17953=AXIS2_PLACEMENT_3D('',#33763,#20647,#20648);
#17954=AXIS2_PLACEMENT_3D('',#33766,#20650,#20651);
#17955=AXIS2_PLACEMENT_3D('',#33767,#20652,#20653);
#17956=AXIS2_PLACEMENT_3D('',#33772,#20656,#20657);
#17957=AXIS2_PLACEMENT_3D('',#33773,#20658,#20659);
#17958=AXIS2_PLACEMENT_3D('',#33775,#20660,#20661);
#17959=AXIS2_PLACEMENT_3D('',#33777,#20662,#20663);
#17960=AXIS2_PLACEMENT_3D('',#33779,#20664,#20665);
#17961=AXIS2_PLACEMENT_3D('',#33780,#20666,#20667);
#17962=AXIS2_PLACEMENT_3D('',#33782,#20668,#20669);
#17963=AXIS2_PLACEMENT_3D('',#33785,#20671,#20672);
#17964=AXIS2_PLACEMENT_3D('',#33786,#20673,#20674);
#17965=AXIS2_PLACEMENT_3D('',#33788,#20675,#20676);
#17966=AXIS2_PLACEMENT_3D('',#33789,#20677,#20678);
#17967=AXIS2_PLACEMENT_3D('',#33790,#20679,#20680);
#17968=AXIS2_PLACEMENT_3D('',#33792,#20681,#20682);
#17969=AXIS2_PLACEMENT_3D('',#33794,#20684,#20685);
#17970=AXIS2_PLACEMENT_3D('',#33796,#20686,#20687);
#17971=AXIS2_PLACEMENT_3D('',#33797,#20688,#20689);
#17972=AXIS2_PLACEMENT_3D('',#33798,#20690,#20691);
#17973=AXIS2_PLACEMENT_3D('',#33801,#20692,#20693);
#17974=AXIS2_PLACEMENT_3D('',#33804,#20696,#20697);
#17975=AXIS2_PLACEMENT_3D('',#33807,#20698,#20699);
#17976=AXIS2_PLACEMENT_3D('',#33808,#20700,#20701);
#17977=AXIS2_PLACEMENT_3D('',#33809,#20702,#20703);
#17978=AXIS2_PLACEMENT_3D('',#33810,#20704,#20705);
#17979=AXIS2_PLACEMENT_3D('',#33813,#20706,#20707);
#17980=AXIS2_PLACEMENT_3D('',#33816,#20710,#20711);
#17981=AXIS2_PLACEMENT_3D('',#33817,#20712,#20713);
#17982=AXIS2_PLACEMENT_3D('',#33818,#20714,#20715);
#17983=AXIS2_PLACEMENT_3D('',#33819,#20716,#20717);
#17984=AXIS2_PLACEMENT_3D('',#33822,#20720,#20721);
#17985=AXIS2_PLACEMENT_3D('',#33824,#20723,#20724);
#17986=AXIS2_PLACEMENT_3D('',#33825,#20725,#20726);
#17987=AXIS2_PLACEMENT_3D('',#33827,#20727,#20728);
#17988=AXIS2_PLACEMENT_3D('',#33829,#20729,#20730);
#17989=AXIS2_PLACEMENT_3D('',#33881,#20731,#20732);
#17990=AXIS2_PLACEMENT_3D('',#33882,#20733,#20734);
#17991=AXIS2_PLACEMENT_3D('',#33933,#20735,#20736);
#17992=AXIS2_PLACEMENT_3D('',#33985,#20737,#20738);
#17993=AXIS2_PLACEMENT_3D('',#33986,#20739,#20740);
#17994=AXIS2_PLACEMENT_3D('',#34037,#20741,#20742);
#17995=AXIS2_PLACEMENT_3D('',#34038,#20743,#20744);
#17996=AXIS2_PLACEMENT_3D('',#34040,#20746,#20747);
#17997=AXIS2_PLACEMENT_3D('',#34042,#20749,#20750);
#17998=AXIS2_PLACEMENT_3D('',#34044,#20752,#20753);
#17999=AXIS2_PLACEMENT_3D('',#34046,#20755,#20756);
#18000=AXIS2_PLACEMENT_3D('',#34048,#20758,#20759);
#18001=AXIS2_PLACEMENT_3D('',#34050,#20761,#20762);
#18002=AXIS2_PLACEMENT_3D('',#34052,#20764,#20765);
#18003=AXIS2_PLACEMENT_3D('',#34053,#20766,#20767);
#18004=AXIS2_PLACEMENT_3D('',#34055,#20768,#20769);
#18005=AXIS2_PLACEMENT_3D('',#34056,#20770,#20771);
#18006=AXIS2_PLACEMENT_3D('',#34058,#20773,#20774);
#18007=AXIS2_PLACEMENT_3D('',#34060,#20775,#20776);
#18008=AXIS2_PLACEMENT_3D('',#34061,#20777,#20778);
#18009=AXIS2_PLACEMENT_3D('',#34063,#20780,#20781);
#18010=AXIS2_PLACEMENT_3D('',#34065,#20783,#20784);
#18011=AXIS2_PLACEMENT_3D('',#34066,#20785,#20786);
#18012=AXIS2_PLACEMENT_3D('',#34088,#20788,#20789);
#18013=AXIS2_PLACEMENT_3D('',#34099,#20790,#20791);
#18014=AXIS2_PLACEMENT_3D('',#34183,#20793,#20794);
#18015=AXIS2_PLACEMENT_3D('',#34273,#20796,#20797);
#18016=AXIS2_PLACEMENT_3D('',#34357,#20799,#20800);
#18017=AXIS2_PLACEMENT_3D('',#34447,#20802,#20803);
#18018=AXIS2_PLACEMENT_3D('',#34537,#20805,#20806);
#18019=AXIS2_PLACEMENT_3D('',#34546,#20808,#20809);
#18020=AXIS2_PLACEMENT_3D('',#34547,#20810,#20811);
#18021=AXIS2_PLACEMENT_3D('',#34569,#20813,#20814);
#18022=AXIS2_PLACEMENT_3D('',#34584,#20815,#20816);
#18023=AXIS2_PLACEMENT_3D('',#34622,#20818,#20819);
#18024=AXIS2_PLACEMENT_3D('',#34659,#20821,#20822);
#18025=AXIS2_PLACEMENT_3D('',#34696,#20824,#20825);
#18026=AXIS2_PLACEMENT_3D('',#34733,#20827,#20828);
#18027=AXIS2_PLACEMENT_3D('',#34735,#20829,#20830);
#18028=AXIS2_PLACEMENT_3D('',#34739,#20832,#20833);
#18029=AXIS2_PLACEMENT_3D('',#34740,#20834,#20835);
#18030=AXIS2_PLACEMENT_3D('',#34741,#20836,#20837);
#18031=AXIS2_PLACEMENT_3D('',#34745,#20839,#20840);
#18032=AXIS2_PLACEMENT_3D('',#34746,#20841,#20842);
#18033=AXIS2_PLACEMENT_3D('',#34747,#20843,#20844);
#18034=AXIS2_PLACEMENT_3D('',#34883,#20845,#20846);
#18035=AXIS2_PLACEMENT_3D('',#35017,#20847,#20848);
#18036=AXIS2_PLACEMENT_3D('',#35021,#20850,#20851);
#18037=AXIS2_PLACEMENT_3D('',#35022,#20852,#20853);
#18038=AXIS2_PLACEMENT_3D('',#35023,#20854,#20855);
#18039=AXIS2_PLACEMENT_3D('',#35027,#20857,#20858);
#18040=AXIS2_PLACEMENT_3D('',#35028,#20859,#20860);
#18041=AXIS2_PLACEMENT_3D('',#35029,#20861,#20862);
#18042=AXIS2_PLACEMENT_3D('',#35032,#20864,#20865);
#18043=AXIS2_PLACEMENT_3D('',#35033,#20866,#20867);
#18044=AXIS2_PLACEMENT_3D('',#35046,#20874,#20875);
#18045=AXIS2_PLACEMENT_3D('',#35052,#20879,#20880);
#18046=AXIS2_PLACEMENT_3D('',#35056,#20883,#20884);
#18047=AXIS2_PLACEMENT_3D('',#35062,#20888,#20889);
#18048=AXIS2_PLACEMENT_3D('',#35066,#20892,#20893);
#18049=AXIS2_PLACEMENT_3D('',#35068,#20895,#20896);
#18050=AXIS2_PLACEMENT_3D('',#35070,#20898,#20899);
#18051=AXIS2_PLACEMENT_3D('',#35076,#20903,#20904);
#18052=AXIS2_PLACEMENT_3D('',#35080,#20907,#20908);
#18053=AXIS2_PLACEMENT_3D('',#35084,#20911,#20912);
#18054=AXIS2_PLACEMENT_3D('',#35220,#20913,#20914);
#18055=AXIS2_PLACEMENT_3D('',#35222,#20915,#20916);
#18056=AXIS2_PLACEMENT_3D('',#35708,#20917,#20918);
#18057=AXIS2_PLACEMENT_3D('',#36053,#20919,#20920);
#18058=AXIS2_PLACEMENT_3D('',#36054,#20921,#20922);
#18059=AXIS2_PLACEMENT_3D('',#36055,#20923,#20924);
#18060=AXIS2_PLACEMENT_3D('',#36059,#20927,#20928);
#18061=AXIS2_PLACEMENT_3D('',#36063,#20931,#20932);
#18062=AXIS2_PLACEMENT_3D('',#36065,#20934,#20935);
#18063=AXIS2_PLACEMENT_3D('',#36066,#20936,#20937);
#18064=AXIS2_PLACEMENT_3D('',#36068,#20938,#20939);
#18065=AXIS2_PLACEMENT_3D('',#36070,#20941,#20942);
#18066=AXIS2_PLACEMENT_3D('',#36071,#20943,#20944);
#18067=AXIS2_PLACEMENT_3D('',#36072,#20945,#20946);
#18068=AXIS2_PLACEMENT_3D('',#36075,#20947,#20948);
#18069=AXIS2_PLACEMENT_3D('',#36079,#20950,#20951);
#18070=AXIS2_PLACEMENT_3D('',#36083,#20953,#20954);
#18071=AXIS2_PLACEMENT_3D('',#36087,#20956,#20957);
#18072=AXIS2_PLACEMENT_3D('',#36090,#20959,#20960);
#18073=AXIS2_PLACEMENT_3D('',#36091,#20961,#20962);
#18074=AXIS2_PLACEMENT_3D('',#36097,#20966,#20967);
#18075=AXIS2_PLACEMENT_3D('',#36099,#20968,#20969);
#18076=AXIS2_PLACEMENT_3D('',#36101,#20971,#20972);
#18077=AXIS2_PLACEMENT_3D('',#36105,#20975,#20976);
#18078=AXIS2_PLACEMENT_3D('',#36107,#20977,#20978);
#18079=AXIS2_PLACEMENT_3D('',#36109,#20980,#20981);
#18080=AXIS2_PLACEMENT_3D('',#36113,#20984,#20985);
#18081=AXIS2_PLACEMENT_3D('',#36115,#20986,#20987);
#18082=AXIS2_PLACEMENT_3D('',#36117,#20989,#20990);
#18083=AXIS2_PLACEMENT_3D('',#36121,#20993,#20994);
#18084=AXIS2_PLACEMENT_3D('',#36122,#20995,#20996);
#18085=AXIS2_PLACEMENT_3D('',#36123,#20997,#20998);
#18086=AXIS2_PLACEMENT_3D('',#36124,#20999,#21000);
#18087=AXIS2_PLACEMENT_3D('',#36128,#21002,#21003);
#18088=AXIS2_PLACEMENT_3D('',#36130,#21004,#21005);
#18089=AXIS2_PLACEMENT_3D('',#36131,#21006,#21007);
#18090=AXIS2_PLACEMENT_3D('',#36132,#21008,#21009);
#18091=AXIS2_PLACEMENT_3D('',#36146,#21017,#21018);
#18092=AXIS2_PLACEMENT_3D('',#36148,#21019,#21020);
#18093=AXIS2_PLACEMENT_3D('',#36149,#21021,#21022);
#18094=AXIS2_PLACEMENT_3D('',#36152,#21024,#21025);
#18095=AXIS2_PLACEMENT_3D('',#36153,#21026,#21027);
#18096=AXIS2_PLACEMENT_3D('',#36157,#21029,#21030);
#18097=AXIS2_PLACEMENT_3D('',#36158,#21031,#21032);
#18098=AXIS2_PLACEMENT_3D('',#36162,#21034,#21035);
#18099=AXIS2_PLACEMENT_3D('',#36163,#21036,#21037);
#18100=AXIS2_PLACEMENT_3D('',#36167,#21039,#21040);
#18101=AXIS2_PLACEMENT_3D('',#36168,#21041,#21042);
#18102=AXIS2_PLACEMENT_3D('',#36173,#21044,#21045);
#18103=AXIS2_PLACEMENT_3D('',#36174,#21046,#21047);
#18104=AXIS2_PLACEMENT_3D('',#36175,#21048,#21049);
#18105=AXIS2_PLACEMENT_3D('',#36176,#21050,#21051);
#18106=AXIS2_PLACEMENT_3D('',#36177,#21052,#21053);
#18107=AXIS2_PLACEMENT_3D('',#36181,#21055,#21056);
#18108=AXIS2_PLACEMENT_3D('',#36182,#21057,#21058);
#18109=AXIS2_PLACEMENT_3D('',#36184,#21059,#21060);
#18110=AXIS2_PLACEMENT_3D('',#36186,#21062,#21063);
#18111=AXIS2_PLACEMENT_3D('',#36187,#21064,#21065);
#18112=AXIS2_PLACEMENT_3D('',#36188,#21066,#21067);
#18113=AXIS2_PLACEMENT_3D('',#36189,#21068,#21069);
#18114=AXIS2_PLACEMENT_3D('',#36190,#21070,#21071);
#18115=AXIS2_PLACEMENT_3D('',#36191,#21072,#21073);
#18116=AXIS2_PLACEMENT_3D('',#36192,#21074,#21075);
#18117=AXIS2_PLACEMENT_3D('',#36194,#21076,#21077);
#18118=AXIS2_PLACEMENT_3D('',#36196,#21079,#21080);
#18119=AXIS2_PLACEMENT_3D('',#36197,#21081,#21082);
#18120=AXIS2_PLACEMENT_3D('',#36201,#21085,#21086);
#18121=AXIS2_PLACEMENT_3D('',#36203,#21088,#21089);
#18122=AXIS2_PLACEMENT_3D('',#36207,#21092,#21093);
#18123=AXIS2_PLACEMENT_3D('',#36209,#21095,#21096);
#18124=AXIS2_PLACEMENT_3D('',#36213,#21099,#21100);
#18125=AXIS2_PLACEMENT_3D('',#36224,#21106,#21107);
#18126=AXIS2_PLACEMENT_3D('',#36225,#21108,#21109);
#18127=AXIS2_PLACEMENT_3D('',#36228,#21112,#21113);
#18128=AXIS2_PLACEMENT_3D('',#36232,#21116,#21117);
#18129=AXIS2_PLACEMENT_3D('',#36234,#21119,#21120);
#18130=AXIS2_PLACEMENT_3D('',#36236,#21122,#21123);
#18131=AXIS2_PLACEMENT_3D('',#36237,#21124,#21125);
#18132=AXIS2_PLACEMENT_3D('',#36238,#21126,#21127);
#18133=AXIS2_PLACEMENT_3D('',#36240,#21128,#21129);
#18134=AXIS2_PLACEMENT_3D('',#36241,#21130,#21131);
#18135=AXIS2_PLACEMENT_3D('',#36243,#21132,#21133);
#18136=AXIS2_PLACEMENT_3D('',#36245,#21135,#21136);
#18137=AXIS2_PLACEMENT_3D('',#36247,#21138,#21139);
#18138=AXIS2_PLACEMENT_3D('',#36248,#21140,#21141);
#18139=AXIS2_PLACEMENT_3D('',#36255,#21145,#21146);
#18140=AXIS2_PLACEMENT_3D('',#36262,#21150,#21151);
#18141=AXIS2_PLACEMENT_3D('',#36269,#21155,#21156);
#18142=AXIS2_PLACEMENT_3D('',#36272,#21159,#21160);
#18143=AXIS2_PLACEMENT_3D('',#36279,#21164,#21165);
#18144=AXIS2_PLACEMENT_3D('',#36286,#21169,#21170);
#18145=AXIS2_PLACEMENT_3D('',#36293,#21174,#21175);
#18146=AXIS2_PLACEMENT_3D('',#36296,#21178,#21179);
#18147=AXIS2_PLACEMENT_3D('',#36299,#21182,#21183);
#18148=AXIS2_PLACEMENT_3D('',#36305,#21187,#21188);
#18149=AXIS2_PLACEMENT_3D('',#36311,#21192,#21193);
#18150=AXIS2_PLACEMENT_3D('',#36314,#21196,#21197);
#18151=AXIS2_PLACEMENT_3D('',#36317,#21200,#21201);
#18152=AXIS2_PLACEMENT_3D('',#36323,#21205,#21206);
#18153=AXIS2_PLACEMENT_3D('',#36329,#21210,#21211);
#18154=AXIS2_PLACEMENT_3D('',#36332,#21214,#21215);
#18155=AXIS2_PLACEMENT_3D('',#36338,#21219,#21220);
#18156=AXIS2_PLACEMENT_3D('',#36344,#21224,#21225);
#18157=AXIS2_PLACEMENT_3D('',#36346,#21227,#21228);
#18158=AXIS2_PLACEMENT_3D('',#36348,#21230,#21231);
#18159=AXIS2_PLACEMENT_3D('',#36350,#21233,#21234);
#18160=AXIS2_PLACEMENT_3D('',#36352,#21235,#21236);
#18161=AXIS2_PLACEMENT_3D('',#36353,#21237,#21238);
#18162=AXIS2_PLACEMENT_3D('',#36356,#21239,#21240);
#18163=AXIS2_PLACEMENT_3D('',#36357,#21241,#21242);
#18164=AXIS2_PLACEMENT_3D('',#36361,#21244,#21245);
#18165=AXIS2_PLACEMENT_3D('',#36362,#21246,#21247);
#18166=AXIS2_PLACEMENT_3D('',#36363,#21248,#21249);
#18167=AXIS2_PLACEMENT_3D('',#36367,#21251,#21252);
#18168=AXIS2_PLACEMENT_3D('',#36368,#21253,#21254);
#18169=AXIS2_PLACEMENT_3D('',#36369,#21255,#21256);
#18170=AXIS2_PLACEMENT_3D('',#36371,#21257,#21258);
#18171=AXIS2_PLACEMENT_3D('',#36373,#21260,#21261);
#18172=AXIS2_PLACEMENT_3D('',#36376,#21263,#21264);
#18173=AXIS2_PLACEMENT_3D('',#36377,#21265,#21266);
#18174=AXIS2_PLACEMENT_3D('',#36378,#21267,#21268);
#18175=AXIS2_PLACEMENT_3D('',#36380,#21269,#21270);
#18176=AXIS2_PLACEMENT_3D('',#36384,#21272,#21273);
#18177=AXIS2_PLACEMENT_3D('',#36385,#21274,#21275);
#18178=AXIS2_PLACEMENT_3D('',#36386,#21276,#21277);
#18179=AXIS2_PLACEMENT_3D('',#36389,#21279,#21280);
#18180=AXIS2_PLACEMENT_3D('',#36390,#21281,#21282);
#18181=AXIS2_PLACEMENT_3D('',#36394,#21286,#21287);
#18182=AXIS2_PLACEMENT_3D('',#36396,#21288,#21289);
#18183=AXIS2_PLACEMENT_3D('',#36397,#21290,#21291);
#18184=AXIS2_PLACEMENT_3D('',#36399,#21292,#21293);
#18185=AXIS2_PLACEMENT_3D('',#36401,#21294,#21295);
#18186=AXIS2_PLACEMENT_3D('',#36402,#21296,#21297);
#18187=AXIS2_PLACEMENT_3D('',#36404,#21299,#21300);
#18188=AXIS2_PLACEMENT_3D('',#36406,#21301,#21302);
#18189=AXIS2_PLACEMENT_3D('',#36408,#21304,#21305);
#18190=AXIS2_PLACEMENT_3D('',#36410,#21306,#21307);
#18191=AXIS2_PLACEMENT_3D('',#36411,#21308,#21309);
#18192=AXIS2_PLACEMENT_3D('',#36413,#21310,#21311);
#18193=AXIS2_PLACEMENT_3D('',#36414,#21312,#21313);
#18194=AXIS2_PLACEMENT_3D('',#36416,#21315,#21316);
#18195=AXIS2_PLACEMENT_3D('',#36417,#21317,#21318);
#18196=AXIS2_PLACEMENT_3D('',#36418,#21319,#21320);
#18197=AXIS2_PLACEMENT_3D('',#36419,#21321,#21322);
#18198=AXIS2_PLACEMENT_3D('',#36421,#21323,#21324);
#18199=AXIS2_PLACEMENT_3D('',#36423,#21326,#21327);
#18200=AXIS2_PLACEMENT_3D('',#36425,#21328,#21329);
#18201=AXIS2_PLACEMENT_3D('',#36427,#21331,#21332);
#18202=AXIS2_PLACEMENT_3D('',#36428,#21333,#21334);
#18203=AXIS2_PLACEMENT_3D('',#36429,#21335,#21336);
#18204=AXIS2_PLACEMENT_3D('',#36432,#21337,#21338);
#18205=AXIS2_PLACEMENT_3D('',#36433,#21339,#21340);
#18206=AXIS2_PLACEMENT_3D('',#36434,#21341,#21342);
#18207=AXIS2_PLACEMENT_3D('',#36436,#21343,#21344);
#18208=AXIS2_PLACEMENT_3D('',#36439,#21346,#21347);
#18209=AXIS2_PLACEMENT_3D('',#36440,#21348,#21349);
#18210=AXIS2_PLACEMENT_3D('',#36442,#21350,#21351);
#18211=AXIS2_PLACEMENT_3D('',#36443,#21352,#21353);
#18212=AXIS2_PLACEMENT_3D('',#36445,#21354,#21355);
#18213=AXIS2_PLACEMENT_3D('',#36447,#21357,#21358);
#18214=AXIS2_PLACEMENT_3D('',#36449,#21359,#21360);
#18215=AXIS2_PLACEMENT_3D('',#36451,#21362,#21363);
#18216=AXIS2_PLACEMENT_3D('',#36453,#21364,#21365);
#18217=AXIS2_PLACEMENT_3D('',#36455,#21367,#21368);
#18218=AXIS2_PLACEMENT_3D('',#36456,#21369,#21370);
#18219=AXIS2_PLACEMENT_3D('',#36457,#21371,#21372);
#18220=AXIS2_PLACEMENT_3D('',#36459,#21373,#21374);
#18221=AXIS2_PLACEMENT_3D('',#36462,#21376,#21377);
#18222=AXIS2_PLACEMENT_3D('',#36463,#21378,#21379);
#18223=AXIS2_PLACEMENT_3D('',#36473,#21384,#21385);
#18224=AXIS2_PLACEMENT_3D('',#36475,#21386,#21387);
#18225=AXIS2_PLACEMENT_3D('',#36477,#21388,#21389);
#18226=AXIS2_PLACEMENT_3D('',#36479,#21390,#21391);
#18227=AXIS2_PLACEMENT_3D('',#36481,#21392,#21393);
#18228=AXIS2_PLACEMENT_3D('',#36482,#21394,#21395);
#18229=AXIS2_PLACEMENT_3D('',#36484,#21396,#21397);
#18230=AXIS2_PLACEMENT_3D('',#36486,#21399,#21400);
#18231=AXIS2_PLACEMENT_3D('',#36489,#21402,#21403);
#18232=AXIS2_PLACEMENT_3D('',#36490,#21404,#21405);
#18233=AXIS2_PLACEMENT_3D('',#36492,#21406,#21407);
#18234=AXIS2_PLACEMENT_3D('',#36494,#21409,#21410);
#18235=AXIS2_PLACEMENT_3D('',#36503,#21415,#21416);
#18236=AXIS2_PLACEMENT_3D('',#36505,#21417,#21418);
#18237=AXIS2_PLACEMENT_3D('',#36508,#21420,#21421);
#18238=AXIS2_PLACEMENT_3D('',#36509,#21422,#21423);
#18239=AXIS2_PLACEMENT_3D('',#36515,#21427,#21428);
#18240=AXIS2_PLACEMENT_3D('',#36517,#21429,#21430);
#18241=AXIS2_PLACEMENT_3D('',#36520,#21432,#21433);
#18242=AXIS2_PLACEMENT_3D('',#36521,#21434,#21435);
#18243=AXIS2_PLACEMENT_3D('',#36527,#21439,#21440);
#18244=AXIS2_PLACEMENT_3D('',#36529,#21441,#21442);
#18245=AXIS2_PLACEMENT_3D('',#36532,#21444,#21445);
#18246=AXIS2_PLACEMENT_3D('',#36533,#21446,#21447);
#18247=AXIS2_PLACEMENT_3D('',#36539,#21451,#21452);
#18248=AXIS2_PLACEMENT_3D('',#36540,#21453,#21454);
#18249=AXIS2_PLACEMENT_3D('',#36543,#21456,#21457);
#18250=AXIS2_PLACEMENT_3D('',#36544,#21458,#21459);
#18251=AXIS2_PLACEMENT_3D('',#36548,#21462,#21463);
#18252=AXIS2_PLACEMENT_3D('',#36550,#21464,#21465);
#18253=AXIS2_PLACEMENT_3D('',#36553,#21467,#21468);
#18254=AXIS2_PLACEMENT_3D('',#36554,#21469,#21470);
#18255=AXIS2_PLACEMENT_3D('',#36560,#21474,#21475);
#18256=AXIS2_PLACEMENT_3D('',#36562,#21476,#21477);
#18257=AXIS2_PLACEMENT_3D('',#36565,#21479,#21480);
#18258=AXIS2_PLACEMENT_3D('',#36566,#21481,#21482);
#18259=AXIS2_PLACEMENT_3D('',#36572,#21486,#21487);
#18260=AXIS2_PLACEMENT_3D('',#36574,#21488,#21489);
#18261=AXIS2_PLACEMENT_3D('',#36577,#21491,#21492);
#18262=AXIS2_PLACEMENT_3D('',#36578,#21493,#21494);
#18263=AXIS2_PLACEMENT_3D('',#36584,#21498,#21499);
#18264=AXIS2_PLACEMENT_3D('',#36585,#21500,#21501);
#18265=AXIS2_PLACEMENT_3D('',#36586,#21502,#21503);
#18266=AXIS2_PLACEMENT_3D('',#36587,#21504,#21505);
#18267=AXIS2_PLACEMENT_3D('',#36590,#21507,#21508);
#18268=AXIS2_PLACEMENT_3D('',#36591,#21509,#21510);
#18269=AXIS2_PLACEMENT_3D('',#36595,#21513,#21514);
#18270=AXIS2_PLACEMENT_3D('',#36598,#21516,#21517);
#18271=AXIS2_PLACEMENT_3D('',#36599,#21518,#21519);
#18272=AXIS2_PLACEMENT_3D('',#36603,#21522,#21523);
#18273=AXIS2_PLACEMENT_3D('',#36606,#21525,#21526);
#18274=AXIS2_PLACEMENT_3D('',#36607,#21527,#21528);
#18275=AXIS2_PLACEMENT_3D('',#36611,#21531,#21532);
#18276=AXIS2_PLACEMENT_3D('',#36614,#21534,#21535);
#18277=AXIS2_PLACEMENT_3D('',#36615,#21536,#21537);
#18278=AXIS2_PLACEMENT_3D('',#36620,#21540,#21541);
#18279=AXIS2_PLACEMENT_3D('',#36622,#21542,#21543);
#18280=AXIS2_PLACEMENT_3D('',#36624,#21544,#21545);
#18281=AXIS2_PLACEMENT_3D('',#36626,#21546,#21547);
#18282=AXIS2_PLACEMENT_3D('',#36628,#21548,#21549);
#18283=AXIS2_PLACEMENT_3D('',#36630,#21550,#21551);
#18284=AXIS2_PLACEMENT_3D('',#36631,#21552,#21553);
#18285=AXIS2_PLACEMENT_3D('',#36632,#21554,#21555);
#18286=AXIS2_PLACEMENT_3D('',#36638,#21559,#21560);
#18287=AXIS2_PLACEMENT_3D('',#36640,#21561,#21562);
#18288=AXIS2_PLACEMENT_3D('',#36643,#21564,#21565);
#18289=AXIS2_PLACEMENT_3D('',#36644,#21566,#21567);
#18290=AXIS2_PLACEMENT_3D('',#36650,#21571,#21572);
#18291=AXIS2_PLACEMENT_3D('',#36652,#21573,#21574);
#18292=AXIS2_PLACEMENT_3D('',#36655,#21576,#21577);
#18293=AXIS2_PLACEMENT_3D('',#36656,#21578,#21579);
#18294=AXIS2_PLACEMENT_3D('',#36662,#21583,#21584);
#18295=AXIS2_PLACEMENT_3D('',#36664,#21585,#21586);
#18296=AXIS2_PLACEMENT_3D('',#36667,#21588,#21589);
#18297=AXIS2_PLACEMENT_3D('',#36668,#21590,#21591);
#18298=AXIS2_PLACEMENT_3D('',#36674,#21595,#21596);
#18299=AXIS2_PLACEMENT_3D('',#36675,#21597,#21598);
#18300=AXIS2_PLACEMENT_3D('',#36678,#21600,#21601);
#18301=AXIS2_PLACEMENT_3D('',#36679,#21602,#21603);
#18302=AXIS2_PLACEMENT_3D('',#36683,#21606,#21607);
#18303=AXIS2_PLACEMENT_3D('',#36686,#21609,#21610);
#18304=AXIS2_PLACEMENT_3D('',#36687,#21611,#21612);
#18305=AXIS2_PLACEMENT_3D('',#36691,#21615,#21616);
#18306=AXIS2_PLACEMENT_3D('',#36694,#21618,#21619);
#18307=AXIS2_PLACEMENT_3D('',#36695,#21620,#21621);
#18308=AXIS2_PLACEMENT_3D('',#36699,#21624,#21625);
#18309=AXIS2_PLACEMENT_3D('',#36702,#21627,#21628);
#18310=AXIS2_PLACEMENT_3D('',#36703,#21629,#21630);
#18311=AXIS2_PLACEMENT_3D('',#36707,#21633,#21634);
#18312=AXIS2_PLACEMENT_3D('',#36708,#21635,#21636);
#18313=AXIS2_PLACEMENT_3D('',#36709,#21637,#21638);
#18314=AXIS2_PLACEMENT_3D('',#36711,#21640,#21641);
#18315=AXIS2_PLACEMENT_3D('',#36713,#21643,#21644);
#18316=AXIS2_PLACEMENT_3D('',#36715,#21646,#21647);
#18317=AXIS2_PLACEMENT_3D('',#36717,#21649,#21650);
#18318=AXIS2_PLACEMENT_3D('',#36719,#21652,#21653);
#18319=AXIS2_PLACEMENT_3D('',#36721,#21655,#21656);
#18320=AXIS2_PLACEMENT_3D('',#36722,#21657,#21658);
#18321=AXIS2_PLACEMENT_3D('',#36723,#21659,#21660);
#18322=AXIS2_PLACEMENT_3D('',#36725,#21662,#21663);
#18323=AXIS2_PLACEMENT_3D('',#36727,#21665,#21666);
#18324=AXIS2_PLACEMENT_3D('',#36729,#21668,#21669);
#18325=AXIS2_PLACEMENT_3D('',#36731,#21671,#21672);
#18326=AXIS2_PLACEMENT_3D('',#36733,#21674,#21675);
#18327=AXIS2_PLACEMENT_3D('',#36735,#21677,#21678);
#18328=AXIS2_PLACEMENT_3D('',#36736,#21679,#21680);
#18329=AXIS2_PLACEMENT_3D('',#36752,#21682,#21683);
#18330=AXIS2_PLACEMENT_3D('',#36760,#21684,#21685);
#18331=AXIS2_PLACEMENT_3D('',#36808,#21687,#21688);
#18332=AXIS2_PLACEMENT_3D('',#36856,#21690,#21691);
#18333=AXIS2_PLACEMENT_3D('',#36910,#21693,#21694);
#18334=AXIS2_PLACEMENT_3D('',#36958,#21696,#21697);
#18335=AXIS2_PLACEMENT_3D('',#37006,#21699,#21700);
#18336=AXIS2_PLACEMENT_3D('',#37060,#21702,#21703);
#18337=AXIS2_PLACEMENT_3D('',#37108,#21705,#21706);
#18338=AXIS2_PLACEMENT_3D('',#37162,#21708,#21709);
#18339=AXIS2_PLACEMENT_3D('',#37167,#21711,#21712);
#18340=AXIS2_PLACEMENT_3D('',#37209,#21713,#21714);
#18341=AXIS2_PLACEMENT_3D('',#37222,#21716,#21717);
#18342=AXIS2_PLACEMENT_3D('',#37229,#21718,#21719);
#18343=AXIS2_PLACEMENT_3D('',#37254,#21721,#21722);
#18344=AXIS2_PLACEMENT_3D('',#37279,#21724,#21725);
#18345=AXIS2_PLACEMENT_3D('',#37304,#21727,#21728);
#18346=AXIS2_PLACEMENT_3D('',#37329,#21730,#21731);
#18347=AXIS2_PLACEMENT_3D('',#37353,#21733,#21734);
#18348=AXIS2_PLACEMENT_3D('',#37378,#21736,#21737);
#18349=AXIS2_PLACEMENT_3D('',#37403,#21739,#21740);
#18350=AXIS2_PLACEMENT_3D('',#37427,#21742,#21743);
#18351=AXIS2_PLACEMENT_3D('',#37430,#21744,#21745);
#18352=AXIS2_PLACEMENT_3D('',#37431,#21746,#21747);
#18353=AXIS2_PLACEMENT_3D('',#37435,#21749,#21750);
#18354=AXIS2_PLACEMENT_3D('',#37436,#21751,#21752);
#18355=AXIS2_PLACEMENT_3D('',#37437,#21753,#21754);
#18356=AXIS2_PLACEMENT_3D('',#37441,#21756,#21757);
#18357=AXIS2_PLACEMENT_3D('',#37442,#21758,#21759);
#18358=AXIS2_PLACEMENT_3D('',#37443,#21760,#21761);
#18359=AXIS2_PLACEMENT_3D('',#37445,#21762,#21763);
#18360=AXIS2_PLACEMENT_3D('',#37447,#21765,#21766);
#18361=AXIS2_PLACEMENT_3D('',#37450,#21768,#21769);
#18362=AXIS2_PLACEMENT_3D('',#37451,#21770,#21771);
#18363=AXIS2_PLACEMENT_3D('',#37452,#21772,#21773);
#18364=AXIS2_PLACEMENT_3D('',#37551,#21774,#21775);
#18365=AXIS2_PLACEMENT_3D('',#38016,#21776,#21777);
#18366=AXIS2_PLACEMENT_3D('',#38018,#21778,#21779);
#18367=AXIS2_PLACEMENT_3D('',#38380,#21780,#21781);
#18368=AXIS2_PLACEMENT_3D('',#38381,#21782,#21783);
#18369=AXIS2_PLACEMENT_3D('',#38382,#21784,#21785);
#18370=AXIS2_PLACEMENT_3D('',#38384,#21786,#21787);
#18371=AXIS2_PLACEMENT_3D('',#38386,#21789,#21790);
#18372=AXIS2_PLACEMENT_3D('',#38387,#21791,#21792);
#18373=AXIS2_PLACEMENT_3D('',#38389,#21793,#21794);
#18374=AXIS2_PLACEMENT_3D('',#38391,#21796,#21797);
#18375=AXIS2_PLACEMENT_3D('',#38392,#21798,#21799);
#18376=AXIS2_PLACEMENT_3D('',#38393,#21800,#21801);
#18377=AXIS2_PLACEMENT_3D('',#38409,#21803,#21804);
#18378=AXIS2_PLACEMENT_3D('',#38417,#21805,#21806);
#18379=AXIS2_PLACEMENT_3D('',#38465,#21808,#21809);
#18380=AXIS2_PLACEMENT_3D('',#38513,#21811,#21812);
#18381=AXIS2_PLACEMENT_3D('',#38564,#21814,#21815);
#18382=AXIS2_PLACEMENT_3D('',#38615,#21817,#21818);
#18383=AXIS2_PLACEMENT_3D('',#38663,#21820,#21821);
#18384=AXIS2_PLACEMENT_3D('',#38711,#21823,#21824);
#18385=AXIS2_PLACEMENT_3D('',#38765,#21826,#21827);
#18386=AXIS2_PLACEMENT_3D('',#38813,#21829,#21830);
#18387=AXIS2_PLACEMENT_3D('',#38861,#21832,#21833);
#18388=AXIS2_PLACEMENT_3D('',#38915,#21835,#21836);
#18389=AXIS2_PLACEMENT_3D('',#38963,#21838,#21839);
#18390=AXIS2_PLACEMENT_3D('',#39011,#21841,#21842);
#18391=AXIS2_PLACEMENT_3D('',#39059,#21844,#21845);
#18392=AXIS2_PLACEMENT_3D('',#39113,#21847,#21848);
#18393=AXIS2_PLACEMENT_3D('',#39161,#21850,#21851);
#18394=AXIS2_PLACEMENT_3D('',#39209,#21853,#21854);
#18395=AXIS2_PLACEMENT_3D('',#39263,#21856,#21857);
#18396=AXIS2_PLACEMENT_3D('',#39311,#21859,#21860);
#18397=AXIS2_PLACEMENT_3D('',#39359,#21862,#21863);
#18398=AXIS2_PLACEMENT_3D('',#39413,#21865,#21866);
#18399=AXIS2_PLACEMENT_3D('',#39461,#21868,#21869);
#18400=AXIS2_PLACEMENT_3D('',#39509,#21871,#21872);
#18401=AXIS2_PLACEMENT_3D('',#39557,#21874,#21875);
#18402=AXIS2_PLACEMENT_3D('',#39611,#21877,#21878);
#18403=AXIS2_PLACEMENT_3D('',#39659,#21880,#21881);
#18404=AXIS2_PLACEMENT_3D('',#39707,#21883,#21884);
#18405=AXIS2_PLACEMENT_3D('',#39761,#21886,#21887);
#18406=AXIS2_PLACEMENT_3D('',#39809,#21889,#21890);
#18407=AXIS2_PLACEMENT_3D('',#39857,#21892,#21893);
#18408=AXIS2_PLACEMENT_3D('',#39911,#21895,#21896);
#18409=AXIS2_PLACEMENT_3D('',#39959,#21898,#21899);
#18410=AXIS2_PLACEMENT_3D('',#40007,#21901,#21902);
#18411=AXIS2_PLACEMENT_3D('',#40055,#21904,#21905);
#18412=AXIS2_PLACEMENT_3D('',#40109,#21907,#21908);
#18413=AXIS2_PLACEMENT_3D('',#40157,#21910,#21911);
#18414=AXIS2_PLACEMENT_3D('',#40205,#21913,#21914);
#18415=AXIS2_PLACEMENT_3D('',#40259,#21916,#21917);
#18416=AXIS2_PLACEMENT_3D('',#40307,#21919,#21920);
#18417=AXIS2_PLACEMENT_3D('',#40355,#21922,#21923);
#18418=AXIS2_PLACEMENT_3D('',#40409,#21925,#21926);
#18419=AXIS2_PLACEMENT_3D('',#40457,#21928,#21929);
#18420=AXIS2_PLACEMENT_3D('',#40505,#21931,#21932);
#18421=AXIS2_PLACEMENT_3D('',#40553,#21934,#21935);
#18422=AXIS2_PLACEMENT_3D('',#40562,#21937,#21938);
#18423=AXIS2_PLACEMENT_3D('',#40563,#21939,#21940);
#18424=AXIS2_PLACEMENT_3D('',#40578,#21942,#21943);
#18425=AXIS2_PLACEMENT_3D('',#40588,#21944,#21945);
#18426=AXIS2_PLACEMENT_3D('',#40612,#21947,#21948);
#18427=AXIS2_PLACEMENT_3D('',#40636,#21950,#21951);
#18428=AXIS2_PLACEMENT_3D('',#40661,#21953,#21954);
#18429=AXIS2_PLACEMENT_3D('',#40686,#21956,#21957);
#18430=AXIS2_PLACEMENT_3D('',#40710,#21959,#21960);
#18431=AXIS2_PLACEMENT_3D('',#40735,#21962,#21963);
#18432=AXIS2_PLACEMENT_3D('',#40760,#21965,#21966);
#18433=AXIS2_PLACEMENT_3D('',#40784,#21968,#21969);
#18434=AXIS2_PLACEMENT_3D('',#40809,#21971,#21972);
#18435=AXIS2_PLACEMENT_3D('',#40834,#21974,#21975);
#18436=AXIS2_PLACEMENT_3D('',#40858,#21977,#21978);
#18437=AXIS2_PLACEMENT_3D('',#40882,#21980,#21981);
#18438=AXIS2_PLACEMENT_3D('',#40907,#21983,#21984);
#18439=AXIS2_PLACEMENT_3D('',#40932,#21986,#21987);
#18440=AXIS2_PLACEMENT_3D('',#40956,#21989,#21990);
#18441=AXIS2_PLACEMENT_3D('',#40981,#21992,#21993);
#18442=AXIS2_PLACEMENT_3D('',#41006,#21995,#21996);
#18443=AXIS2_PLACEMENT_3D('',#41030,#21998,#21999);
#18444=AXIS2_PLACEMENT_3D('',#41055,#22001,#22002);
#18445=AXIS2_PLACEMENT_3D('',#41080,#22004,#22005);
#18446=AXIS2_PLACEMENT_3D('',#41104,#22007,#22008);
#18447=AXIS2_PLACEMENT_3D('',#41128,#22010,#22011);
#18448=AXIS2_PLACEMENT_3D('',#41153,#22013,#22014);
#18449=AXIS2_PLACEMENT_3D('',#41178,#22016,#22017);
#18450=AXIS2_PLACEMENT_3D('',#41202,#22019,#22020);
#18451=AXIS2_PLACEMENT_3D('',#41227,#22022,#22023);
#18452=AXIS2_PLACEMENT_3D('',#41252,#22025,#22026);
#18453=AXIS2_PLACEMENT_3D('',#41276,#22028,#22029);
#18454=AXIS2_PLACEMENT_3D('',#41301,#22031,#22032);
#18455=AXIS2_PLACEMENT_3D('',#41326,#22034,#22035);
#18456=AXIS2_PLACEMENT_3D('',#41350,#22037,#22038);
#18457=AXIS2_PLACEMENT_3D('',#41374,#22040,#22041);
#18458=AXIS2_PLACEMENT_3D('',#41399,#22043,#22044);
#18459=AXIS2_PLACEMENT_3D('',#41424,#22046,#22047);
#18460=AXIS2_PLACEMENT_3D('',#41448,#22049,#22050);
#18461=AXIS2_PLACEMENT_3D('',#41473,#22052,#22053);
#18462=AXIS2_PLACEMENT_3D('',#41498,#22055,#22056);
#18463=AXIS2_PLACEMENT_3D('',#41522,#22058,#22059);
#18464=AXIS2_PLACEMENT_3D('',#41547,#22061,#22062);
#18465=AXIS2_PLACEMENT_3D('',#41571,#22064,#22065);
#18466=AXIS2_PLACEMENT_3D('',#41596,#22067,#22068);
#18467=AXIS2_PLACEMENT_3D('',#42961,#22070,#22071);
#18468=AXIS2_PLACEMENT_3D('',#42963,#22072,#22073);
#18469=AXIS2_PLACEMENT_3D('',#42964,#22074,#22075);
#18470=AXIS2_PLACEMENT_3D('',#43063,#22076,#22077);
#18471=AXIS2_PLACEMENT_3D('',#43064,#22078,#22079);
#18472=AXIS2_PLACEMENT_3D('',#44304,#22080,#22081);
#18473=AXIS2_PLACEMENT_3D('',#44328,#22083,#22084);
#18474=AXIS2_PLACEMENT_3D('',#44336,#22085,#22086);
#18475=AXIS2_PLACEMENT_3D('',#44342,#22090,#22091);
#18476=AXIS2_PLACEMENT_3D('',#44346,#22094,#22095);
#18477=AXIS2_PLACEMENT_3D('',#44350,#22098,#22099);
#18478=AXIS2_PLACEMENT_3D('',#44356,#22103,#22104);
#18479=AXIS2_PLACEMENT_3D('',#44357,#22105,#22106);
#18480=AXIS2_PLACEMENT_3D('',#44359,#22108,#22109);
#18481=AXIS2_PLACEMENT_3D('',#44361,#22111,#22112);
#18482=AXIS2_PLACEMENT_3D('',#44362,#22113,#22114);
#18483=AXIS2_PLACEMENT_3D('',#44363,#22115,#22116);
#18484=AXIS2_PLACEMENT_3D('',#44365,#22117,#22118);
#18485=AXIS2_PLACEMENT_3D('',#44366,#22119,#22120);
#18486=AXIS2_PLACEMENT_3D('',#44368,#22122,#22123);
#18487=AXIS2_PLACEMENT_3D('',#44369,#22124,#22125);
#18488=AXIS2_PLACEMENT_3D('',#44370,#22126,#22127);
#18489=AXIS2_PLACEMENT_3D('',#44386,#22129,#22130);
#18490=AXIS2_PLACEMENT_3D('',#44394,#22131,#22132);
#18491=AXIS2_PLACEMENT_3D('',#44442,#22134,#22135);
#18492=AXIS2_PLACEMENT_3D('',#44490,#22137,#22138);
#18493=AXIS2_PLACEMENT_3D('',#44538,#22140,#22141);
#18494=AXIS2_PLACEMENT_3D('',#44592,#22143,#22144);
#18495=AXIS2_PLACEMENT_3D('',#44640,#22146,#22147);
#18496=AXIS2_PLACEMENT_3D('',#44688,#22149,#22150);
#18497=AXIS2_PLACEMENT_3D('',#44742,#22152,#22153);
#18498=AXIS2_PLACEMENT_3D('',#44790,#22155,#22156);
#18499=AXIS2_PLACEMENT_3D('',#44838,#22158,#22159);
#18500=AXIS2_PLACEMENT_3D('',#44886,#22161,#22162);
#18501=AXIS2_PLACEMENT_3D('',#44940,#22164,#22165);
#18502=AXIS2_PLACEMENT_3D('',#44988,#22167,#22168);
#18503=AXIS2_PLACEMENT_3D('',#45036,#22170,#22171);
#18504=AXIS2_PLACEMENT_3D('',#45090,#22173,#22174);
#18505=AXIS2_PLACEMENT_3D('',#45138,#22176,#22177);
#18506=AXIS2_PLACEMENT_3D('',#45186,#22179,#22180);
#18507=AXIS2_PLACEMENT_3D('',#45234,#22182,#22183);
#18508=AXIS2_PLACEMENT_3D('',#45288,#22185,#22186);
#18509=AXIS2_PLACEMENT_3D('',#45336,#22188,#22189);
#18510=AXIS2_PLACEMENT_3D('',#45384,#22191,#22192);
#18511=AXIS2_PLACEMENT_3D('',#45438,#22194,#22195);
#18512=AXIS2_PLACEMENT_3D('',#45486,#22197,#22198);
#18513=AXIS2_PLACEMENT_3D('',#45534,#22200,#22201);
#18514=AXIS2_PLACEMENT_3D('',#45582,#22203,#22204);
#18515=AXIS2_PLACEMENT_3D('',#45636,#22206,#22207);
#18516=AXIS2_PLACEMENT_3D('',#45684,#22209,#22210);
#18517=AXIS2_PLACEMENT_3D('',#45732,#22212,#22213);
#18518=AXIS2_PLACEMENT_3D('',#45786,#22215,#22216);
#18519=AXIS2_PLACEMENT_3D('',#45834,#22218,#22219);
#18520=AXIS2_PLACEMENT_3D('',#45882,#22221,#22222);
#18521=AXIS2_PLACEMENT_3D('',#45930,#22224,#22225);
#18522=AXIS2_PLACEMENT_3D('',#45984,#22227,#22228);
#18523=AXIS2_PLACEMENT_3D('',#46032,#22230,#22231);
#18524=AXIS2_PLACEMENT_3D('',#46080,#22233,#22234);
#18525=AXIS2_PLACEMENT_3D('',#46134,#22236,#22237);
#18526=AXIS2_PLACEMENT_3D('',#46182,#22239,#22240);
#18527=AXIS2_PLACEMENT_3D('',#46230,#22242,#22243);
#18528=AXIS2_PLACEMENT_3D('',#46278,#22245,#22246);
#18529=AXIS2_PLACEMENT_3D('',#46332,#22248,#22249);
#18530=AXIS2_PLACEMENT_3D('',#46380,#22251,#22252);
#18531=AXIS2_PLACEMENT_3D('',#46428,#22254,#22255);
#18532=AXIS2_PLACEMENT_3D('',#46482,#22257,#22258);
#18533=AXIS2_PLACEMENT_3D('',#46530,#22260,#22261);
#18534=AXIS2_PLACEMENT_3D('',#46578,#22263,#22264);
#18535=AXIS2_PLACEMENT_3D('',#46626,#22266,#22267);
#18536=AXIS2_PLACEMENT_3D('',#46680,#22269,#22270);
#18537=AXIS2_PLACEMENT_3D('',#46728,#22272,#22273);
#18538=AXIS2_PLACEMENT_3D('',#46776,#22275,#22276);
#18539=AXIS2_PLACEMENT_3D('',#46830,#22278,#22279);
#18540=AXIS2_PLACEMENT_3D('',#46878,#22281,#22282);
#18541=AXIS2_PLACEMENT_3D('',#46926,#22284,#22285);
#18542=AXIS2_PLACEMENT_3D('',#46974,#22287,#22288);
#18543=AXIS2_PLACEMENT_3D('',#47028,#22290,#22291);
#18544=AXIS2_PLACEMENT_3D('',#47076,#22293,#22294);
#18545=AXIS2_PLACEMENT_3D('',#47124,#22296,#22297);
#18546=AXIS2_PLACEMENT_3D('',#47178,#22299,#22300);
#18547=AXIS2_PLACEMENT_3D('',#47226,#22302,#22303);
#18548=AXIS2_PLACEMENT_3D('',#47274,#22305,#22306);
#18549=AXIS2_PLACEMENT_3D('',#47322,#22308,#22309);
#18550=AXIS2_PLACEMENT_3D('',#47376,#22311,#22312);
#18551=AXIS2_PLACEMENT_3D('',#47424,#22314,#22315);
#18552=AXIS2_PLACEMENT_3D('',#47472,#22317,#22318);
#18553=AXIS2_PLACEMENT_3D('',#47526,#22320,#22321);
#18554=AXIS2_PLACEMENT_3D('',#47574,#22323,#22324);
#18555=AXIS2_PLACEMENT_3D('',#47622,#22326,#22327);
#18556=AXIS2_PLACEMENT_3D('',#47670,#22329,#22330);
#18557=AXIS2_PLACEMENT_3D('',#47724,#22332,#22333);
#18558=AXIS2_PLACEMENT_3D('',#47772,#22335,#22336);
#18559=AXIS2_PLACEMENT_3D('',#47820,#22338,#22339);
#18560=AXIS2_PLACEMENT_3D('',#47874,#22341,#22342);
#18561=AXIS2_PLACEMENT_3D('',#47922,#22344,#22345);
#18562=AXIS2_PLACEMENT_3D('',#47970,#22347,#22348);
#18563=AXIS2_PLACEMENT_3D('',#48018,#22350,#22351);
#18564=AXIS2_PLACEMENT_3D('',#48072,#22353,#22354);
#18565=AXIS2_PLACEMENT_3D('',#48120,#22356,#22357);
#18566=AXIS2_PLACEMENT_3D('',#48168,#22359,#22360);
#18567=AXIS2_PLACEMENT_3D('',#48222,#22362,#22363);
#18568=AXIS2_PLACEMENT_3D('',#48270,#22365,#22366);
#18569=AXIS2_PLACEMENT_3D('',#48318,#22368,#22369);
#18570=AXIS2_PLACEMENT_3D('',#48366,#22371,#22372);
#18571=AXIS2_PLACEMENT_3D('',#48420,#22374,#22375);
#18572=AXIS2_PLACEMENT_3D('',#48468,#22377,#22378);
#18573=AXIS2_PLACEMENT_3D('',#48516,#22380,#22381);
#18574=AXIS2_PLACEMENT_3D('',#48570,#22383,#22384);
#18575=AXIS2_PLACEMENT_3D('',#48618,#22386,#22387);
#18576=AXIS2_PLACEMENT_3D('',#48666,#22389,#22390);
#18577=AXIS2_PLACEMENT_3D('',#48714,#22392,#22393);
#18578=AXIS2_PLACEMENT_3D('',#48723,#22395,#22396);
#18579=AXIS2_PLACEMENT_3D('',#48724,#22397,#22398);
#18580=AXIS2_PLACEMENT_3D('',#48751,#22400,#22401);
#18581=AXIS2_PLACEMENT_3D('',#48761,#22402,#22403);
#18582=AXIS2_PLACEMENT_3D('',#48809,#22405,#22406);
#18583=AXIS2_PLACEMENT_3D('',#48857,#22408,#22409);
#18584=AXIS2_PLACEMENT_3D('',#48882,#22411,#22412);
#18585=AXIS2_PLACEMENT_3D('',#48907,#22414,#22415);
#18586=AXIS2_PLACEMENT_3D('',#48931,#22417,#22418);
#18587=AXIS2_PLACEMENT_3D('',#48956,#22420,#22421);
#18588=AXIS2_PLACEMENT_3D('',#48995,#22423,#22424);
#18589=AXIS2_PLACEMENT_3D('',#49031,#22426,#22427);
#18590=AXIS2_PLACEMENT_3D('',#49055,#22429,#22430);
#18591=AXIS2_PLACEMENT_3D('',#49080,#22432,#22433);
#18592=AXIS2_PLACEMENT_3D('',#49105,#22435,#22436);
#18593=AXIS2_PLACEMENT_3D('',#49129,#22438,#22439);
#18594=AXIS2_PLACEMENT_3D('',#49154,#22441,#22442);
#18595=AXIS2_PLACEMENT_3D('',#49179,#22444,#22445);
#18596=AXIS2_PLACEMENT_3D('',#49215,#22447,#22448);
#18597=AXIS2_PLACEMENT_3D('',#49251,#22450,#22451);
#18598=AXIS2_PLACEMENT_3D('',#49276,#22453,#22454);
#18599=AXIS2_PLACEMENT_3D('',#49301,#22456,#22457);
#18600=AXIS2_PLACEMENT_3D('',#49325,#22459,#22460);
#18601=AXIS2_PLACEMENT_3D('',#49350,#22462,#22463);
#18602=AXIS2_PLACEMENT_3D('',#49375,#22465,#22466);
#18603=AXIS2_PLACEMENT_3D('',#49399,#22468,#22469);
#18604=AXIS2_PLACEMENT_3D('',#49423,#22471,#22472);
#18605=AXIS2_PLACEMENT_3D('',#49448,#22474,#22475);
#18606=AXIS2_PLACEMENT_3D('',#49473,#22477,#22478);
#18607=AXIS2_PLACEMENT_3D('',#49497,#22480,#22481);
#18608=AXIS2_PLACEMENT_3D('',#49522,#22483,#22484);
#18609=AXIS2_PLACEMENT_3D('',#49547,#22486,#22487);
#18610=AXIS2_PLACEMENT_3D('',#49571,#22489,#22490);
#18611=AXIS2_PLACEMENT_3D('',#49595,#22492,#22493);
#18612=AXIS2_PLACEMENT_3D('',#49620,#22495,#22496);
#18613=AXIS2_PLACEMENT_3D('',#49645,#22498,#22499);
#18614=AXIS2_PLACEMENT_3D('',#49669,#22501,#22502);
#18615=AXIS2_PLACEMENT_3D('',#49694,#22504,#22505);
#18616=AXIS2_PLACEMENT_3D('',#49719,#22507,#22508);
#18617=AXIS2_PLACEMENT_3D('',#49743,#22510,#22511);
#18618=AXIS2_PLACEMENT_3D('',#49767,#22513,#22514);
#18619=AXIS2_PLACEMENT_3D('',#49792,#22516,#22517);
#18620=AXIS2_PLACEMENT_3D('',#49817,#22519,#22520);
#18621=AXIS2_PLACEMENT_3D('',#49841,#22522,#22523);
#18622=AXIS2_PLACEMENT_3D('',#49866,#22525,#22526);
#18623=AXIS2_PLACEMENT_3D('',#49891,#22528,#22529);
#18624=AXIS2_PLACEMENT_3D('',#49915,#22531,#22532);
#18625=AXIS2_PLACEMENT_3D('',#49939,#22534,#22535);
#18626=AXIS2_PLACEMENT_3D('',#49964,#22537,#22538);
#18627=AXIS2_PLACEMENT_3D('',#49989,#22540,#22541);
#18628=AXIS2_PLACEMENT_3D('',#50013,#22543,#22544);
#18629=AXIS2_PLACEMENT_3D('',#50038,#22546,#22547);
#18630=AXIS2_PLACEMENT_3D('',#50063,#22549,#22550);
#18631=AXIS2_PLACEMENT_3D('',#50087,#22552,#22553);
#18632=AXIS2_PLACEMENT_3D('',#50111,#22555,#22556);
#18633=AXIS2_PLACEMENT_3D('',#50136,#22558,#22559);
#18634=AXIS2_PLACEMENT_3D('',#50161,#22561,#22562);
#18635=AXIS2_PLACEMENT_3D('',#50185,#22564,#22565);
#18636=AXIS2_PLACEMENT_3D('',#50210,#22567,#22568);
#18637=AXIS2_PLACEMENT_3D('',#50235,#22570,#22571);
#18638=AXIS2_PLACEMENT_3D('',#50259,#22573,#22574);
#18639=AXIS2_PLACEMENT_3D('',#50283,#22576,#22577);
#18640=AXIS2_PLACEMENT_3D('',#50308,#22579,#22580);
#18641=AXIS2_PLACEMENT_3D('',#50333,#22582,#22583);
#18642=AXIS2_PLACEMENT_3D('',#50357,#22585,#22586);
#18643=AXIS2_PLACEMENT_3D('',#50382,#22588,#22589);
#18644=AXIS2_PLACEMENT_3D('',#50407,#22591,#22592);
#18645=AXIS2_PLACEMENT_3D('',#50431,#22594,#22595);
#18646=AXIS2_PLACEMENT_3D('',#50455,#22597,#22598);
#18647=AXIS2_PLACEMENT_3D('',#50480,#22600,#22601);
#18648=AXIS2_PLACEMENT_3D('',#50505,#22603,#22604);
#18649=AXIS2_PLACEMENT_3D('',#50529,#22606,#22607);
#18650=AXIS2_PLACEMENT_3D('',#50554,#22609,#22610);
#18651=AXIS2_PLACEMENT_3D('',#50579,#22612,#22613);
#18652=AXIS2_PLACEMENT_3D('',#50603,#22615,#22616);
#18653=AXIS2_PLACEMENT_3D('',#50627,#22618,#22619);
#18654=AXIS2_PLACEMENT_3D('',#50652,#22621,#22622);
#18655=AXIS2_PLACEMENT_3D('',#50677,#22624,#22625);
#18656=AXIS2_PLACEMENT_3D('',#50701,#22627,#22628);
#18657=AXIS2_PLACEMENT_3D('',#50726,#22630,#22631);
#18658=AXIS2_PLACEMENT_3D('',#50751,#22633,#22634);
#18659=AXIS2_PLACEMENT_3D('',#50775,#22636,#22637);
#18660=AXIS2_PLACEMENT_3D('',#50799,#22639,#22640);
#18661=AXIS2_PLACEMENT_3D('',#50824,#22642,#22643);
#18662=AXIS2_PLACEMENT_3D('',#50849,#22645,#22646);
#18663=AXIS2_PLACEMENT_3D('',#50873,#22648,#22649);
#18664=AXIS2_PLACEMENT_3D('',#50898,#22651,#22652);
#18665=AXIS2_PLACEMENT_3D('',#50923,#22654,#22655);
#18666=AXIS2_PLACEMENT_3D('',#50947,#22657,#22658);
#18667=AXIS2_PLACEMENT_3D('',#53413,#22660,#22661);
#18668=AXIS2_PLACEMENT_3D('',#53415,#22662,#22663);
#18669=AXIS2_PLACEMENT_3D('',#53416,#22664,#22665);
#18670=AXIS2_PLACEMENT_3D('',#53515,#22666,#22667);
#18671=AXIS2_PLACEMENT_3D('',#53516,#22668,#22669);
#18672=AXIS2_PLACEMENT_3D('',#55857,#22670,#22671);
#18673=AXIS2_PLACEMENT_3D('',#55881,#22673,#22674);
#18674=AXIS2_PLACEMENT_3D('',#55889,#22675,#22676);
#18675=AXIS2_PLACEMENT_3D('',#55895,#22680,#22681);
#18676=AXIS2_PLACEMENT_3D('',#55899,#22684,#22685);
#18677=AXIS2_PLACEMENT_3D('',#55903,#22688,#22689);
#18678=AXIS2_PLACEMENT_3D('',#55909,#22693,#22694);
#18679=AXIS2_PLACEMENT_3D('',#55910,#22695,#22696);
#18680=AXIS2_PLACEMENT_3D('',#55912,#22698,#22699);
#18681=AXIS2_PLACEMENT_3D('',#55914,#22701,#22702);
#18682=AXIS2_PLACEMENT_3D('',#55915,#22703,#22704);
#18683=AXIS2_PLACEMENT_3D('',#55916,#22705,#22706);
#18684=AXIS2_PLACEMENT_3D('',#55918,#22707,#22708);
#18685=AXIS2_PLACEMENT_3D('',#55919,#22709,#22710);
#18686=AXIS2_PLACEMENT_3D('',#55921,#22712,#22713);
#18687=AXIS2_PLACEMENT_3D('',#55922,#22714,#22715);
#18688=AXIS2_PLACEMENT_3D('',#55923,#22716,#22717);
#18689=AXIS2_PLACEMENT_3D('',#55925,#22718,#22719);
#18690=AXIS2_PLACEMENT_3D('',#55949,#22721,#22722);
#18691=AXIS2_PLACEMENT_3D('',#55983,#22723,#22724);
#18692=AXIS2_PLACEMENT_3D('',#56017,#22725,#22726);
#18693=AXIS2_PLACEMENT_3D('',#56051,#22727,#22728);
#18694=AXIS2_PLACEMENT_3D('',#56085,#22729,#22730);
#18695=AXIS2_PLACEMENT_3D('',#56119,#22731,#22732);
#18696=AXIS2_PLACEMENT_3D('',#56233,#22733,#22734);
#18697=AXIS2_PLACEMENT_3D('',#56234,#22735,#22736);
#18698=AXIS2_PLACEMENT_3D('',#56239,#22737,#22738);
#18699=AXIS2_PLACEMENT_3D('',#56249,#22739,#22740);
#18700=AXIS2_PLACEMENT_3D('',#56259,#22741,#22742);
#18701=AXIS2_PLACEMENT_3D('',#56269,#22743,#22744);
#18702=AXIS2_PLACEMENT_3D('',#56313,#22745,#22746);
#18703=AXIS2_PLACEMENT_3D('',#56315,#22747,#22748);
#18704=AXIS2_PLACEMENT_3D('',#56316,#22749,#22750);
#18705=AXIS2_PLACEMENT_3D('',#56318,#22752,#22753);
#18706=AXIS2_PLACEMENT_3D('',#56327,#22755,#22756);
#18707=AXIS2_PLACEMENT_3D('',#56329,#22758,#22759);
#18708=AXIS2_PLACEMENT_3D('',#56345,#22761,#22762);
#18709=AXIS2_PLACEMENT_3D('',#56354,#22764,#22765);
#18710=AXIS2_PLACEMENT_3D('',#56395,#22767,#22768);
#18711=AXIS2_PLACEMENT_3D('',#56428,#22771,#22772);
#18712=AXIS2_PLACEMENT_3D('',#56436,#22775,#22776);
#18713=AXIS2_PLACEMENT_3D('',#56469,#22779,#22780);
#18714=AXIS2_PLACEMENT_3D('',#56477,#22783,#22784);
#18715=AXIS2_PLACEMENT_3D('',#56485,#22787,#22788);
#18716=AXIS2_PLACEMENT_3D('',#56493,#22791,#22792);
#18717=AXIS2_PLACEMENT_3D('',#56497,#22793,#22794);
#18718=AXIS2_PLACEMENT_3D('',#56501,#22795,#22796);
#18719=AXIS2_PLACEMENT_3D('',#56505,#22797,#22798);
#18720=AXIS2_PLACEMENT_3D('',#56507,#22799,#22800);
#18721=AXIS2_PLACEMENT_3D('',#56522,#22802,#22803);
#18722=AXIS2_PLACEMENT_3D('',#56524,#22804,#22805);
#18723=AXIS2_PLACEMENT_3D('',#56527,#22807,#22808);
#18724=AXIS2_PLACEMENT_3D('',#56528,#22809,#22810);
#18725=AXIS2_PLACEMENT_3D('',#56531,#22812,#22813);
#18726=AXIS2_PLACEMENT_3D('',#56532,#22814,#22815);
#18727=AXIS2_PLACEMENT_3D('',#56534,#22817,#22818);
#18728=AXIS2_PLACEMENT_3D('',#56535,#22819,#22820);
#18729=AXIS2_PLACEMENT_3D('',#56536,#22821,#22822);
#18730=AXIS2_PLACEMENT_3D('',#56537,#22823,#22824);
#18731=AXIS2_PLACEMENT_3D('',#56538,#22825,#22826);
#18732=AXIS2_PLACEMENT_3D('',#56539,#22827,#22828);
#18733=AXIS2_PLACEMENT_3D('',#56540,#22829,#22830);
#18734=AXIS2_PLACEMENT_3D('',#56541,#22831,#22832);
#18735=AXIS2_PLACEMENT_3D('',#56542,#22833,#22834);
#18736=AXIS2_PLACEMENT_3D('',#56543,#22835,#22836);
#18737=AXIS2_PLACEMENT_3D('',#56544,#22837,#22838);
#18738=AXIS2_PLACEMENT_3D('',#56545,#22839,#22840);
#18739=AXIS2_PLACEMENT_3D('',#56546,#22841,#22842);
#18740=AXIS2_PLACEMENT_3D('',#56547,#22843,#22844);
#18741=AXIS2_PLACEMENT_3D('',#56548,#22845,#22846);
#18742=AXIS2_PLACEMENT_3D('',#56549,#22847,#22848);
#18743=AXIS2_PLACEMENT_3D('',#56550,#22849,#22850);
#18744=AXIS2_PLACEMENT_3D('',#56551,#22851,#22852);
#18745=AXIS2_PLACEMENT_3D('',#56552,#22853,#22854);
#18746=AXIS2_PLACEMENT_3D('',#56553,#22855,#22856);
#18747=AXIS2_PLACEMENT_3D('',#56554,#22857,#22858);
#18748=AXIS2_PLACEMENT_3D('',#56555,#22859,#22860);
#18749=AXIS2_PLACEMENT_3D('',#56556,#22861,#22862);
#18750=AXIS2_PLACEMENT_3D('',#56557,#22863,#22864);
#18751=AXIS2_PLACEMENT_3D('',#56558,#22865,#22866);
#18752=AXIS2_PLACEMENT_3D('',#56559,#22867,#22868);
#18753=AXIS2_PLACEMENT_3D('',#56560,#22869,#22870);
#18754=AXIS2_PLACEMENT_3D('',#56561,#22871,#22872);
#18755=AXIS2_PLACEMENT_3D('',#56562,#22873,#22874);
#18756=AXIS2_PLACEMENT_3D('',#56563,#22875,#22876);
#18757=AXIS2_PLACEMENT_3D('',#56564,#22877,#22878);
#18758=AXIS2_PLACEMENT_3D('',#56565,#22879,#22880);
#18759=AXIS2_PLACEMENT_3D('',#56566,#22881,#22882);
#18760=AXIS2_PLACEMENT_3D('',#56567,#22883,#22884);
#18761=AXIS2_PLACEMENT_3D('',#56568,#22885,#22886);
#18762=AXIS2_PLACEMENT_3D('',#56569,#22887,#22888);
#18763=AXIS2_PLACEMENT_3D('',#56570,#22889,#22890);
#18764=AXIS2_PLACEMENT_3D('',#56571,#22891,#22892);
#18765=AXIS2_PLACEMENT_3D('',#56572,#22893,#22894);
#18766=AXIS2_PLACEMENT_3D('',#56573,#22895,#22896);
#18767=AXIS2_PLACEMENT_3D('',#56574,#22897,#22898);
#18768=AXIS2_PLACEMENT_3D('',#56575,#22899,#22900);
#18769=AXIS2_PLACEMENT_3D('',#56576,#22901,#22902);
#18770=AXIS2_PLACEMENT_3D('',#56577,#22903,#22904);
#18771=AXIS2_PLACEMENT_3D('',#56578,#22905,#22906);
#18772=AXIS2_PLACEMENT_3D('',#56579,#22907,#22908);
#18773=AXIS2_PLACEMENT_3D('',#56580,#22909,#22910);
#18774=AXIS2_PLACEMENT_3D('',#56581,#22911,#22912);
#18775=AXIS2_PLACEMENT_3D('',#56582,#22913,#22914);
#18776=AXIS2_PLACEMENT_3D('',#56583,#22915,#22916);
#18777=AXIS2_PLACEMENT_3D('',#56584,#22917,#22918);
#18778=AXIS2_PLACEMENT_3D('',#56585,#22919,#22920);
#18779=AXIS2_PLACEMENT_3D('',#56586,#22921,#22922);
#18780=AXIS2_PLACEMENT_3D('',#56587,#22923,#22924);
#18781=AXIS2_PLACEMENT_3D('',#56588,#22925,#22926);
#18782=AXIS2_PLACEMENT_3D('',#56589,#22927,#22928);
#18783=AXIS2_PLACEMENT_3D('',#56590,#22929,#22930);
#18784=AXIS2_PLACEMENT_3D('',#56591,#22931,#22932);
#18785=AXIS2_PLACEMENT_3D('',#56592,#22933,#22934);
#18786=AXIS2_PLACEMENT_3D('',#56593,#22935,#22936);
#18787=AXIS2_PLACEMENT_3D('',#56594,#22937,#22938);
#18788=AXIS2_PLACEMENT_3D('',#56595,#22939,#22940);
#18789=DIRECTION('axis',(0.,0.,1.));
#18790=DIRECTION('refdir',(1.,0.,0.));
#18791=DIRECTION('axis',(0.,0.,1.));
#18792=DIRECTION('refdir',(1.,0.,0.));
#18793=DIRECTION('center_axis',(0.331061386243095,0.943609219189173,0.));
#18794=DIRECTION('ref_axis',(0.,0.,1.));
#18795=DIRECTION('',(0.,0.,1.));
#18796=DIRECTION('',(-0.943609219189173,0.331061386243095,0.));
#18797=DIRECTION('',(0.,0.,-1.));
#18798=DIRECTION('center_axis',(0.,1.,0.));
#18799=DIRECTION('ref_axis',(-1.,0.,0.));
#18800=DIRECTION('',(-1.,0.,0.));
#18801=DIRECTION('',(-1.,0.,0.));
#18802=DIRECTION('',(0.,0.,1.));
#18803=DIRECTION('',(0.,0.,1.));
#18804=DIRECTION('',(-1.,0.,0.));
#18805=DIRECTION('',(0.,0.,-1.));
#18806=DIRECTION('center_axis',(-0.331061386243095,0.943609219189173,0.));
#18807=DIRECTION('ref_axis',(0.,0.,1.));
#18808=DIRECTION('',(0.,0.,1.));
#18809=DIRECTION('',(-0.943609219189173,-0.331061386243095,0.));
#18810=DIRECTION('center_axis',(0.,0.,1.));
#18811=DIRECTION('ref_axis',(1.,0.,0.));
#18812=DIRECTION('center_axis',(0.,0.,1.));
#18813=DIRECTION('ref_axis',(1.,0.,0.));
#18814=DIRECTION('',(0.,0.,1.));
#18815=DIRECTION('center_axis',(0.,0.,-1.));
#18816=DIRECTION('ref_axis',(0.,1.,0.));
#18817=DIRECTION('center_axis',(0.,0.,1.));
#18818=DIRECTION('ref_axis',(1.,0.,0.));
#18819=DIRECTION('center_axis',(0.,0.,-1.));
#18820=DIRECTION('ref_axis',(0.,1.,0.));
#18821=DIRECTION('center_axis',(-0.331061386243095,-0.943609219189173,0.));
#18822=DIRECTION('ref_axis',(0.,0.,-1.));
#18823=DIRECTION('',(0.,0.,1.));
#18824=DIRECTION('',(0.943609219189173,-0.331061386243095,0.));
#18825=DIRECTION('',(0.,0.,-1.));
#18826=DIRECTION('center_axis',(0.,-1.,0.));
#18827=DIRECTION('ref_axis',(1.,0.,0.));
#18828=DIRECTION('',(1.,0.,0.));
#18829=DIRECTION('',(1.,0.,0.));
#18830=DIRECTION('',(0.,0.,1.));
#18831=DIRECTION('',(0.,0.,1.));
#18832=DIRECTION('',(1.,0.,0.));
#18833=DIRECTION('',(0.,0.,-1.));
#18834=DIRECTION('center_axis',(0.331061386243095,-0.943609219189173,0.));
#18835=DIRECTION('ref_axis',(0.,0.,-1.));
#18836=DIRECTION('',(0.,0.,1.));
#18837=DIRECTION('',(0.943609219189173,0.331061386243095,0.));
#18838=DIRECTION('center_axis',(0.,0.,1.));
#18839=DIRECTION('ref_axis',(1.,0.,0.));
#18840=DIRECTION('center_axis',(0.,0.,1.));
#18841=DIRECTION('ref_axis',(1.,0.,0.));
#18842=DIRECTION('',(0.,0.,1.));
#18843=DIRECTION('center_axis',(0.,0.,-1.));
#18844=DIRECTION('ref_axis',(0.,-1.,0.));
#18845=DIRECTION('center_axis',(0.,0.,1.));
#18846=DIRECTION('ref_axis',(1.,0.,0.));
#18847=DIRECTION('center_axis',(0.,0.,-1.));
#18848=DIRECTION('ref_axis',(0.,-1.,0.));
#18849=DIRECTION('center_axis',(0.,0.,-1.));
#18850=DIRECTION('ref_axis',(1.,0.,0.));
#18851=DIRECTION('center_axis',(0.,0.,-1.));
#18852=DIRECTION('ref_axis',(1.,0.,0.));
#18853=DIRECTION('',(0.707106781186547,-8.65956056235493E-17,0.707106781186547));
#18854=DIRECTION('center_axis',(0.,0.,1.));
#18855=DIRECTION('ref_axis',(1.,0.,0.));
#18856=DIRECTION('center_axis',(0.,0.,1.));
#18857=DIRECTION('ref_axis',(0.707106781186548,0.707106781186548,0.));
#18858=DIRECTION('',(0.,1.,0.));
#18859=DIRECTION('center_axis',(0.,0.,1.));
#18860=DIRECTION('ref_axis',(0.707106781186548,-0.707106781186547,0.));
#18861=DIRECTION('',(1.,0.,0.));
#18862=DIRECTION('center_axis',(0.,0.,1.));
#18863=DIRECTION('ref_axis',(-0.707106781186548,-0.707106781186548,0.));
#18864=DIRECTION('',(0.,-1.,0.));
#18865=DIRECTION('center_axis',(0.,0.,1.));
#18866=DIRECTION('ref_axis',(-0.707106781186548,0.707106781186548,0.));
#18867=DIRECTION('',(-1.,0.,0.));
#18868=DIRECTION('center_axis',(0.,0.,-1.));
#18869=DIRECTION('ref_axis',(1.,0.,0.));
#18870=DIRECTION('center_axis',(0.,0.,1.));
#18871=DIRECTION('ref_axis',(1.,0.,0.));
#18872=DIRECTION('center_axis',(0.,0.,-1.));
#18873=DIRECTION('ref_axis',(1.,0.,0.));
#18874=DIRECTION('',(0.707106781186547,-8.65956056235493E-17,0.707106781186547));
#18875=DIRECTION('center_axis',(0.,0.,1.));
#18876=DIRECTION('ref_axis',(1.,0.,0.));
#18877=DIRECTION('center_axis',(0.,0.,1.));
#18878=DIRECTION('ref_axis',(1.,0.,0.));
#18879=DIRECTION('',(0.707106781186541,8.65956056235486E-17,-0.707106781186554));
#18880=DIRECTION('center_axis',(0.,0.,-1.));
#18881=DIRECTION('ref_axis',(1.,0.,0.));
#18882=DIRECTION('center_axis',(0.,0.,1.));
#18883=DIRECTION('ref_axis',(1.,0.,0.));
#18884=DIRECTION('',(0.,-1.,0.));
#18885=DIRECTION('center_axis',(0.,0.,-1.));
#18886=DIRECTION('ref_axis',(0.707106781186548,0.707106781186548,0.));
#18887=DIRECTION('',(1.,0.,0.));
#18888=DIRECTION('center_axis',(0.,0.,-1.));
#18889=DIRECTION('ref_axis',(-0.707106781186548,0.707106781186548,0.));
#18890=DIRECTION('',(0.,1.,0.));
#18891=DIRECTION('center_axis',(0.,0.,-1.));
#18892=DIRECTION('ref_axis',(-0.707106781186548,-0.707106781186548,0.));
#18893=DIRECTION('',(-1.,0.,0.));
#18894=DIRECTION('center_axis',(0.,0.,-1.));
#18895=DIRECTION('ref_axis',(0.707106781186548,-0.707106781186547,0.));
#18896=DIRECTION('center_axis',(0.,0.,1.));
#18897=DIRECTION('ref_axis',(1.,0.,0.));
#18898=DIRECTION('center_axis',(0.,0.,-1.));
#18899=DIRECTION('ref_axis',(1.,0.,0.));
#18900=DIRECTION('center_axis',(0.,0.,-1.));
#18901=DIRECTION('ref_axis',(1.,0.,0.));
#18902=DIRECTION('',(0.,0.,-1.));
#18903=DIRECTION('center_axis',(0.,0.,-1.));
#18904=DIRECTION('ref_axis',(1.,0.,0.));
#18905=DIRECTION('center_axis',(0.,0.,1.));
#18906=DIRECTION('ref_axis',(1.,0.,0.));
#18907=DIRECTION('',(0.707106781186541,8.65956056235486E-17,-0.707106781186554));
#18908=DIRECTION('center_axis',(0.,0.,-1.));
#18909=DIRECTION('ref_axis',(1.,0.,0.));
#18910=DIRECTION('center_axis',(0.,0.,-1.));
#18911=DIRECTION('ref_axis',(1.,0.,0.));
#18912=DIRECTION('',(0.,0.,-1.));
#18913=DIRECTION('center_axis',(0.,0.,-1.));
#18914=DIRECTION('ref_axis',(1.,0.,0.));
#18915=DIRECTION('center_axis',(1.,0.,0.));
#18916=DIRECTION('ref_axis',(0.,0.,-1.));
#18917=DIRECTION('center_axis',(1.,0.,0.));
#18918=DIRECTION('ref_axis',(0.,1.,1.41638472441199E-16));
#18919=DIRECTION('center_axis',(-1.,0.,0.));
#18920=DIRECTION('ref_axis',(0.,1.,1.41638472441199E-16));
#18921=DIRECTION('center_axis',(-1.,0.,0.));
#18922=DIRECTION('ref_axis',(0.,1.,0.));
#18923=DIRECTION('center_axis',(1.,0.,0.));
#18924=DIRECTION('ref_axis',(0.,0.,-1.));
#18925=DIRECTION('center_axis',(1.,0.,0.));
#18926=DIRECTION('ref_axis',(0.,0.,-1.));
#18927=DIRECTION('center_axis',(1.,0.,0.));
#18928=DIRECTION('ref_axis',(0.,-1.,3.06161699786838E-17));
#18929=DIRECTION('center_axis',(-1.,0.,0.));
#18930=DIRECTION('ref_axis',(0.,-1.,3.06161699786838E-17));
#18931=DIRECTION('center_axis',(-1.,0.,0.));
#18932=DIRECTION('ref_axis',(0.,-1.,3.06161699786838E-17));
#18933=DIRECTION('center_axis',(-1.,0.,0.));
#18934=DIRECTION('ref_axis',(0.,-1.,1.22464679914735E-16));
#18935=DIRECTION('center_axis',(1.,0.,0.));
#18936=DIRECTION('ref_axis',(0.,0.,-1.));
#18937=DIRECTION('center_axis',(1.,0.,0.));
#18938=DIRECTION('ref_axis',(0.,0.,-1.));
#18939=DIRECTION('center_axis',(-1.,0.,0.));
#18940=DIRECTION('ref_axis',(0.,-1.,1.83697019872103E-16));
#18941=DIRECTION('center_axis',(0.,-1.,-1.22464679914735E-16));
#18942=DIRECTION('ref_axis',(0.,-1.22464679914735E-16,1.));
#18943=DIRECTION('center_axis',(1.,0.,0.));
#18944=DIRECTION('ref_axis',(0.,-1.,3.06161699786838E-17));
#18945=DIRECTION('center_axis',(1.,0.,0.));
#18946=DIRECTION('ref_axis',(0.,-1.,3.06161699786838E-17));
#18947=DIRECTION('center_axis',(-1.,0.,0.));
#18948=DIRECTION('ref_axis',(0.,1.,0.));
#18949=DIRECTION('',(-0.64018439966448,-0.768221279597376,-9.4079973109581E-17));
#18950=DIRECTION('center_axis',(1.,0.,0.));
#18951=DIRECTION('ref_axis',(0.,1.,0.));
#18952=DIRECTION('center_axis',(1.,0.,0.));
#18953=DIRECTION('ref_axis',(0.,1.,0.));
#18954=DIRECTION('center_axis',(1.,0.,0.));
#18955=DIRECTION('ref_axis',(0.,0.,-1.));
#18956=DIRECTION('',(0.,-1.77635683940025E-16,-1.));
#18957=DIRECTION('',(0.,-1.,0.));
#18958=DIRECTION('',(0.,1.99840144432528E-16,1.));
#18959=DIRECTION('',(0.,1.,0.));
#18960=DIRECTION('',(0.,0.866025403784439,0.5));
#18961=DIRECTION('',(0.,0.5,-0.866025403784438));
#18962=DIRECTION('',(0.,-0.866025403784439,-0.5));
#18963=DIRECTION('',(0.,-0.5,0.866025403784439));
#18964=DIRECTION('',(0.,6.66133814775094E-17,1.));
#18965=DIRECTION('',(0.,1.,0.));
#18966=DIRECTION('',(0.,-7.7715611723761E-17,-1.));
#18967=DIRECTION('',(0.,-1.,0.));
#18968=DIRECTION('',(0.,-0.866025403784439,0.5));
#18969=DIRECTION('',(0.,0.5,0.866025403784438));
#18970=DIRECTION('',(0.,0.866025403784439,-0.5));
#18971=DIRECTION('',(0.,-0.5,-0.866025403784439));
#18972=DIRECTION('',(0.,-0.866025403784439,-0.5));
#18973=DIRECTION('',(0.,-0.499999999999999,0.866025403784439));
#18974=DIRECTION('',(0.,0.866025403784439,0.5));
#18975=DIRECTION('',(0.,0.5,-0.866025403784439));
#18976=DIRECTION('',(0.,0.866025403784438,-0.5));
#18977=DIRECTION('',(0.,-0.500000000000001,-0.866025403784438));
#18978=DIRECTION('',(0.,-0.866025403784438,0.5));
#18979=DIRECTION('',(0.,0.5,0.866025403784438));
#18980=DIRECTION('center_axis',(1.,0.,0.));
#18981=DIRECTION('ref_axis',(0.,-0.999985032132206,0.00547133544502502));
#18982=DIRECTION('center_axis',(-1.,0.,0.));
#18983=DIRECTION('ref_axis',(0.,-0.999998948230417,0.00145035790781154));
#18984=DIRECTION('center_axis',(-1.,0.,0.));
#18985=DIRECTION('ref_axis',(0.,0.999955202286269,-0.00946538011005637));
#18986=DIRECTION('center_axis',(1.,0.,0.));
#18987=DIRECTION('ref_axis',(0.,0.,-1.));
#18988=DIRECTION('',(0.,1.,0.));
#18989=DIRECTION('',(0.,0.,1.));
#18990=DIRECTION('',(0.,0.,1.));
#18991=DIRECTION('',(0.,-1.,0.));
#18992=DIRECTION('center_axis',(-1.,0.,0.));
#18993=DIRECTION('ref_axis',(0.,0.,-1.));
#18994=DIRECTION('center_axis',(-1.,0.,0.));
#18995=DIRECTION('ref_axis',(0.,0.,-1.));
#18996=DIRECTION('center_axis',(-1.,0.,0.));
#18997=DIRECTION('ref_axis',(0.,0.,-1.));
#18998=DIRECTION('center_axis',(1.,0.,0.));
#18999=DIRECTION('ref_axis',(0.,0.,-1.));
#19000=DIRECTION('center_axis',(1.,0.,0.));
#19001=DIRECTION('ref_axis',(0.,-0.999998948230417,0.00145035790781157));
#19002=DIRECTION('center_axis',(1.,0.,0.));
#19003=DIRECTION('ref_axis',(0.,-0.999998948230417,0.00145035790781157));
#19004=DIRECTION('center_axis',(1.,0.,0.));
#19005=DIRECTION('ref_axis',(0.,1.,0.));
#19006=DIRECTION('center_axis',(-1.,0.,0.));
#19007=DIRECTION('ref_axis',(0.,1.,0.));
#19008=DIRECTION('center_axis',(1.,0.,0.));
#19009=DIRECTION('ref_axis',(0.,0.999998948230416,0.00145035790796071));
#19010=DIRECTION('center_axis',(-1.,0.,0.));
#19011=DIRECTION('ref_axis',(0.,1.,0.));
#19012=DIRECTION('',(-1.,0.,0.));
#19013=DIRECTION('center_axis',(-1.,0.,0.));
#19014=DIRECTION('ref_axis',(0.,1.,1.22464679914735E-16));
#19015=DIRECTION('center_axis',(1.,0.,0.));
#19016=DIRECTION('ref_axis',(0.,0.999985032132206,0.00547133544502336));
#19017=DIRECTION('center_axis',(-1.,0.,0.));
#19018=DIRECTION('ref_axis',(0.,0.999998948230416,0.00145035790796071));
#19019=DIRECTION('center_axis',(-1.,0.,0.));
#19020=DIRECTION('ref_axis',(0.,-0.999955202286269,-0.00946538011005535));
#19021=DIRECTION('center_axis',(1.,0.,0.));
#19022=DIRECTION('ref_axis',(0.,0.,-1.));
#19023=DIRECTION('',(0.,-1.,0.));
#19024=DIRECTION('',(0.,0.,-1.));
#19025=DIRECTION('',(0.,0.,-1.));
#19026=DIRECTION('',(0.,1.,0.));
#19027=DIRECTION('center_axis',(-1.,0.,0.));
#19028=DIRECTION('ref_axis',(0.,0.,-1.));
#19029=DIRECTION('center_axis',(-1.,0.,0.));
#19030=DIRECTION('ref_axis',(0.,0.,-1.));
#19031=DIRECTION('center_axis',(-1.,0.,0.));
#19032=DIRECTION('ref_axis',(0.,0.,-1.));
#19033=DIRECTION('center_axis',(-1.,0.,0.));
#19034=DIRECTION('ref_axis',(0.,0.,1.));
#19035=DIRECTION('center_axis',(1.,0.,0.));
#19036=DIRECTION('ref_axis',(0.,1.,1.22464679914735E-16));
#19037=DIRECTION('center_axis',(0.,0.,-1.));
#19038=DIRECTION('ref_axis',(0.,-1.,0.));
#19039=DIRECTION('center_axis',(1.,0.,0.));
#19040=DIRECTION('ref_axis',(0.,1.,1.22464679914735E-16));
#19041=DIRECTION('center_axis',(-1.,0.,0.));
#19042=DIRECTION('ref_axis',(0.,0.,1.));
#19043=DIRECTION('center_axis',(1.,0.,0.));
#19044=DIRECTION('ref_axis',(0.,0.,-1.));
#19045=DIRECTION('center_axis',(1.,0.,0.));
#19046=DIRECTION('ref_axis',(0.,0.,-1.));
#19047=DIRECTION('center_axis',(1.,0.,0.));
#19048=DIRECTION('ref_axis',(0.,0.,-1.));
#19049=DIRECTION('center_axis',(1.,0.,0.));
#19050=DIRECTION('ref_axis',(0.,0.,-1.));
#19051=DIRECTION('center_axis',(1.,0.,0.));
#19052=DIRECTION('ref_axis',(0.,0.,-1.));
#19053=DIRECTION('center_axis',(1.,0.,0.));
#19054=DIRECTION('ref_axis',(0.,0.,-1.));
#19055=DIRECTION('center_axis',(-1.,0.,0.));
#19056=DIRECTION('ref_axis',(0.,1.,0.));
#19057=DIRECTION('center_axis',(0.,0.,1.));
#19058=DIRECTION('ref_axis',(1.,0.,0.));
#19059=DIRECTION('center_axis',(0.,0.,1.));
#19060=DIRECTION('ref_axis',(-0.309915766398542,-0.950764017902237,0.));
#19061=DIRECTION('center_axis',(-1.,0.,0.));
#19062=DIRECTION('ref_axis',(0.,0.,-1.));
#19063=DIRECTION('center_axis',(0.,0.,-1.));
#19064=DIRECTION('ref_axis',(-0.309915766398542,-0.950764017902237,0.));
#19065=DIRECTION('center_axis',(1.,0.,0.));
#19066=DIRECTION('ref_axis',(0.,-0.707106781186546,-0.707106781186549));
#19067=DIRECTION('center_axis',(-1.,0.,0.));
#19068=DIRECTION('ref_axis',(0.,0.,-1.));
#19069=DIRECTION('',(-1.,0.,0.));
#19070=DIRECTION('',(1.,0.,0.));
#19071=DIRECTION('center_axis',(0.,0.,1.));
#19072=DIRECTION('ref_axis',(1.,0.,0.));
#19073=DIRECTION('center_axis',(0.,-1.,0.));
#19074=DIRECTION('ref_axis',(0.,0.,-1.));
#19075=DIRECTION('center_axis',(0.,0.,-1.));
#19076=DIRECTION('ref_axis',(0.707106781186548,-0.707106781186547,0.));
#19077=DIRECTION('center_axis',(0.,0.,1.));
#19078=DIRECTION('ref_axis',(0.707106781186548,-0.707106781186547,0.));
#19079=DIRECTION('center_axis',(0.,1.,0.));
#19080=DIRECTION('ref_axis',(0.707106781186544,0.,-0.707106781186551));
#19081=DIRECTION('',(0.,-1.,0.));
#19082=DIRECTION('',(0.,1.,0.));
#19083=DIRECTION('center_axis',(1.,0.,0.));
#19084=DIRECTION('ref_axis',(0.,1.,0.));
#19085=DIRECTION('',(0.,0.,1.));
#19086=DIRECTION('',(0.,0.,1.));
#19087=DIRECTION('',(0.,-1.,0.));
#19088=DIRECTION('',(0.,0.,1.));
#19089=DIRECTION('',(0.,1.,0.));
#19090=DIRECTION('',(0.,0.,1.));
#19091=DIRECTION('center_axis',(0.,0.,1.));
#19092=DIRECTION('ref_axis',(1.,0.,0.));
#19093=DIRECTION('center_axis',(0.,0.,-1.));
#19094=DIRECTION('ref_axis',(-1.,0.,0.));
#19095=DIRECTION('',(-1.,0.,0.));
#19096=DIRECTION('center_axis',(0.,0.,-1.));
#19097=DIRECTION('ref_axis',(2.22044604925031E-15,-1.,0.));
#19098=DIRECTION('center_axis',(0.,1.,0.));
#19099=DIRECTION('ref_axis',(0.707106781186544,0.,0.707106781186551));
#19100=DIRECTION('center_axis',(0.,1.,0.));
#19101=DIRECTION('ref_axis',(0.,0.,1.));
#19102=DIRECTION('center_axis',(0.,-1.,0.));
#19103=DIRECTION('ref_axis',(1.,0.,0.));
#19104=DIRECTION('center_axis',(0.,0.,1.));
#19105=DIRECTION('ref_axis',(1.,0.,0.));
#19106=DIRECTION('center_axis',(1.,0.,0.));
#19107=DIRECTION('ref_axis',(0.,1.,0.));
#19108=DIRECTION('center_axis',(0.,0.,1.));
#19109=DIRECTION('ref_axis',(0.707106781186548,0.707106781186548,0.));
#19110=DIRECTION('center_axis',(-1.,0.,0.));
#19111=DIRECTION('ref_axis',(0.,0.707106781186549,0.707106781186546));
#19112=DIRECTION('center_axis',(1.,0.,0.));
#19113=DIRECTION('ref_axis',(0.,1.,0.));
#19114=DIRECTION('',(-1.,0.,0.));
#19115=DIRECTION('center_axis',(0.,0.,1.));
#19116=DIRECTION('ref_axis',(1.,0.,0.));
#19117=DIRECTION('center_axis',(0.,1.,0.));
#19118=DIRECTION('ref_axis',(-1.,0.,0.));
#19119=DIRECTION('center_axis',(0.,0.,1.));
#19120=DIRECTION('ref_axis',(-0.707106781186548,0.707106781186548,0.));
#19121=DIRECTION('center_axis',(0.,-1.,0.));
#19122=DIRECTION('ref_axis',(-0.707106781186548,0.,0.707106781186548));
#19123=DIRECTION('center_axis',(0.,1.,0.));
#19124=DIRECTION('ref_axis',(-1.,0.,0.));
#19125=DIRECTION('',(0.,-1.,0.));
#19126=DIRECTION('center_axis',(0.,0.,1.));
#19127=DIRECTION('ref_axis',(1.,0.,0.));
#19128=DIRECTION('center_axis',(-1.,0.,0.));
#19129=DIRECTION('ref_axis',(0.,-1.,0.));
#19130=DIRECTION('center_axis',(0.,0.,1.));
#19131=DIRECTION('ref_axis',(-0.707106781186548,-0.707106781186548,0.));
#19132=DIRECTION('center_axis',(1.,0.,0.));
#19133=DIRECTION('ref_axis',(0.,-0.707106781186549,0.707106781186546));
#19134=DIRECTION('center_axis',(-1.,0.,0.));
#19135=DIRECTION('ref_axis',(0.,-1.,0.));
#19136=DIRECTION('',(1.,0.,0.));
#19137=DIRECTION('center_axis',(0.,0.,1.));
#19138=DIRECTION('ref_axis',(1.,0.,0.));
#19139=DIRECTION('center_axis',(0.,0.,1.));
#19140=DIRECTION('ref_axis',(0.707106781186548,-0.707106781186547,0.));
#19141=DIRECTION('center_axis',(0.,0.,1.));
#19142=DIRECTION('ref_axis',(0.,1.,0.));
#19143=DIRECTION('',(0.,0.,1.));
#19144=DIRECTION('center_axis',(0.,0.,-1.));
#19145=DIRECTION('ref_axis',(-0.309915766398542,0.950764017902237,0.));
#19146=DIRECTION('',(0.,0.,1.));
#19147=DIRECTION('center_axis',(0.,1.,0.));
#19148=DIRECTION('ref_axis',(-1.,0.,0.));
#19149=DIRECTION('',(0.,0.,1.));
#19150=DIRECTION('',(1.,0.,0.));
#19151=DIRECTION('center_axis',(0.,0.,1.));
#19152=DIRECTION('ref_axis',(1.,5.55111512312578E-16,0.));
#19153=DIRECTION('center_axis',(0.,0.,-1.));
#19154=DIRECTION('ref_axis',(0.707106781186548,0.707106781186548,0.));
#19155=DIRECTION('center_axis',(0.,1.,0.));
#19156=DIRECTION('ref_axis',(0.707106781186544,0.,-0.707106781186551));
#19157=DIRECTION('center_axis',(0.,-1.,0.));
#19158=DIRECTION('ref_axis',(0.,0.,-1.));
#19159=DIRECTION('',(0.,1.,0.));
#19160=DIRECTION('center_axis',(-1.,0.,0.));
#19161=DIRECTION('ref_axis',(0.,0.707106781186546,-0.707106781186549));
#19162=DIRECTION('center_axis',(-1.,0.,0.));
#19163=DIRECTION('ref_axis',(0.,1.,0.));
#19164=DIRECTION('',(-1.,0.,0.));
#19165=DIRECTION('center_axis',(1.,0.,0.));
#19166=DIRECTION('ref_axis',(0.,0.,-1.));
#19167=DIRECTION('center_axis',(0.,0.,1.));
#19168=DIRECTION('ref_axis',(1.,0.,0.));
#19169=DIRECTION('center_axis',(0.,0.,1.));
#19170=DIRECTION('ref_axis',(-0.309915766398542,0.950764017902237,0.));
#19171=DIRECTION('center_axis',(0.,0.,1.));
#19172=DIRECTION('ref_axis',(1.,0.,0.));
#19173=DIRECTION('center_axis',(0.,0.,1.));
#19174=DIRECTION('ref_axis',(0.707106781186548,0.707106781186548,0.));
#19175=DIRECTION('center_axis',(0.,0.,1.));
#19176=DIRECTION('ref_axis',(1.,0.,0.));
#19177=DIRECTION('center_axis',(0.,0.,-1.));
#19178=DIRECTION('ref_axis',(1.,5.55111512312577E-16,0.));
#19179=DIRECTION('',(1.,0.,0.));
#19180=DIRECTION('center_axis',(0.,0.,-1.));
#19181=DIRECTION('ref_axis',(0.,1.,0.));
#19182=DIRECTION('center_axis',(1.,0.,0.));
#19183=DIRECTION('ref_axis',(0.,0.,-1.));
#19184=DIRECTION('center_axis',(0.,-1.,-1.22464679914735E-16));
#19185=DIRECTION('ref_axis',(0.,-1.22464679914735E-16,1.));
#19186=DIRECTION('center_axis',(1.,0.,0.));
#19187=DIRECTION('ref_axis',(0.,1.,6.12323399573677E-17));
#19188=DIRECTION('center_axis',(1.,0.,0.));
#19189=DIRECTION('ref_axis',(0.,1.,6.12323399573677E-17));
#19190=DIRECTION('center_axis',(-1.,0.,0.));
#19191=DIRECTION('ref_axis',(0.,1.,0.));
#19192=DIRECTION('',(0.888217643155949,0.459422918873766,5.62630807053692E-17));
#19193=DIRECTION('center_axis',(1.,0.,0.));
#19194=DIRECTION('ref_axis',(0.,0.,-1.));
#19195=DIRECTION('center_axis',(0.,0.,-1.));
#19196=DIRECTION('ref_axis',(-0.816496580927725,0.577350269189627,0.));
#19197=DIRECTION('',(0.,0.,-1.));
#19198=DIRECTION('',(0.,0.,1.));
#19199=DIRECTION('center_axis',(0.,0.,1.));
#19200=DIRECTION('ref_axis',(-0.816496580927725,-0.577350269189627,0.));
#19201=DIRECTION('',(0.,0.,-1.));
#19202=DIRECTION('',(0.,0.,1.));
#19203=DIRECTION('center_axis',(1.,0.,0.));
#19204=DIRECTION('ref_axis',(0.,0.,-1.));
#19205=DIRECTION('center_axis',(1.,0.,0.));
#19206=DIRECTION('ref_axis',(0.,0.,-1.));
#19207=DIRECTION('center_axis',(1.,0.,0.));
#19208=DIRECTION('ref_axis',(0.,0.,-1.));
#19209=DIRECTION('center_axis',(0.,0.,1.));
#19210=DIRECTION('ref_axis',(1.,0.,0.));
#19211=DIRECTION('center_axis',(0.,0.,1.));
#19212=DIRECTION('ref_axis',(1.,0.,0.));
#19213=DIRECTION('',(0.,0.,1.));
#19214=DIRECTION('',(0.,0.,1.));
#19215=DIRECTION('center_axis',(0.,0.,1.));
#19216=DIRECTION('ref_axis',(1.,0.,0.));
#19217=DIRECTION('center_axis',(0.,0.,1.));
#19218=DIRECTION('ref_axis',(1.,0.,0.));
#19219=DIRECTION('center_axis',(0.,0.,1.));
#19220=DIRECTION('ref_axis',(-0.294281086116927,-0.955718913883074,0.));
#19221=DIRECTION('center_axis',(-1.,0.,0.));
#19222=DIRECTION('ref_axis',(0.,-1.,0.));
#19223=DIRECTION('center_axis',(0.,0.,-1.));
#19224=DIRECTION('ref_axis',(-0.294281086116927,-0.955718913883074,0.));
#19225=DIRECTION('center_axis',(1.,0.,0.));
#19226=DIRECTION('ref_axis',(0.,-0.707106781186549,0.707106781186546));
#19227=DIRECTION('',(-1.,0.,0.));
#19228=DIRECTION('',(1.,0.,0.));
#19229=DIRECTION('center_axis',(-1.,0.,0.));
#19230=DIRECTION('ref_axis',(0.,-1.,0.));
#19231=DIRECTION('',(-1.,0.,0.));
#19232=DIRECTION('center_axis',(0.,0.,1.));
#19233=DIRECTION('ref_axis',(1.,0.,0.));
#19234=DIRECTION('center_axis',(0.,-1.,0.));
#19235=DIRECTION('ref_axis',(1.,0.,0.));
#19236=DIRECTION('center_axis',(0.,0.,-1.));
#19237=DIRECTION('ref_axis',(0.707106781186548,-0.707106781186547,0.));
#19238=DIRECTION('center_axis',(0.,0.,1.));
#19239=DIRECTION('ref_axis',(0.707106781186548,-0.707106781186547,0.));
#19240=DIRECTION('center_axis',(0.,1.,0.));
#19241=DIRECTION('ref_axis',(0.707106781186548,0.,0.707106781186548));
#19242=DIRECTION('',(0.,-1.,0.));
#19243=DIRECTION('',(0.,1.,0.));
#19244=DIRECTION('center_axis',(0.,-1.,0.));
#19245=DIRECTION('ref_axis',(1.,0.,0.));
#19246=DIRECTION('',(0.,0.,1.));
#19247=DIRECTION('',(-1.,0.,0.));
#19248=DIRECTION('',(0.,0.,1.));
#19249=DIRECTION('center_axis',(0.,0.,1.));
#19250=DIRECTION('ref_axis',(-1.,0.,0.));
#19251=DIRECTION('',(0.,0.,1.));
#19252=DIRECTION('center_axis',(0.,0.,-1.));
#19253=DIRECTION('ref_axis',(-0.707106781186548,-0.707106781186548,0.));
#19254=DIRECTION('center_axis',(0.,0.,1.));
#19255=DIRECTION('ref_axis',(1.,0.,0.));
#19256=DIRECTION('center_axis',(0.,0.,1.));
#19257=DIRECTION('ref_axis',(0.,-1.,0.));
#19258=DIRECTION('center_axis',(0.,0.,1.));
#19259=DIRECTION('ref_axis',(-1.,0.,0.));
#19260=DIRECTION('center_axis',(0.,0.,-1.));
#19261=DIRECTION('ref_axis',(0.,-1.,0.));
#19262=DIRECTION('center_axis',(0.,0.,1.));
#19263=DIRECTION('ref_axis',(0.,-1.,0.));
#19264=DIRECTION('center_axis',(0.,0.,1.));
#19265=DIRECTION('ref_axis',(1.,0.,0.));
#19266=DIRECTION('center_axis',(0.,1.,0.));
#19267=DIRECTION('ref_axis',(1.,0.,0.));
#19268=DIRECTION('center_axis',(1.,0.,0.));
#19269=DIRECTION('ref_axis',(0.,0.,-1.));
#19270=DIRECTION('center_axis',(0.,0.,-1.));
#19271=DIRECTION('ref_axis',(0.707106781186548,0.707106781186548,0.));
#19272=DIRECTION('center_axis',(-1.,0.,0.));
#19273=DIRECTION('ref_axis',(0.,0.707106781186549,-0.707106781186546));
#19274=DIRECTION('center_axis',(1.,0.,0.));
#19275=DIRECTION('ref_axis',(0.,0.,-1.));
#19276=DIRECTION('',(1.,0.,0.));
#19277=DIRECTION('center_axis',(0.,0.,1.));
#19278=DIRECTION('ref_axis',(1.,0.,0.));
#19279=DIRECTION('center_axis',(0.,1.,0.));
#19280=DIRECTION('ref_axis',(0.,0.,-1.));
#19281=DIRECTION('center_axis',(0.,0.,-1.));
#19282=DIRECTION('ref_axis',(-0.707106781186548,0.707106781186548,0.));
#19283=DIRECTION('center_axis',(0.,-1.,0.));
#19284=DIRECTION('ref_axis',(-0.707106781186551,0.,-0.707106781186544));
#19285=DIRECTION('center_axis',(0.,1.,0.));
#19286=DIRECTION('ref_axis',(0.,0.,-1.));
#19287=DIRECTION('',(0.,1.,0.));
#19288=DIRECTION('center_axis',(0.,0.,1.));
#19289=DIRECTION('ref_axis',(1.,0.,0.));
#19290=DIRECTION('center_axis',(-1.,0.,0.));
#19291=DIRECTION('ref_axis',(0.,0.,-1.));
#19292=DIRECTION('center_axis',(1.,0.,0.));
#19293=DIRECTION('ref_axis',(0.,-0.707106781186549,-0.707106781186546));
#19294=DIRECTION('center_axis',(-1.,0.,0.));
#19295=DIRECTION('ref_axis',(0.,0.,-1.));
#19296=DIRECTION('center_axis',(0.,0.,1.));
#19297=DIRECTION('ref_axis',(1.,0.,0.));
#19298=DIRECTION('center_axis',(0.,-1.,0.));
#19299=DIRECTION('ref_axis',(0.,0.,-1.));
#19300=DIRECTION('center_axis',(0.,0.,-1.));
#19301=DIRECTION('ref_axis',(0.707106781186548,-0.707106781186547,0.));
#19302=DIRECTION('center_axis',(0.,1.,0.));
#19303=DIRECTION('ref_axis',(0.707106781186548,0.,-0.707106781186548));
#19304=DIRECTION('',(0.,-1.,0.));
#19305=DIRECTION('center_axis',(0.,0.,1.));
#19306=DIRECTION('ref_axis',(1.11022302462516E-15,-1.,0.));
#19307=DIRECTION('',(0.,0.,1.));
#19308=DIRECTION('center_axis',(1.,0.,0.));
#19309=DIRECTION('ref_axis',(0.,1.,0.));
#19310=DIRECTION('',(0.,0.,1.));
#19311=DIRECTION('',(0.,1.,0.));
#19312=DIRECTION('',(0.,0.,1.));
#19313=DIRECTION('',(0.,0.,1.));
#19314=DIRECTION('center_axis',(0.,0.,1.));
#19315=DIRECTION('ref_axis',(1.,5.55111512312578E-16,0.));
#19316=DIRECTION('',(0.,0.,1.));
#19317=DIRECTION('center_axis',(0.,0.,1.));
#19318=DIRECTION('ref_axis',(0.707106781186548,0.707106781186548,0.));
#19319=DIRECTION('center_axis',(0.,1.,0.));
#19320=DIRECTION('ref_axis',(0.707106781186548,0.,0.707106781186548));
#19321=DIRECTION('center_axis',(0.,-1.,0.));
#19322=DIRECTION('ref_axis',(1.,0.,0.));
#19323=DIRECTION('',(0.,-1.,0.));
#19324=DIRECTION('center_axis',(0.,0.,1.));
#19325=DIRECTION('ref_axis',(1.,0.,0.));
#19326=DIRECTION('center_axis',(1.,0.,0.));
#19327=DIRECTION('ref_axis',(0.,1.,0.));
#19328=DIRECTION('center_axis',(0.,0.,-1.));
#19329=DIRECTION('ref_axis',(0.707106781186548,0.707106781186548,0.));
#19330=DIRECTION('center_axis',(-1.,0.,0.));
#19331=DIRECTION('ref_axis',(0.,0.707106781186549,0.707106781186546));
#19332=DIRECTION('',(1.,0.,0.));
#19333=DIRECTION('',(-1.,0.,0.));
#19334=DIRECTION('center_axis',(1.,0.,0.));
#19335=DIRECTION('ref_axis',(0.,1.,0.));
#19336=DIRECTION('',(1.,0.,0.));
#19337=DIRECTION('center_axis',(0.,0.,1.));
#19338=DIRECTION('ref_axis',(1.,0.,0.));
#19339=DIRECTION('center_axis',(0.,0.,-1.));
#19340=DIRECTION('ref_axis',(-0.294281086116927,0.955718913883074,0.));
#19341=DIRECTION('center_axis',(0.,0.,1.));
#19342=DIRECTION('ref_axis',(-0.294281086116927,0.955718913883074,0.));
#19343=DIRECTION('center_axis',(0.,0.,1.));
#19344=DIRECTION('ref_axis',(1.,0.,0.));
#19345=DIRECTION('center_axis',(0.,0.,1.));
#19346=DIRECTION('ref_axis',(0.,1.,0.));
#19347=DIRECTION('center_axis',(0.,0.,1.));
#19348=DIRECTION('ref_axis',(0.,1.,0.));
#19349=DIRECTION('center_axis',(0.,0.,1.));
#19350=DIRECTION('ref_axis',(1.,0.,0.));
#19351=DIRECTION('center_axis',(0.,0.,1.));
#19352=DIRECTION('ref_axis',(0.,1.,0.));
#19353=DIRECTION('center_axis',(0.,0.,1.));
#19354=DIRECTION('ref_axis',(1.,5.55111512312577E-16,0.));
#19355=DIRECTION('center_axis',(0.,0.,-1.));
#19356=DIRECTION('ref_axis',(0.,1.,0.));
#19357=DIRECTION('center_axis',(0.,0.,1.));
#19358=DIRECTION('ref_axis',(0.,-1.,0.));
#19359=DIRECTION('center_axis',(0.,0.,-1.));
#19360=DIRECTION('ref_axis',(0.707106781186546,-0.707106781186549,0.));
#19361=DIRECTION('center_axis',(0.,1.77635683940025E-16,1.));
#19362=DIRECTION('ref_axis',(0.707106781186546,0.707106781186549,0.));
#19363=DIRECTION('center_axis',(0.,0.,1.));
#19364=DIRECTION('ref_axis',(0.707106781186546,0.707106781186549,0.));
#19365=DIRECTION('center_axis',(0.,-0.866025403784439,-0.5));
#19366=DIRECTION('ref_axis',(0.,0.5,-0.866025403784439));
#19367=DIRECTION('center_axis',(0.,0.866025403784439,0.5));
#19368=DIRECTION('ref_axis',(0.707106781186546,0.353553390593275,-0.612372435695796));
#19369=DIRECTION('center_axis',(0.,-0.866025403784439,-0.5));
#19370=DIRECTION('ref_axis',(0.707106781186547,-0.353553390593273,0.612372435695796));
#19371=DIRECTION('center_axis',(0.,-0.866025403784439,-0.5));
#19372=DIRECTION('ref_axis',(0.707106781186547,-0.353553390593273,0.612372435695796));
#19373=DIRECTION('center_axis',(0.,0.,-1.));
#19374=DIRECTION('ref_axis',(0.,1.,0.));
#19375=DIRECTION('center_axis',(0.,0.,1.));
#19376=DIRECTION('ref_axis',(0.707106781186546,0.707106781186549,0.));
#19377=DIRECTION('center_axis',(0.,-6.66133814775094E-17,-1.));
#19378=DIRECTION('ref_axis',(0.707106781186546,-0.707106781186549,0.));
#19379=DIRECTION('center_axis',(0.,0.,-1.));
#19380=DIRECTION('ref_axis',(0.707106781186546,-0.707106781186549,0.));
#19381=DIRECTION('center_axis',(0.,0.866025403784439,-0.5));
#19382=DIRECTION('ref_axis',(0.,0.5,0.866025403784439));
#19383=DIRECTION('center_axis',(0.,-0.866025403784439,0.5));
#19384=DIRECTION('ref_axis',(0.707106781186546,0.353553390593275,0.612372435695795));
#19385=DIRECTION('center_axis',(0.,0.866025403784439,-0.5));
#19386=DIRECTION('ref_axis',(0.707106781186546,-0.353553390593273,-0.612372435695797));
#19387=DIRECTION('center_axis',(0.,0.866025403784439,-0.5));
#19388=DIRECTION('ref_axis',(0.707106781186546,-0.353553390593273,-0.612372435695797));
#19389=DIRECTION('center_axis',(0.,0.866025403784439,0.5));
#19390=DIRECTION('ref_axis',(0.,-0.5,0.866025403784439));
#19391=DIRECTION('center_axis',(0.,-0.866025403784439,-0.5));
#19392=DIRECTION('ref_axis',(0.707106781186546,-0.353553390593275,0.612372435695795));
#19393=DIRECTION('center_axis',(0.,0.866025403784439,0.5));
#19394=DIRECTION('ref_axis',(0.707106781186547,0.353553390593273,-0.612372435695796));
#19395=DIRECTION('center_axis',(0.,0.866025403784439,0.499999999999999));
#19396=DIRECTION('ref_axis',(0.707106781186547,0.353553390593273,-0.612372435695796));
#19397=DIRECTION('center_axis',(0.,-0.866025403784438,0.5));
#19398=DIRECTION('ref_axis',(0.,-0.5,-0.866025403784438));
#19399=DIRECTION('center_axis',(0.,0.866025403784438,-0.5));
#19400=DIRECTION('ref_axis',(0.707106781186546,-0.353553390593275,-0.612372435695795));
#19401=DIRECTION('center_axis',(0.,-0.866025403784438,0.5));
#19402=DIRECTION('ref_axis',(0.707106781186546,0.353553390593276,0.612372435695795));
#19403=DIRECTION('center_axis',(0.,-0.866025403784438,0.500000000000001));
#19404=DIRECTION('ref_axis',(0.707106781186546,0.353553390593276,0.612372435695795));
#19405=DIRECTION('center_axis',(0.,0.866025403784438,-0.500000000000001));
#19406=DIRECTION('ref_axis',(0.,0.500000000000001,0.866025403784438));
#19407=DIRECTION('center_axis',(0.,-0.866025403784439,-0.499999999999999));
#19408=DIRECTION('ref_axis',(0.,0.499999999999999,-0.866025403784439));
#19409=DIRECTION('center_axis',(0.,-0.866025403784439,0.5));
#19410=DIRECTION('ref_axis',(0.,-0.5,-0.866025403784438));
#19411=DIRECTION('center_axis',(0.,0.,1.));
#19412=DIRECTION('ref_axis',(0.,-1.,0.));
#19413=DIRECTION('center_axis',(0.,0.866025403784439,0.5));
#19414=DIRECTION('ref_axis',(0.,-0.5,0.866025403784438));
#19415=DIRECTION('center_axis',(0.,0.,-1.));
#19416=DIRECTION('ref_axis',(0.,1.,0.));
#19417=DIRECTION('center_axis',(0.,0.,1.));
#19418=DIRECTION('ref_axis',(1.,0.,0.));
#19419=DIRECTION('center_axis',(0.,0.,1.));
#19420=DIRECTION('ref_axis',(1.,0.,0.));
#19421=DIRECTION('center_axis',(0.,0.,1.));
#19422=DIRECTION('ref_axis',(1.,0.,0.));
#19423=DIRECTION('center_axis',(0.,0.,1.));
#19424=DIRECTION('ref_axis',(1.,0.,0.));
#19425=DIRECTION('center_axis',(0.,0.,1.));
#19426=DIRECTION('ref_axis',(1.,0.,0.));
#19427=DIRECTION('center_axis',(0.,0.,1.));
#19428=DIRECTION('ref_axis',(2.22044604925031E-15,-1.,0.));
#19429=DIRECTION('center_axis',(1.,0.,0.));
#19430=DIRECTION('ref_axis',(0.,0.,-1.));
#19431=DIRECTION('',(1.,0.,0.));
#19432=DIRECTION('center_axis',(1.,0.,0.));
#19433=DIRECTION('ref_axis',(0.,0.,-1.));
#19434=DIRECTION('',(1.,0.,0.));
#19435=DIRECTION('center_axis',(1.,0.,0.));
#19436=DIRECTION('ref_axis',(0.,0.,-1.));
#19437=DIRECTION('',(1.,0.,0.));
#19438=DIRECTION('center_axis',(1.,0.,0.));
#19439=DIRECTION('ref_axis',(0.,0.,-1.));
#19440=DIRECTION('',(1.,0.,0.));
#19441=DIRECTION('center_axis',(1.,0.,0.));
#19442=DIRECTION('ref_axis',(0.,0.,-1.));
#19443=DIRECTION('',(1.,0.,0.));
#19444=DIRECTION('center_axis',(1.,0.,0.));
#19445=DIRECTION('ref_axis',(0.,0.,-1.));
#19446=DIRECTION('',(1.,0.,0.));
#19447=DIRECTION('center_axis',(0.,0.,1.));
#19448=DIRECTION('ref_axis',(1.,0.,0.));
#19449=DIRECTION('',(0.,0.,1.));
#19450=DIRECTION('center_axis',(0.,0.,1.));
#19451=DIRECTION('ref_axis',(1.,0.,0.));
#19452=DIRECTION('center_axis',(0.,0.,1.));
#19453=DIRECTION('ref_axis',(1.,0.,0.));
#19454=DIRECTION('center_axis',(0.,0.,1.));
#19455=DIRECTION('ref_axis',(1.,0.,0.));
#19456=DIRECTION('center_axis',(0.,0.,1.));
#19457=DIRECTION('ref_axis',(1.,0.,0.));
#19458=DIRECTION('',(0.,0.,1.));
#19459=DIRECTION('center_axis',(0.,0.,1.));
#19460=DIRECTION('ref_axis',(1.,0.,0.));
#19461=DIRECTION('center_axis',(0.,0.,1.));
#19462=DIRECTION('ref_axis',(1.,0.,0.));
#19463=DIRECTION('center_axis',(0.,0.,-1.));
#19464=DIRECTION('ref_axis',(-1.,0.,0.));
#19465=DIRECTION('center_axis',(0.,0.,1.));
#19466=DIRECTION('ref_axis',(1.,0.,0.));
#19467=DIRECTION('center_axis',(0.,0.,1.));
#19468=DIRECTION('ref_axis',(1.,0.,0.));
#19469=DIRECTION('',(0.,0.,1.));
#19470=DIRECTION('center_axis',(-1.,0.,0.));
#19471=DIRECTION('ref_axis',(0.,1.,0.));
#19472=DIRECTION('',(0.707106781186548,0.707106781186548,8.65956056235493E-17));
#19473=DIRECTION('center_axis',(1.,0.,0.));
#19474=DIRECTION('ref_axis',(0.,0.,-1.));
#19475=DIRECTION('center_axis',(1.,0.,0.));
#19476=DIRECTION('ref_axis',(0.,0.,-1.));
#19477=DIRECTION('center_axis',(0.,0.,1.));
#19478=DIRECTION('ref_axis',(1.11022302462516E-15,-1.,0.));
#19479=DIRECTION('',(0.,0.,1.));
#19480=DIRECTION('center_axis',(0.,-1.,0.));
#19481=DIRECTION('ref_axis',(1.,0.,0.));
#19482=DIRECTION('',(0.,0.,1.));
#19483=DIRECTION('center_axis',(0.,0.,1.));
#19484=DIRECTION('ref_axis',(-1.,0.,0.));
#19485=DIRECTION('',(0.,0.,1.));
#19486=DIRECTION('center_axis',(0.,0.,1.));
#19487=DIRECTION('ref_axis',(0.,1.,0.));
#19488=DIRECTION('',(0.,0.,1.));
#19489=DIRECTION('',(0.,0.,1.));
#19490=DIRECTION('center_axis',(0.,1.,0.));
#19491=DIRECTION('ref_axis',(-1.,0.,0.));
#19492=DIRECTION('center_axis',(0.,0.,1.));
#19493=DIRECTION('ref_axis',(0.,1.,0.));
#19494=DIRECTION('center_axis',(-1.,0.,0.));
#19495=DIRECTION('ref_axis',(0.,-1.,0.));
#19496=DIRECTION('center_axis',(-1.,0.,0.));
#19497=DIRECTION('ref_axis',(0.,-1.,0.));
#19498=DIRECTION('center_axis',(0.,0.,1.));
#19499=DIRECTION('ref_axis',(-1.,0.,0.));
#19500=DIRECTION('center_axis',(0.,0.,1.));
#19501=DIRECTION('ref_axis',(-1.,0.,0.));
#19502=DIRECTION('',(0.,0.,1.));
#19503=DIRECTION('center_axis',(0.,0.,1.));
#19504=DIRECTION('ref_axis',(1.,5.55111512312577E-16,0.));
#19505=DIRECTION('center_axis',(0.,0.,1.));
#19506=DIRECTION('ref_axis',(2.22044604925031E-15,-1.,0.));
#19507=DIRECTION('center_axis',(0.,-1.,0.));
#19508=DIRECTION('ref_axis',(1.,0.,0.));
#19509=DIRECTION('',(0.,0.,1.));
#19510=DIRECTION('center_axis',(0.,0.,1.));
#19511=DIRECTION('ref_axis',(0.,1.,0.));
#19512=DIRECTION('',(0.,0.,1.));
#19513=DIRECTION('center_axis',(0.,1.,0.));
#19514=DIRECTION('ref_axis',(-1.,0.,0.));
#19515=DIRECTION('',(0.,0.,1.));
#19516=DIRECTION('center_axis',(0.,0.,1.));
#19517=DIRECTION('ref_axis',(1.,5.55111512312577E-16,0.));
#19518=DIRECTION('center_axis',(0.,0.,1.));
#19519=DIRECTION('ref_axis',(2.22044604925031E-15,-1.,0.));
#19520=DIRECTION('axis',(0.,0.,1.));
#19521=DIRECTION('refdir',(1.,0.,0.));
#19522=DIRECTION('center_axis',(0.,1.,0.));
#19523=DIRECTION('ref_axis',(1.,0.,0.));
#19524=DIRECTION('center_axis',(0.,-1.,0.));
#19525=DIRECTION('ref_axis',(1.,0.,0.));
#19526=DIRECTION('',(0.923879532511287,-0.38268343236509,-1.1314261122877E-16));
#19527=DIRECTION('center_axis',(0.,1.,0.));
#19528=DIRECTION('ref_axis',(1.,0.,0.));
#19529=DIRECTION('center_axis',(0.,1.,0.));
#19530=DIRECTION('ref_axis',(1.,0.,0.));
#19531=DIRECTION('',(-0.707106781186548,0.707106781186547,-8.65956056235494E-17));
#19532=DIRECTION('center_axis',(0.,1.,0.));
#19533=DIRECTION('ref_axis',(1.,0.,0.));
#19534=DIRECTION('center_axis',(0.,1.,0.));
#19535=DIRECTION('ref_axis',(1.,0.,0.));
#19536=DIRECTION('center_axis',(0.,1.,0.));
#19537=DIRECTION('ref_axis',(1.,0.,0.));
#19538=DIRECTION('center_axis',(0.,1.,0.));
#19539=DIRECTION('ref_axis',(1.,0.,0.));
#19540=DIRECTION('',(-0.382683432365092,0.923879532511286,-4.68652040532633E-17));
#19541=DIRECTION('center_axis',(0.,-1.,0.));
#19542=DIRECTION('ref_axis',(1.,0.,0.));
#19543=DIRECTION('center_axis',(0.,-1.,0.));
#19544=DIRECTION('ref_axis',(1.,0.,0.));
#19545=DIRECTION('',(0.,1.,0.));
#19546=DIRECTION('center_axis',(-1.,0.,0.));
#19547=DIRECTION('ref_axis',(0.,-1.,0.));
#19548=DIRECTION('center_axis',(-1.,0.,0.));
#19549=DIRECTION('ref_axis',(0.,-1.,0.));
#19550=DIRECTION('',(-0.70710678118655,0.707106781186545,8.6595605623549E-17));
#19551=DIRECTION('center_axis',(1.,0.,0.));
#19552=DIRECTION('ref_axis',(0.,-1.,0.));
#19553=DIRECTION('center_axis',(1.,0.,0.));
#19554=DIRECTION('ref_axis',(0.,-1.,0.));
#19555=DIRECTION('center_axis',(1.,0.,0.));
#19556=DIRECTION('ref_axis',(0.,1.,0.));
#19557=DIRECTION('',(-1.,0.,0.));
#19558=DIRECTION('center_axis',(1.,0.,0.));
#19559=DIRECTION('ref_axis',(0.,0.,-1.));
#19560=DIRECTION('center_axis',(1.,0.,0.));
#19561=DIRECTION('ref_axis',(0.,0.,-1.));
#19562=DIRECTION('center_axis',(-1.,0.,0.));
#19563=DIRECTION('ref_axis',(0.,0.,-1.));
#19564=DIRECTION('center_axis',(-1.,0.,0.));
#19565=DIRECTION('ref_axis',(0.,0.,-1.));
#19566=DIRECTION('center_axis',(-1.,0.,0.));
#19567=DIRECTION('ref_axis',(0.,0.,-1.));
#19568=DIRECTION('center_axis',(-1.,0.,0.));
#19569=DIRECTION('ref_axis',(0.,0.,-1.));
#19570=DIRECTION('center_axis',(-1.,0.,0.));
#19571=DIRECTION('ref_axis',(0.,0.,-1.));
#19572=DIRECTION('center_axis',(-1.,0.,0.));
#19573=DIRECTION('ref_axis',(0.,0.,-1.));
#19574=DIRECTION('center_axis',(1.,0.,0.));
#19575=DIRECTION('ref_axis',(0.,0.,-1.));
#19576=DIRECTION('center_axis',(0.,1.,0.));
#19577=DIRECTION('ref_axis',(1.,0.,0.));
#19578=DIRECTION('',(0.,1.,0.));
#19579=DIRECTION('center_axis',(0.,1.,0.));
#19580=DIRECTION('ref_axis',(1.,0.,0.));
#19581=DIRECTION('center_axis',(0.,1.,0.));
#19582=DIRECTION('ref_axis',(1.,0.,0.));
#19583=DIRECTION('center_axis',(-1.,0.,0.));
#19584=DIRECTION('ref_axis',(0.,0.,-1.));
#19585=DIRECTION('',(-1.,0.,0.));
#19586=DIRECTION('center_axis',(1.,0.,0.));
#19587=DIRECTION('ref_axis',(0.,0.,-1.));
#19588=DIRECTION('center_axis',(-1.,0.,0.));
#19589=DIRECTION('ref_axis',(0.,0.,-1.));
#19590=DIRECTION('',(-1.,0.,0.));
#19591=DIRECTION('center_axis',(1.,0.,0.));
#19592=DIRECTION('ref_axis',(0.,0.,-1.));
#19593=DIRECTION('center_axis',(-1.,0.,0.));
#19594=DIRECTION('ref_axis',(0.,0.,-1.));
#19595=DIRECTION('',(-1.,0.,0.));
#19596=DIRECTION('center_axis',(1.,0.,0.));
#19597=DIRECTION('ref_axis',(0.,0.,-1.));
#19598=DIRECTION('center_axis',(-1.,0.,0.));
#19599=DIRECTION('ref_axis',(0.,0.,-1.));
#19600=DIRECTION('',(-1.,0.,0.));
#19601=DIRECTION('center_axis',(1.,0.,0.));
#19602=DIRECTION('ref_axis',(0.,0.,-1.));
#19603=DIRECTION('center_axis',(-1.,0.,0.));
#19604=DIRECTION('ref_axis',(0.,0.,-1.));
#19605=DIRECTION('',(-1.,0.,0.));
#19606=DIRECTION('center_axis',(1.,0.,0.));
#19607=DIRECTION('ref_axis',(0.,0.,-1.));
#19608=DIRECTION('center_axis',(-1.,0.,0.));
#19609=DIRECTION('ref_axis',(0.,0.,-1.));
#19610=DIRECTION('',(-1.,0.,0.));
#19611=DIRECTION('center_axis',(1.,0.,0.));
#19612=DIRECTION('ref_axis',(0.,0.,-1.));
#19613=DIRECTION('center_axis',(-1.,0.,0.));
#19614=DIRECTION('ref_axis',(0.,0.,1.));
#19615=DIRECTION('center_axis',(1.,0.,0.));
#19616=DIRECTION('ref_axis',(0.,0.,-1.));
#19617=DIRECTION('center_axis',(1.,0.,0.));
#19618=DIRECTION('ref_axis',(0.,0.,-1.));
#19619=DIRECTION('center_axis',(-1.,0.,0.));
#19620=DIRECTION('ref_axis',(0.,1.,0.));
#19621=DIRECTION('',(-0.514495755427527,-0.857492925712544,-1.05012596676537E-16));
#19622=DIRECTION('center_axis',(1.,0.,0.));
#19623=DIRECTION('ref_axis',(0.,0.,-1.));
#19624=DIRECTION('center_axis',(-1.,0.,0.));
#19625=DIRECTION('ref_axis',(0.,1.,0.));
#19626=DIRECTION('',(-0.884918222381982,-0.465746432832622,-5.70374878182769E-17));
#19627=DIRECTION('center_axis',(1.,0.,0.));
#19628=DIRECTION('ref_axis',(0.,0.,-1.));
#19629=DIRECTION('center_axis',(-1.,0.,0.));
#19630=DIRECTION('ref_axis',(0.,0.,1.));
#19631=DIRECTION('center_axis',(1.,0.,0.));
#19632=DIRECTION('ref_axis',(0.,0.,-1.));
#19633=DIRECTION('center_axis',(1.,0.,0.));
#19634=DIRECTION('ref_axis',(0.,1.,0.));
#19635=DIRECTION('',(-0.707106781186547,0.707106781186547,8.65956056235493E-17));
#19636=DIRECTION('center_axis',(1.,0.,0.));
#19637=DIRECTION('ref_axis',(0.,1.,0.));
#19638=DIRECTION('',(-1.,0.,0.));
#19639=DIRECTION('axis',(0.,0.,1.));
#19640=DIRECTION('refdir',(1.,0.,0.));
#19641=DIRECTION('center_axis',(0.,-1.,0.));
#19642=DIRECTION('ref_axis',(1.,3.43542106681276E-16,0.));
#19643=DIRECTION('center_axis',(-6.65125149629304E-16,1.,0.));
#19644=DIRECTION('ref_axis',(1.,6.65125149629305E-16,0.));
#19645=DIRECTION('',(0.923879532511289,0.382683432365085,1.1314261122877E-16));
#19646=DIRECTION('center_axis',(0.,-1.,0.));
#19647=DIRECTION('ref_axis',(1.,0.,0.));
#19648=DIRECTION('center_axis',(0.,-1.,0.));
#19649=DIRECTION('ref_axis',(1.,0.,0.));
#19650=DIRECTION('',(-0.707106781186549,-0.707106781186546,8.65956056235495E-17));
#19651=DIRECTION('center_axis',(0.,-1.,0.));
#19652=DIRECTION('ref_axis',(1.,0.,0.));
#19653=DIRECTION('center_axis',(0.,1.,0.));
#19654=DIRECTION('ref_axis',(1.,0.,0.));
#19655=DIRECTION('center_axis',(0.,-1.,0.));
#19656=DIRECTION('ref_axis',(1.,0.,0.));
#19657=DIRECTION('center_axis',(0.,-1.,0.));
#19658=DIRECTION('ref_axis',(1.,0.,0.));
#19659=DIRECTION('',(-0.38268343236509,-0.923879532511287,4.6865204053263E-17));
#19660=DIRECTION('center_axis',(0.,1.,0.));
#19661=DIRECTION('ref_axis',(1.,0.,0.));
#19662=DIRECTION('center_axis',(0.,1.,0.));
#19663=DIRECTION('ref_axis',(1.,0.,0.));
#19664=DIRECTION('center_axis',(1.,0.,0.));
#19665=DIRECTION('ref_axis',(0.,-1.,0.));
#19666=DIRECTION('center_axis',(-1.,0.,0.));
#19667=DIRECTION('ref_axis',(0.,-1.,0.));
#19668=DIRECTION('center_axis',(-1.,0.,0.));
#19669=DIRECTION('ref_axis',(0.,-1.,0.));
#19670=DIRECTION('',(-0.70710678118655,-0.707106781186545,-8.6595605623549E-17));
#19671=DIRECTION('center_axis',(1.,0.,0.));
#19672=DIRECTION('ref_axis',(0.,-1.,0.));
#19673=DIRECTION('center_axis',(-1.,0.,0.));
#19674=DIRECTION('ref_axis',(0.,0.,1.));
#19675=DIRECTION('center_axis',(1.,0.,0.));
#19676=DIRECTION('ref_axis',(0.,0.,-1.));
#19677=DIRECTION('center_axis',(1.,0.,0.));
#19678=DIRECTION('ref_axis',(0.,0.,-1.));
#19679=DIRECTION('center_axis',(1.,0.,0.));
#19680=DIRECTION('ref_axis',(0.,0.,-1.));
#19681=DIRECTION('center_axis',(1.,0.,0.));
#19682=DIRECTION('ref_axis',(0.,0.,-1.));
#19683=DIRECTION('center_axis',(1.,0.,0.));
#19684=DIRECTION('ref_axis',(0.,0.,-1.));
#19685=DIRECTION('center_axis',(1.,0.,0.));
#19686=DIRECTION('ref_axis',(0.,0.,-1.));
#19687=DIRECTION('center_axis',(1.,0.,0.));
#19688=DIRECTION('ref_axis',(0.,0.,-1.));
#19689=DIRECTION('center_axis',(1.,0.,0.));
#19690=DIRECTION('ref_axis',(0.,1.,0.));
#19691=DIRECTION('center_axis',(1.,0.,0.));
#19692=DIRECTION('ref_axis',(0.,0.,-1.));
#19693=DIRECTION('',(-1.,0.,0.));
#19694=DIRECTION('center_axis',(0.,1.,0.));
#19695=DIRECTION('ref_axis',(9.49410759657493E-16,0.,-1.));
#19696=DIRECTION('center_axis',(0.,-1.,0.));
#19697=DIRECTION('ref_axis',(1.,0.,0.));
#19698=DIRECTION('',(0.,-1.,0.));
#19699=DIRECTION('center_axis',(0.,-1.,0.));
#19700=DIRECTION('ref_axis',(1.,0.,0.));
#19701=DIRECTION('center_axis',(0.,1.,0.));
#19702=DIRECTION('ref_axis',(1.,0.,0.));
#19703=DIRECTION('center_axis',(1.,0.,0.));
#19704=DIRECTION('ref_axis',(0.,0.,-1.));
#19705=DIRECTION('',(1.,0.,0.));
#19706=DIRECTION('center_axis',(-1.,0.,0.));
#19707=DIRECTION('ref_axis',(0.,0.,-1.));
#19708=DIRECTION('center_axis',(1.,0.,0.));
#19709=DIRECTION('ref_axis',(0.,0.,-1.));
#19710=DIRECTION('',(1.,0.,0.));
#19711=DIRECTION('center_axis',(-1.,0.,0.));
#19712=DIRECTION('ref_axis',(0.,0.,-1.));
#19713=DIRECTION('center_axis',(1.,0.,0.));
#19714=DIRECTION('ref_axis',(0.,0.,-1.));
#19715=DIRECTION('',(1.,0.,0.));
#19716=DIRECTION('center_axis',(-1.,0.,0.));
#19717=DIRECTION('ref_axis',(0.,0.,-1.));
#19718=DIRECTION('center_axis',(1.,0.,0.));
#19719=DIRECTION('ref_axis',(0.,0.,-1.));
#19720=DIRECTION('',(1.,0.,0.));
#19721=DIRECTION('center_axis',(-1.,0.,0.));
#19722=DIRECTION('ref_axis',(0.,0.,-1.));
#19723=DIRECTION('center_axis',(1.,0.,0.));
#19724=DIRECTION('ref_axis',(0.,0.,-1.));
#19725=DIRECTION('',(1.,0.,0.));
#19726=DIRECTION('center_axis',(-1.,0.,0.));
#19727=DIRECTION('ref_axis',(0.,0.,-1.));
#19728=DIRECTION('center_axis',(1.,0.,0.));
#19729=DIRECTION('ref_axis',(0.,0.,-1.));
#19730=DIRECTION('',(1.,0.,0.));
#19731=DIRECTION('center_axis',(-1.,0.,0.));
#19732=DIRECTION('ref_axis',(0.,0.,-1.));
#19733=DIRECTION('center_axis',(1.,0.,0.));
#19734=DIRECTION('ref_axis',(0.,1.,0.));
#19735=DIRECTION('center_axis',(1.,0.,0.));
#19736=DIRECTION('ref_axis',(0.,0.,-1.));
#19737=DIRECTION('',(-1.,0.,0.));
#19738=DIRECTION('center_axis',(-1.,0.,0.));
#19739=DIRECTION('ref_axis',(0.,1.,0.));
#19740=DIRECTION('center_axis',(1.,0.,0.));
#19741=DIRECTION('ref_axis',(0.,0.,-1.));
#19742=DIRECTION('',(-0.707106781186547,-0.707106781186547,-8.65956056235493E-17));
#19743=DIRECTION('center_axis',(1.,0.,0.));
#19744=DIRECTION('ref_axis',(0.,0.,-1.));
#19745=DIRECTION('center_axis',(1.,0.,0.));
#19746=DIRECTION('ref_axis',(0.,0.,-1.));
#19747=DIRECTION('center_axis',(1.,0.,0.));
#19748=DIRECTION('ref_axis',(0.,1.,0.));
#19749=DIRECTION('',(-0.884918222381982,0.465746432832622,5.70374878182769E-17));
#19750=DIRECTION('center_axis',(1.,0.,0.));
#19751=DIRECTION('ref_axis',(0.,0.,-1.));
#19752=DIRECTION('center_axis',(1.,0.,0.));
#19753=DIRECTION('ref_axis',(0.,1.,0.));
#19754=DIRECTION('',(-0.514495755427527,0.857492925712544,1.05012596676537E-16));
#19755=DIRECTION('center_axis',(1.,0.,0.));
#19756=DIRECTION('ref_axis',(0.,0.,-1.));
#19757=DIRECTION('center_axis',(1.,0.,0.));
#19758=DIRECTION('ref_axis',(0.,0.,-1.));
#19759=DIRECTION('axis',(0.,0.,1.));
#19760=DIRECTION('refdir',(1.,0.,0.));
#19761=DIRECTION('center_axis',(1.,0.,0.));
#19762=DIRECTION('ref_axis',(0.,0.,-1.));
#19763=DIRECTION('center_axis',(1.,0.,0.));
#19764=DIRECTION('ref_axis',(0.,0.,-1.));
#19765=DIRECTION('',(1.,0.,0.));
#19766=DIRECTION('center_axis',(-1.,0.,0.));
#19767=DIRECTION('ref_axis',(0.,0.,-1.));
#19768=DIRECTION('center_axis',(1.,0.,0.));
#19769=DIRECTION('ref_axis',(0.,0.,-1.));
#19770=DIRECTION('center_axis',(1.,0.,0.));
#19771=DIRECTION('ref_axis',(0.,0.,-1.));
#19772=DIRECTION('',(1.,0.,0.));
#19773=DIRECTION('center_axis',(-1.,0.,0.));
#19774=DIRECTION('ref_axis',(0.,0.,-1.));
#19775=DIRECTION('center_axis',(1.,0.,0.));
#19776=DIRECTION('ref_axis',(0.,0.,-1.));
#19777=DIRECTION('center_axis',(1.,0.,0.));
#19778=DIRECTION('ref_axis',(0.,0.,-1.));
#19779=DIRECTION('',(1.,0.,0.));
#19780=DIRECTION('center_axis',(-1.,0.,0.));
#19781=DIRECTION('ref_axis',(0.,0.,-1.));
#19782=DIRECTION('center_axis',(1.,0.,0.));
#19783=DIRECTION('ref_axis',(0.,0.,-1.));
#19784=DIRECTION('center_axis',(1.,0.,0.));
#19785=DIRECTION('ref_axis',(0.,0.,-1.));
#19786=DIRECTION('',(1.,0.,0.));
#19787=DIRECTION('center_axis',(-1.,0.,0.));
#19788=DIRECTION('ref_axis',(0.,0.,-1.));
#19789=DIRECTION('center_axis',(1.,0.,0.));
#19790=DIRECTION('ref_axis',(0.,0.,-1.));
#19791=DIRECTION('center_axis',(1.,0.,0.));
#19792=DIRECTION('ref_axis',(0.,0.,-1.));
#19793=DIRECTION('',(1.,0.,0.));
#19794=DIRECTION('center_axis',(-1.,0.,0.));
#19795=DIRECTION('ref_axis',(0.,0.,-1.));
#19796=DIRECTION('center_axis',(1.,0.,0.));
#19797=DIRECTION('ref_axis',(0.,0.,-1.));
#19798=DIRECTION('center_axis',(1.,0.,0.));
#19799=DIRECTION('ref_axis',(0.,0.,-1.));
#19800=DIRECTION('',(1.,0.,0.));
#19801=DIRECTION('center_axis',(-1.,0.,0.));
#19802=DIRECTION('ref_axis',(0.,0.,-1.));
#19803=DIRECTION('center_axis',(1.,0.,0.));
#19804=DIRECTION('ref_axis',(0.,1.,0.));
#19805=DIRECTION('center_axis',(1.,0.,0.));
#19806=DIRECTION('ref_axis',(0.,0.,-1.));
#19807=DIRECTION('',(-1.,0.,0.));
#19808=DIRECTION('center_axis',(1.,0.,0.));
#19809=DIRECTION('ref_axis',(0.,0.,-1.));
#19810=DIRECTION('center_axis',(-1.,0.,0.));
#19811=DIRECTION('ref_axis',(0.,0.,1.));
#19812=DIRECTION('center_axis',(1.,0.,0.));
#19813=DIRECTION('ref_axis',(0.,0.,-1.));
#19814=DIRECTION('center_axis',(1.,0.,0.));
#19815=DIRECTION('ref_axis',(0.,1.,0.));
#19816=DIRECTION('center_axis',(1.,0.,0.));
#19817=DIRECTION('ref_axis',(0.,0.,-1.));
#19818=DIRECTION('',(-1.,0.,0.));
#19819=DIRECTION('center_axis',(1.,0.,0.));
#19820=DIRECTION('ref_axis',(0.,0.,-1.));
#19821=DIRECTION('axis',(0.,0.,1.));
#19822=DIRECTION('refdir',(1.,0.,0.));
#19823=DIRECTION('center_axis',(1.,0.,0.));
#19824=DIRECTION('ref_axis',(0.,0.,-1.));
#19825=DIRECTION('center_axis',(1.,0.,0.));
#19826=DIRECTION('ref_axis',(0.,0.,-1.));
#19827=DIRECTION('',(1.,0.,0.));
#19828=DIRECTION('center_axis',(-1.,0.,0.));
#19829=DIRECTION('ref_axis',(0.,0.,-1.));
#19830=DIRECTION('center_axis',(1.,0.,0.));
#19831=DIRECTION('ref_axis',(0.,0.,-1.));
#19832=DIRECTION('center_axis',(1.,0.,0.));
#19833=DIRECTION('ref_axis',(0.,0.,-1.));
#19834=DIRECTION('',(1.,0.,0.));
#19835=DIRECTION('center_axis',(-1.,0.,0.));
#19836=DIRECTION('ref_axis',(0.,0.,-1.));
#19837=DIRECTION('center_axis',(1.,0.,0.));
#19838=DIRECTION('ref_axis',(0.,0.,-1.));
#19839=DIRECTION('center_axis',(1.,0.,0.));
#19840=DIRECTION('ref_axis',(0.,0.,-1.));
#19841=DIRECTION('',(1.,0.,0.));
#19842=DIRECTION('center_axis',(-1.,0.,0.));
#19843=DIRECTION('ref_axis',(0.,0.,-1.));
#19844=DIRECTION('center_axis',(1.,0.,0.));
#19845=DIRECTION('ref_axis',(0.,0.,-1.));
#19846=DIRECTION('center_axis',(1.,0.,0.));
#19847=DIRECTION('ref_axis',(0.,0.,-1.));
#19848=DIRECTION('',(1.,0.,0.));
#19849=DIRECTION('center_axis',(-1.,0.,0.));
#19850=DIRECTION('ref_axis',(0.,0.,-1.));
#19851=DIRECTION('center_axis',(1.,0.,0.));
#19852=DIRECTION('ref_axis',(0.,0.,-1.));
#19853=DIRECTION('center_axis',(1.,0.,0.));
#19854=DIRECTION('ref_axis',(0.,0.,-1.));
#19855=DIRECTION('',(1.,0.,0.));
#19856=DIRECTION('center_axis',(-1.,0.,0.));
#19857=DIRECTION('ref_axis',(0.,0.,-1.));
#19858=DIRECTION('center_axis',(1.,0.,0.));
#19859=DIRECTION('ref_axis',(0.,0.,-1.));
#19860=DIRECTION('center_axis',(1.,0.,0.));
#19861=DIRECTION('ref_axis',(0.,0.,-1.));
#19862=DIRECTION('',(1.,0.,0.));
#19863=DIRECTION('center_axis',(-1.,0.,0.));
#19864=DIRECTION('ref_axis',(0.,0.,-1.));
#19865=DIRECTION('center_axis',(1.,0.,0.));
#19866=DIRECTION('ref_axis',(0.,1.,0.));
#19867=DIRECTION('center_axis',(1.,0.,0.));
#19868=DIRECTION('ref_axis',(0.,0.,-1.));
#19869=DIRECTION('',(-1.,0.,0.));
#19870=DIRECTION('center_axis',(1.,0.,0.));
#19871=DIRECTION('ref_axis',(0.,0.,-1.));
#19872=DIRECTION('center_axis',(-1.,0.,0.));
#19873=DIRECTION('ref_axis',(0.,0.,1.));
#19874=DIRECTION('center_axis',(1.,0.,0.));
#19875=DIRECTION('ref_axis',(0.,0.,-1.));
#19876=DIRECTION('center_axis',(-1.,0.,0.));
#19877=DIRECTION('ref_axis',(0.,1.,0.));
#19878=DIRECTION('',(-0.124034734589211,-0.992277876713667,-1.21518992558212E-16));
#19879=DIRECTION('center_axis',(1.,0.,0.));
#19880=DIRECTION('ref_axis',(0.,0.,-1.));
#19881=DIRECTION('center_axis',(-1.,0.,0.));
#19882=DIRECTION('ref_axis',(0.,0.,1.));
#19883=DIRECTION('center_axis',(1.,0.,0.));
#19884=DIRECTION('ref_axis',(0.,0.,-1.));
#19885=DIRECTION('center_axis',(1.,0.,0.));
#19886=DIRECTION('ref_axis',(0.,1.,0.));
#19887=DIRECTION('center_axis',(1.,0.,0.));
#19888=DIRECTION('ref_axis',(0.,0.,-1.));
#19889=DIRECTION('',(-1.,0.,0.));
#19890=DIRECTION('center_axis',(1.,0.,0.));
#19891=DIRECTION('ref_axis',(0.,0.,-1.));
#19892=DIRECTION('center_axis',(1.,0.,0.));
#19893=DIRECTION('ref_axis',(0.,0.,-1.));
#19894=DIRECTION('center_axis',(1.,0.,0.));
#19895=DIRECTION('ref_axis',(0.,1.,0.));
#19896=DIRECTION('',(-0.124034734589208,0.992277876713668,1.21518992558212E-16));
#19897=DIRECTION('center_axis',(1.,0.,0.));
#19898=DIRECTION('ref_axis',(0.,0.,-1.));
#19899=DIRECTION('center_axis',(1.,0.,0.));
#19900=DIRECTION('ref_axis',(0.,0.,-1.));
#19901=DIRECTION('axis',(0.,0.,1.));
#19902=DIRECTION('refdir',(1.,0.,0.));
#19903=DIRECTION('center_axis',(1.,0.,-1.09798087011876E-14));
#19904=DIRECTION('ref_axis',(0.,-1.,-3.08236690249437E-17));
#19905=DIRECTION('center_axis',(-1.,0.,0.));
#19906=DIRECTION('ref_axis',(0.,-1.,-6.12323399573677E-17));
#19907=DIRECTION('center_axis',(-1.,0.,0.));
#19908=DIRECTION('ref_axis',(0.,-1.,-6.12323399573677E-17));
#19909=DIRECTION('',(-0.382683432365084,-0.923879532511289,4.06017091232465E-15));
#19910=DIRECTION('center_axis',(1.,0.,0.));
#19911=DIRECTION('ref_axis',(0.,-1.,0.));
#19912=DIRECTION('center_axis',(-1.,0.,0.));
#19913=DIRECTION('ref_axis',(0.,0.,1.));
#19914=DIRECTION('center_axis',(1.,0.,0.));
#19915=DIRECTION('ref_axis',(0.,0.,-1.));
#19916=DIRECTION('center_axis',(1.,0.,0.));
#19917=DIRECTION('ref_axis',(0.,1.,0.));
#19918=DIRECTION('center_axis',(1.,0.,0.));
#19919=DIRECTION('ref_axis',(0.,0.,-1.));
#19920=DIRECTION('',(-0.707106781186547,0.707106781186548,8.65956056235493E-17));
#19921=DIRECTION('center_axis',(1.,0.,0.));
#19922=DIRECTION('ref_axis',(0.,1.,0.));
#19923=DIRECTION('center_axis',(1.,0.,0.));
#19924=DIRECTION('ref_axis',(0.,0.,-1.));
#19925=DIRECTION('',(-1.,0.,0.));
#19926=DIRECTION('center_axis',(1.,0.,0.));
#19927=DIRECTION('ref_axis',(0.,1.,0.));
#19928=DIRECTION('center_axis',(1.,0.,0.));
#19929=DIRECTION('ref_axis',(0.,0.,-1.));
#19930=DIRECTION('',(-1.,0.,0.));
#19931=DIRECTION('center_axis',(1.,0.,0.));
#19932=DIRECTION('ref_axis',(0.,0.,-1.));
#19933=DIRECTION('axis',(0.,0.,1.));
#19934=DIRECTION('refdir',(1.,0.,0.));
#19935=DIRECTION('center_axis',(-1.,0.,-1.53376356854657E-14));
#19936=DIRECTION('ref_axis',(0.,-1.,-3.09974638881766E-17));
#19937=DIRECTION('center_axis',(-1.,0.,0.));
#19938=DIRECTION('ref_axis',(0.,-1.,0.));
#19939=DIRECTION('',(-0.16018224300696,0.987087457637498,-2.30533632915147E-15));
#19940=DIRECTION('center_axis',(1.,0.,0.));
#19941=DIRECTION('ref_axis',(0.,-1.,-6.12323399573677E-17));
#19942=DIRECTION('center_axis',(1.,0.,0.));
#19943=DIRECTION('ref_axis',(0.,-1.,-6.12323399573677E-17));
#19944=DIRECTION('center_axis',(1.,0.,0.));
#19945=DIRECTION('ref_axis',(0.,0.,-1.));
#19946=DIRECTION('center_axis',(1.,0.,0.));
#19947=DIRECTION('ref_axis',(0.,-1.,0.));
#19948=DIRECTION('center_axis',(-1.,0.,0.));
#19949=DIRECTION('ref_axis',(0.,1.,0.));
#19950=DIRECTION('',(-0.316227766016838,-0.948683298050514,-1.16180196436212E-16));
#19951=DIRECTION('center_axis',(1.,0.,0.));
#19952=DIRECTION('ref_axis',(0.,0.,-1.));
#19953=DIRECTION('center_axis',(-1.,0.,0.));
#19954=DIRECTION('ref_axis',(0.,-1.,0.));
#19955=DIRECTION('center_axis',(-1.,0.,0.));
#19956=DIRECTION('ref_axis',(0.,-1.,0.));
#19957=DIRECTION('',(0.707106781186549,-0.707106781186546,8.65956056235491E-17));
#19958=DIRECTION('center_axis',(1.,0.,0.));
#19959=DIRECTION('ref_axis',(0.,-1.,0.));
#19960=DIRECTION('center_axis',(1.,0.,0.));
#19961=DIRECTION('ref_axis',(0.,-1.,0.));
#19962=DIRECTION('center_axis',(1.,0.,0.));
#19963=DIRECTION('ref_axis',(0.,1.,0.));
#19964=DIRECTION('center_axis',(-1.,0.,0.));
#19965=DIRECTION('ref_axis',(0.,-1.,0.));
#19966=DIRECTION('center_axis',(-1.,0.,0.));
#19967=DIRECTION('ref_axis',(0.,-1.,0.));
#19968=DIRECTION('',(-1.,0.,0.));
#19969=DIRECTION('center_axis',(-1.,0.,0.));
#19970=DIRECTION('ref_axis',(0.,0.,1.));
#19971=DIRECTION('center_axis',(1.,0.,0.));
#19972=DIRECTION('ref_axis',(0.,0.,-1.));
#19973=DIRECTION('center_axis',(1.,0.,0.));
#19974=DIRECTION('ref_axis',(0.,-1.,0.));
#19975=DIRECTION('',(0.707106781186542,0.707106781186553,-8.659560562355E-17));
#19976=DIRECTION('center_axis',(1.,0.,0.));
#19977=DIRECTION('ref_axis',(0.,1.,0.));
#19978=DIRECTION('',(-1.,0.,0.));
#19979=DIRECTION('axis',(0.,0.,1.));
#19980=DIRECTION('refdir',(1.,0.,0.));
#19981=DIRECTION('center_axis',(1.,0.,0.));
#19982=DIRECTION('ref_axis',(0.,1.,0.));
#19983=DIRECTION('',(-1.,0.,0.));
#19984=DIRECTION('center_axis',(1.,0.,0.));
#19985=DIRECTION('ref_axis',(0.,1.,0.));
#19986=DIRECTION('center_axis',(1.,0.,0.));
#19987=DIRECTION('ref_axis',(0.,1.,0.));
#19988=DIRECTION('',(-1.,0.,0.));
#19989=DIRECTION('center_axis',(1.,0.,0.));
#19990=DIRECTION('ref_axis',(0.,1.,0.));
#19991=DIRECTION('',(-1.,0.,0.));
#19992=DIRECTION('center_axis',(1.,0.,0.));
#19993=DIRECTION('ref_axis',(0.,1.,0.));
#19994=DIRECTION('',(-1.,0.,0.));
#19995=DIRECTION('center_axis',(1.,0.,0.));
#19996=DIRECTION('ref_axis',(0.,1.,0.));
#19997=DIRECTION('',(-1.,0.,0.));
#19998=DIRECTION('center_axis',(1.,0.,0.));
#19999=DIRECTION('ref_axis',(0.,1.,0.));
#20000=DIRECTION('',(-1.,0.,0.));
#20001=DIRECTION('center_axis',(1.,0.,0.));
#20002=DIRECTION('ref_axis',(0.,1.,0.));
#20003=DIRECTION('',(-1.,0.,0.));
#20004=DIRECTION('center_axis',(1.,0.,0.));
#20005=DIRECTION('ref_axis',(0.,1.,0.));
#20006=DIRECTION('',(-1.,0.,0.));
#20007=DIRECTION('center_axis',(1.,0.,0.));
#20008=DIRECTION('ref_axis',(0.,1.,0.));
#20009=DIRECTION('',(-1.,0.,0.));
#20010=DIRECTION('center_axis',(1.,0.,0.));
#20011=DIRECTION('ref_axis',(0.,1.,0.));
#20012=DIRECTION('',(-1.,0.,0.));
#20013=DIRECTION('center_axis',(1.,0.,0.));
#20014=DIRECTION('ref_axis',(0.,1.,0.));
#20015=DIRECTION('',(-1.,0.,0.));
#20016=DIRECTION('center_axis',(1.,0.,0.));
#20017=DIRECTION('ref_axis',(0.,1.,0.));
#20018=DIRECTION('',(-1.,0.,0.));
#20019=DIRECTION('center_axis',(1.,0.,0.));
#20020=DIRECTION('ref_axis',(0.,1.,0.));
#20021=DIRECTION('',(-1.,0.,0.));
#20022=DIRECTION('center_axis',(1.,0.,0.));
#20023=DIRECTION('ref_axis',(0.,1.,0.));
#20024=DIRECTION('',(-1.,0.,0.));
#20025=DIRECTION('center_axis',(1.,0.,0.));
#20026=DIRECTION('ref_axis',(0.,1.,0.));
#20027=DIRECTION('',(-1.,0.,0.));
#20028=DIRECTION('center_axis',(1.,0.,0.));
#20029=DIRECTION('ref_axis',(0.,-0.313365996365904,-0.949632430112622));
#20030=DIRECTION('',(1.,0.,0.));
#20031=DIRECTION('center_axis',(1.,0.,0.));
#20032=DIRECTION('ref_axis',(0.,1.,8.41174344736429E-14));
#20033=DIRECTION('center_axis',(1.,0.,0.));
#20034=DIRECTION('ref_axis',(0.,1.,8.41174344736429E-14));
#20035=DIRECTION('',(1.,0.,0.));
#20036=DIRECTION('center_axis',(1.,0.,0.));
#20037=DIRECTION('ref_axis',(0.,1.,8.41174344736429E-14));
#20038=DIRECTION('',(1.,0.,0.));
#20039=DIRECTION('center_axis',(1.,0.,0.));
#20040=DIRECTION('ref_axis',(0.,1.,8.41174344736429E-14));
#20041=DIRECTION('',(1.,0.,0.));
#20042=DIRECTION('center_axis',(1.,0.,0.));
#20043=DIRECTION('ref_axis',(0.,1.,8.41174344736429E-14));
#20044=DIRECTION('',(1.,0.,0.));
#20045=DIRECTION('center_axis',(1.,0.,0.));
#20046=DIRECTION('ref_axis',(0.,1.,8.41174344736429E-14));
#20047=DIRECTION('',(1.,0.,0.));
#20048=DIRECTION('center_axis',(1.,0.,0.));
#20049=DIRECTION('ref_axis',(0.,1.,8.41174344736429E-14));
#20050=DIRECTION('',(1.,0.,0.));
#20051=DIRECTION('center_axis',(1.,0.,0.));
#20052=DIRECTION('ref_axis',(0.,1.,8.41174344736429E-14));
#20053=DIRECTION('',(1.,0.,0.));
#20054=DIRECTION('center_axis',(1.,0.,0.));
#20055=DIRECTION('ref_axis',(0.,1.,8.41174344736429E-14));
#20056=DIRECTION('',(1.,0.,0.));
#20057=DIRECTION('center_axis',(1.,0.,0.));
#20058=DIRECTION('ref_axis',(0.,1.,8.41174344736429E-14));
#20059=DIRECTION('',(1.,0.,0.));
#20060=DIRECTION('center_axis',(1.,0.,0.));
#20061=DIRECTION('ref_axis',(0.,1.,8.41174344736429E-14));
#20062=DIRECTION('',(1.,0.,0.));
#20063=DIRECTION('center_axis',(1.,0.,0.));
#20064=DIRECTION('ref_axis',(0.,1.,8.41174344736429E-14));
#20065=DIRECTION('',(1.,0.,0.));
#20066=DIRECTION('center_axis',(1.,0.,0.));
#20067=DIRECTION('ref_axis',(0.,1.,8.41174344736429E-14));
#20068=DIRECTION('',(1.,0.,0.));
#20069=DIRECTION('center_axis',(1.,0.,0.));
#20070=DIRECTION('ref_axis',(0.,1.,8.41174344736429E-14));
#20071=DIRECTION('',(1.,0.,0.));
#20072=DIRECTION('center_axis',(1.,0.,0.));
#20073=DIRECTION('ref_axis',(0.,1.,8.41174344736429E-14));
#20074=DIRECTION('',(1.,0.,0.));
#20075=DIRECTION('center_axis',(1.,0.,0.));
#20076=DIRECTION('ref_axis',(0.,1.,0.));
#20077=DIRECTION('',(-1.,0.,0.));
#20078=DIRECTION('center_axis',(-1.,0.,0.));
#20079=DIRECTION('ref_axis',(0.,1.,0.));
#20080=DIRECTION('center_axis',(1.,0.,0.));
#20081=DIRECTION('ref_axis',(0.,1.,0.));
#20082=DIRECTION('',(-1.,0.,0.));
#20083=DIRECTION('center_axis',(1.,0.,0.));
#20084=DIRECTION('ref_axis',(0.,1.,0.));
#20085=DIRECTION('',(-1.,0.,0.));
#20086=DIRECTION('center_axis',(1.,0.,0.));
#20087=DIRECTION('ref_axis',(0.,1.,0.));
#20088=DIRECTION('',(-1.,0.,0.));
#20089=DIRECTION('center_axis',(1.,0.,0.));
#20090=DIRECTION('ref_axis',(0.,1.,0.));
#20091=DIRECTION('',(-1.,0.,0.));
#20092=DIRECTION('center_axis',(1.,0.,0.));
#20093=DIRECTION('ref_axis',(0.,1.,0.));
#20094=DIRECTION('',(-1.,0.,0.));
#20095=DIRECTION('center_axis',(1.,0.,0.));
#20096=DIRECTION('ref_axis',(0.,1.,0.));
#20097=DIRECTION('',(-1.,0.,0.));
#20098=DIRECTION('center_axis',(1.,0.,0.));
#20099=DIRECTION('ref_axis',(0.,1.,0.));
#20100=DIRECTION('',(-1.,0.,0.));
#20101=DIRECTION('center_axis',(1.,0.,0.));
#20102=DIRECTION('ref_axis',(0.,1.,0.));
#20103=DIRECTION('',(-1.,0.,0.));
#20104=DIRECTION('center_axis',(1.,0.,0.));
#20105=DIRECTION('ref_axis',(0.,1.,0.));
#20106=DIRECTION('',(-1.,0.,0.));
#20107=DIRECTION('center_axis',(1.,0.,0.));
#20108=DIRECTION('ref_axis',(0.,1.,0.));
#20109=DIRECTION('',(-1.,0.,0.));
#20110=DIRECTION('center_axis',(1.,0.,0.));
#20111=DIRECTION('ref_axis',(0.,1.,0.));
#20112=DIRECTION('',(-1.,0.,0.));
#20113=DIRECTION('center_axis',(1.,0.,0.));
#20114=DIRECTION('ref_axis',(0.,1.,0.));
#20115=DIRECTION('',(-1.,0.,0.));
#20116=DIRECTION('center_axis',(1.,0.,0.));
#20117=DIRECTION('ref_axis',(0.,1.,0.));
#20118=DIRECTION('',(-1.,0.,0.));
#20119=DIRECTION('center_axis',(1.,0.,0.));
#20120=DIRECTION('ref_axis',(0.,1.,0.));
#20121=DIRECTION('',(-1.,0.,0.));
#20122=DIRECTION('center_axis',(1.,0.,0.));
#20123=DIRECTION('ref_axis',(0.,-0.313365995386845,-0.949632430435699));
#20124=DIRECTION('',(1.,0.,0.));
#20125=DIRECTION('center_axis',(1.,0.,0.));
#20126=DIRECTION('ref_axis',(0.,1.,8.41174344736429E-14));
#20127=DIRECTION('center_axis',(1.,0.,0.));
#20128=DIRECTION('ref_axis',(0.,1.,8.41174344736429E-14));
#20129=DIRECTION('',(1.,0.,0.));
#20130=DIRECTION('center_axis',(1.,0.,0.));
#20131=DIRECTION('ref_axis',(0.,1.,8.41174344736429E-14));
#20132=DIRECTION('',(1.,0.,0.));
#20133=DIRECTION('center_axis',(1.,0.,0.));
#20134=DIRECTION('ref_axis',(0.,1.,8.41174344736429E-14));
#20135=DIRECTION('',(1.,0.,0.));
#20136=DIRECTION('center_axis',(1.,0.,0.));
#20137=DIRECTION('ref_axis',(0.,1.,8.41174344736429E-14));
#20138=DIRECTION('',(1.,0.,0.));
#20139=DIRECTION('center_axis',(1.,0.,0.));
#20140=DIRECTION('ref_axis',(0.,1.,8.41174344736429E-14));
#20141=DIRECTION('',(1.,0.,0.));
#20142=DIRECTION('center_axis',(1.,0.,0.));
#20143=DIRECTION('ref_axis',(0.,1.,8.41174344736429E-14));
#20144=DIRECTION('',(1.,0.,0.));
#20145=DIRECTION('center_axis',(1.,0.,0.));
#20146=DIRECTION('ref_axis',(0.,1.,8.41174344736429E-14));
#20147=DIRECTION('',(1.,0.,0.));
#20148=DIRECTION('center_axis',(1.,0.,0.));
#20149=DIRECTION('ref_axis',(0.,1.,8.41174344736429E-14));
#20150=DIRECTION('',(1.,0.,0.));
#20151=DIRECTION('center_axis',(1.,0.,0.));
#20152=DIRECTION('ref_axis',(0.,1.,8.41174344736429E-14));
#20153=DIRECTION('',(1.,0.,0.));
#20154=DIRECTION('center_axis',(1.,0.,0.));
#20155=DIRECTION('ref_axis',(0.,1.,8.41174344736429E-14));
#20156=DIRECTION('',(1.,0.,0.));
#20157=DIRECTION('center_axis',(1.,0.,0.));
#20158=DIRECTION('ref_axis',(0.,1.,8.41174344736429E-14));
#20159=DIRECTION('',(1.,0.,0.));
#20160=DIRECTION('center_axis',(1.,0.,0.));
#20161=DIRECTION('ref_axis',(0.,1.,8.41174344736429E-14));
#20162=DIRECTION('',(1.,0.,0.));
#20163=DIRECTION('center_axis',(1.,0.,0.));
#20164=DIRECTION('ref_axis',(0.,1.,8.41174344736429E-14));
#20165=DIRECTION('',(1.,0.,0.));
#20166=DIRECTION('center_axis',(1.,0.,0.));
#20167=DIRECTION('ref_axis',(0.,1.,8.41174344736429E-14));
#20168=DIRECTION('',(1.,0.,0.));
#20169=DIRECTION('center_axis',(1.,0.,0.));
#20170=DIRECTION('ref_axis',(0.,0.,-1.));
#20171=DIRECTION('center_axis',(-1.,0.,0.));
#20172=DIRECTION('ref_axis',(0.,1.,0.));
#20173=DIRECTION('center_axis',(-1.,0.,0.));
#20174=DIRECTION('ref_axis',(0.,1.,0.));
#20175=DIRECTION('center_axis',(1.,0.,0.));
#20176=DIRECTION('ref_axis',(0.,0.888917223619435,0.458067865662629));
#20177=DIRECTION('center_axis',(-1.,0.,0.));
#20178=DIRECTION('ref_axis',(0.,1.,8.41174344736429E-14));
#20179=DIRECTION('center_axis',(1.,0.,0.));
#20180=DIRECTION('ref_axis',(0.,1.,0.));
#20181=DIRECTION('center_axis',(-1.,0.,0.));
#20182=DIRECTION('ref_axis',(0.,1.,0.));
#20183=DIRECTION('center_axis',(1.,0.,0.));
#20184=DIRECTION('ref_axis',(0.,0.,-1.));
#20185=DIRECTION('center_axis',(1.,0.,0.));
#20186=DIRECTION('ref_axis',(0.,1.,0.));
#20187=DIRECTION('center_axis',(1.,0.,0.));
#20188=DIRECTION('ref_axis',(0.,1.,0.));
#20189=DIRECTION('center_axis',(-1.,0.,0.));
#20190=DIRECTION('ref_axis',(0.,1.,8.41174344736429E-14));
#20191=DIRECTION('center_axis',(1.,0.,0.));
#20192=DIRECTION('ref_axis',(0.,0.888917222728707,0.458067867391156));
#20193=DIRECTION('center_axis',(-1.,0.,0.));
#20194=DIRECTION('ref_axis',(0.,0.,1.));
#20195=DIRECTION('center_axis',(1.,0.,0.));
#20196=DIRECTION('ref_axis',(0.,0.,-1.));
#20197=DIRECTION('center_axis',(1.,0.,0.));
#20198=DIRECTION('ref_axis',(0.,1.,0.));
#20199=DIRECTION('',(-0.707106781186546,0.707106781186549,8.65956056235495E-17));
#20200=DIRECTION('center_axis',(1.,0.,0.));
#20201=DIRECTION('ref_axis',(0.,1.,0.));
#20202=DIRECTION('center_axis',(1.,0.,0.));
#20203=DIRECTION('ref_axis',(0.,1.,0.));
#20204=DIRECTION('center_axis',(-1.,0.,0.));
#20205=DIRECTION('ref_axis',(0.,0.,1.));
#20206=DIRECTION('center_axis',(1.,0.,0.));
#20207=DIRECTION('ref_axis',(0.,0.,-1.));
#20208=DIRECTION('center_axis',(1.,0.,0.));
#20209=DIRECTION('ref_axis',(0.,1.,0.));
#20210=DIRECTION('center_axis',(1.,0.,0.));
#20211=DIRECTION('ref_axis',(0.,0.,-1.));
#20212=DIRECTION('',(-1.,0.,0.));
#20213=DIRECTION('center_axis',(1.,0.,0.));
#20214=DIRECTION('ref_axis',(0.,0.,-1.));
#20215=DIRECTION('center_axis',(-1.,0.,0.));
#20216=DIRECTION('ref_axis',(0.,1.,0.));
#20217=DIRECTION('center_axis',(1.,0.,0.));
#20218=DIRECTION('ref_axis',(0.,0.,-1.));
#20219=DIRECTION('',(-0.707106781186546,-0.707106781186549,-8.65956056235495E-17));
#20220=DIRECTION('center_axis',(1.,0.,0.));
#20221=DIRECTION('ref_axis',(0.,0.,-1.));
#20222=DIRECTION('axis',(0.,0.,1.));
#20223=DIRECTION('refdir',(1.,0.,0.));
#20224=DIRECTION('center_axis',(-1.,0.,-2.84206292975234E-15));
#20225=DIRECTION('ref_axis',(0.,1.,3.18972570729564E-17));
#20226=DIRECTION('center_axis',(-1.,0.,0.));
#20227=DIRECTION('ref_axis',(0.,1.,0.));
#20228=DIRECTION('',(-0.25906346438713,-0.965860301192537,-8.85366735539473E-16));
#20229=DIRECTION('center_axis',(1.,0.,0.));
#20230=DIRECTION('ref_axis',(0.,1.,6.12323399573677E-17));
#20231=DIRECTION('center_axis',(1.,0.,0.));
#20232=DIRECTION('ref_axis',(0.,1.,6.12323399573677E-17));
#20233=DIRECTION('center_axis',(1.,0.,0.));
#20234=DIRECTION('ref_axis',(0.,1.,6.12323399573677E-17));
#20235=DIRECTION('center_axis',(1.,0.,0.));
#20236=DIRECTION('ref_axis',(0.,1.,6.12323399573677E-17));
#20237=DIRECTION('center_axis',(1.,0.,0.));
#20238=DIRECTION('ref_axis',(0.,1.,6.12323399573677E-17));
#20239=DIRECTION('center_axis',(1.,0.,0.));
#20240=DIRECTION('ref_axis',(0.,1.,6.12323399573677E-17));
#20241=DIRECTION('center_axis',(-1.,0.,0.));
#20242=DIRECTION('ref_axis',(0.,1.,0.));
#20243=DIRECTION('center_axis',(-1.,0.,0.));
#20244=DIRECTION('ref_axis',(0.,1.,0.));
#20245=DIRECTION('center_axis',(-1.,0.,0.));
#20246=DIRECTION('ref_axis',(0.,1.,0.));
#20247=DIRECTION('center_axis',(-1.,0.,0.));
#20248=DIRECTION('ref_axis',(0.,1.,0.));
#20249=DIRECTION('center_axis',(-1.,0.,0.));
#20250=DIRECTION('ref_axis',(0.,1.,0.));
#20251=DIRECTION('center_axis',(-1.,0.,0.));
#20252=DIRECTION('ref_axis',(0.,1.,0.));
#20253=DIRECTION('center_axis',(1.,0.,0.));
#20254=DIRECTION('ref_axis',(0.,0.,-1.));
#20255=DIRECTION('center_axis',(-1.,0.,0.));
#20256=DIRECTION('ref_axis',(0.,1.,0.));
#20257=DIRECTION('center_axis',(0.369289098563654,0.804810021844156,-0.464657282759296));
#20258=DIRECTION('ref_axis',(-0.782867463262138,0.,-0.622188504366245));
#20259=DIRECTION('',(-1.31968027496911E-14,-0.499999999999999,-0.866025403784439));
#20260=DIRECTION('center_axis',(0.36928909856366,-9.22265434949625E-13,
-0.929314565516994));
#20261=DIRECTION('ref_axis',(-0.929314565516994,0.,-0.36928909856366));
#20262=DIRECTION('',(-1.13115452140209E-14,-1.,-1.88525753567016E-15));
#20263=DIRECTION('center_axis',(0.369289098563657,0.804810021845078,0.464657282757696));
#20264=DIRECTION('ref_axis',(0.782867463261092,0.,-0.622188504367561));
#20265=DIRECTION('',(-1.31968027496911E-14,0.500000000000001,-0.866025403784438));
#20266=DIRECTION('center_axis',(0.369289098563656,-0.804810021845079,-0.464657282757697));
#20267=DIRECTION('ref_axis',(-0.782867463261094,0.,-0.622188504367559));
#20268=DIRECTION('',(-1.31968027496911E-14,-0.499999999999999,0.866025403784439));
#20269=DIRECTION('center_axis',(0.369289098563656,9.24740123922532E-13,
0.929314565516996));
#20270=DIRECTION('ref_axis',(0.929314565516995,0.,-0.369289098563656));
#20271=DIRECTION('',(-1.50820602853613E-14,1.,1.88525753567016E-15));
#20272=DIRECTION('center_axis',(0.369289098563655,-0.804810021844154,0.4646572827593));
#20273=DIRECTION('ref_axis',(0.78286746326214,0.,-0.622188504366242));
#20274=DIRECTION('',(-2.07378328923717E-14,0.500000000000004,0.866025403784436));
#20275=DIRECTION('center_axis',(0.,-0.866025403784437,0.500000000000004));
#20276=DIRECTION('ref_axis',(1.,0.,0.));
#20277=DIRECTION('',(1.,0.,0.));
#20278=DIRECTION('',(-1.,0.,0.));
#20279=DIRECTION('center_axis',(0.,-1.88525753567016E-15,1.));
#20280=DIRECTION('ref_axis',(1.,0.,0.));
#20281=DIRECTION('',(1.,0.,0.));
#20282=DIRECTION('',(-1.,0.,0.));
#20283=DIRECTION('center_axis',(0.,-0.866025403784439,-0.499999999999999));
#20284=DIRECTION('ref_axis',(0.,0.499999999999999,-0.866025403784439));
#20285=DIRECTION('',(1.,0.,0.));
#20286=DIRECTION('',(-1.,0.,0.));
#20287=DIRECTION('center_axis',(0.,0.866025403784438,0.500000000000001));
#20288=DIRECTION('ref_axis',(1.,0.,0.));
#20289=DIRECTION('',(1.,0.,0.));
#20290=DIRECTION('',(-1.,0.,0.));
#20291=DIRECTION('center_axis',(0.,1.88525753567016E-15,-1.));
#20292=DIRECTION('ref_axis',(-1.,0.,0.));
#20293=DIRECTION('',(1.,0.,0.));
#20294=DIRECTION('',(-1.,0.,0.));
#20295=DIRECTION('center_axis',(0.,0.866025403784439,-0.499999999999999));
#20296=DIRECTION('ref_axis',(0.,0.499999999999999,0.866025403784439));
#20297=DIRECTION('',(1.,0.,0.));
#20298=DIRECTION('',(-1.,0.,0.));
#20299=DIRECTION('center_axis',(0.,0.5,0.866025403784439));
#20300=DIRECTION('ref_axis',(0.,-0.866025403784439,0.5));
#20301=DIRECTION('center_axis',(0.,1.,-3.60555503696918E-16));
#20302=DIRECTION('ref_axis',(0.,3.60555503696918E-16,1.));
#20303=DIRECTION('center_axis',(0.,0.5,-0.866025403784439));
#20304=DIRECTION('ref_axis',(0.,0.866025403784439,0.5));
#20305=DIRECTION('center_axis',(1.,0.,0.));
#20306=DIRECTION('ref_axis',(0.,1.,0.));
#20307=DIRECTION('center_axis',(-1.,0.,0.));
#20308=DIRECTION('ref_axis',(0.,1.,0.));
#20309=DIRECTION('',(0.500438231481872,-0.865772242839476,-1.06026520598399E-16));
#20310=DIRECTION('center_axis',(-1.,0.,0.));
#20311=DIRECTION('ref_axis',(0.,1.,0.));
#20312=DIRECTION('center_axis',(1.,0.,0.));
#20313=DIRECTION('ref_axis',(0.,1.,0.));
#20314=DIRECTION('',(0.78086880944303,0.624695047554425,7.6503079043073E-17));
#20315=DIRECTION('center_axis',(1.,0.,0.));
#20316=DIRECTION('ref_axis',(0.,0.,-1.));
#20317=DIRECTION('center_axis',(1.,0.,0.));
#20318=DIRECTION('ref_axis',(0.,1.,0.));
#20319=DIRECTION('',(1.,0.,0.));
#20320=DIRECTION('center_axis',(1.,0.,0.));
#20321=DIRECTION('ref_axis',(0.,0.,-1.));
#20322=DIRECTION('center_axis',(1.,0.,0.));
#20323=DIRECTION('ref_axis',(0.,1.,0.));
#20324=DIRECTION('',(0.780868809443029,-0.624695047554425,-7.6503079043073E-17));
#20325=DIRECTION('center_axis',(0.,-0.5,-0.866025403784439));
#20326=DIRECTION('ref_axis',(0.,0.866025403784439,-0.5));
#20327=DIRECTION('center_axis',(0.,-1.,-1.20185167898973E-16));
#20328=DIRECTION('ref_axis',(0.,1.20185167898973E-16,-1.));
#20329=DIRECTION('center_axis',(0.,-0.5,0.866025403784439));
#20330=DIRECTION('ref_axis',(0.,-0.866025403784439,-0.5));
#20331=DIRECTION('center_axis',(1.,0.,0.));
#20332=DIRECTION('ref_axis',(0.,0.,-1.));
#20333=DIRECTION('axis',(0.,0.,1.));
#20334=DIRECTION('refdir',(1.,0.,0.));
#20335=DIRECTION('center_axis',(-1.,0.,0.));
#20336=DIRECTION('ref_axis',(0.,-1.,0.));
#20337=DIRECTION('center_axis',(-1.,0.,0.));
#20338=DIRECTION('ref_axis',(0.,-1.,0.));
#20339=DIRECTION('',(0.70710678118654,-0.707106781186555,8.65956056235503E-17));
#20340=DIRECTION('center_axis',(1.,0.,0.));
#20341=DIRECTION('ref_axis',(0.,-1.,0.));
#20342=DIRECTION('center_axis',(1.,0.,0.));
#20343=DIRECTION('ref_axis',(0.,-1.,0.));
#20344=DIRECTION('center_axis',(1.,0.,0.));
#20345=DIRECTION('ref_axis',(0.,0.,-1.));
#20346=DIRECTION('center_axis',(1.,0.,0.));
#20347=DIRECTION('ref_axis',(0.,0.,-1.));
#20348=DIRECTION('center_axis',(1.,0.,0.));
#20349=DIRECTION('ref_axis',(0.,1.,0.));
#20350=DIRECTION('',(1.,0.,0.));
#20351=DIRECTION('',(1.,0.,0.));
#20352=DIRECTION('',(1.,0.,0.));
#20353=DIRECTION('center_axis',(1.,0.,0.));
#20354=DIRECTION('ref_axis',(0.,0.,-1.));
#20355=DIRECTION('center_axis',(0.656178714924787,0.,-0.754605522163505));
#20356=DIRECTION('ref_axis',(0.754605522163505,0.,0.656178714924787));
#20357=DIRECTION('center_axis',(-0.656178714924787,0.,-0.754605522163505));
#20358=DIRECTION('ref_axis',(-0.754605522163505,0.,0.656178714924787));
#20359=DIRECTION('center_axis',(0.656178714924787,0.,-0.754605522163505));
#20360=DIRECTION('ref_axis',(0.754605522163505,0.,0.656178714924787));
#20361=DIRECTION('center_axis',(-0.656178714924787,0.,-0.754605522163505));
#20362=DIRECTION('ref_axis',(-0.754605522163505,0.,0.656178714924787));
#20363=DIRECTION('center_axis',(1.,0.,0.));
#20364=DIRECTION('ref_axis',(0.,1.,0.));
#20365=DIRECTION('center_axis',(1.,0.,0.));
#20366=DIRECTION('ref_axis',(0.,1.,0.));
#20367=DIRECTION('',(-0.707106781186552,0.707106781186543,8.65956056235488E-17));
#20368=DIRECTION('center_axis',(-1.,0.,0.));
#20369=DIRECTION('ref_axis',(0.,1.,0.));
#20370=DIRECTION('center_axis',(1.,0.,0.));
#20371=DIRECTION('ref_axis',(0.,0.,-1.));
#20372=DIRECTION('center_axis',(-1.,0.,0.));
#20373=DIRECTION('ref_axis',(0.,1.,-1.43254583822601E-16));
#20374=DIRECTION('center_axis',(1.,0.,0.));
#20375=DIRECTION('ref_axis',(0.,1.,0.));
#20376=DIRECTION('center_axis',(1.,0.,0.));
#20377=DIRECTION('ref_axis',(0.,0.,-1.));
#20378=DIRECTION('',(1.,0.,0.));
#20379=DIRECTION('center_axis',(-1.,0.,0.));
#20380=DIRECTION('ref_axis',(0.,1.,-1.43254583822601E-16));
#20381=DIRECTION('center_axis',(1.,0.,0.));
#20382=DIRECTION('ref_axis',(0.,1.,-1.43254583822601E-16));
#20383=DIRECTION('center_axis',(0.,2.07899039078655E-17,1.));
#20384=DIRECTION('ref_axis',(0.,-1.,2.07899039078655E-17));
#20385=DIRECTION('center_axis',(1.,0.,0.));
#20386=DIRECTION('ref_axis',(0.,1.,0.));
#20387=DIRECTION('',(-1.,0.,0.));
#20388=DIRECTION('center_axis',(-1.,0.,0.));
#20389=DIRECTION('ref_axis',(0.,-1.,1.83697019872103E-16));
#20390=DIRECTION('center_axis',(-1.,0.,0.));
#20391=DIRECTION('ref_axis',(0.,-1.,1.83697019872103E-16));
#20392=DIRECTION('center_axis',(1.,0.,0.));
#20393=DIRECTION('ref_axis',(0.,0.,-1.));
#20394=DIRECTION('center_axis',(0.,-1.,-1.22464679914735E-16));
#20395=DIRECTION('ref_axis',(0.,-1.22464679914735E-16,1.));
#20396=DIRECTION('center_axis',(1.,0.,0.));
#20397=DIRECTION('ref_axis',(0.,-1.,1.83697019872103E-16));
#20398=DIRECTION('center_axis',(-1.,0.,0.));
#20399=DIRECTION('ref_axis',(0.,0.,1.));
#20400=DIRECTION('center_axis',(1.,0.,0.));
#20401=DIRECTION('ref_axis',(0.,0.,-1.));
#20402=DIRECTION('center_axis',(1.,0.,0.));
#20403=DIRECTION('ref_axis',(0.,0.,-1.));
#20404=DIRECTION('center_axis',(-1.,0.,0.));
#20405=DIRECTION('ref_axis',(0.,-1.,1.83697019872103E-16));
#20406=DIRECTION('center_axis',(0.,-1.,-1.22464679914735E-16));
#20407=DIRECTION('ref_axis',(0.,-1.22464679914735E-16,1.));
#20408=DIRECTION('center_axis',(1.,0.,0.));
#20409=DIRECTION('ref_axis',(0.,-1.,1.83697019872103E-16));
#20410=DIRECTION('center_axis',(1.,0.,0.));
#20411=DIRECTION('ref_axis',(0.,-1.,1.83697019872103E-16));
#20412=DIRECTION('center_axis',(1.,0.,0.));
#20413=DIRECTION('ref_axis',(0.,1.,0.));
#20414=DIRECTION('',(-1.,0.,0.));
#20415=DIRECTION('center_axis',(-1.,0.,0.));
#20416=DIRECTION('ref_axis',(0.,1.,1.22464679914735E-16));
#20417=DIRECTION('center_axis',(1.,0.,0.));
#20418=DIRECTION('ref_axis',(0.,0.,-1.));
#20419=DIRECTION('center_axis',(1.,0.,0.));
#20420=DIRECTION('ref_axis',(0.,0.,-1.));
#20421=DIRECTION('center_axis',(1.,0.,0.));
#20422=DIRECTION('ref_axis',(0.,1.,1.22464679914735E-16));
#20423=DIRECTION('center_axis',(0.,0.,-1.));
#20424=DIRECTION('ref_axis',(0.,-1.,0.));
#20425=DIRECTION('center_axis',(1.,0.,0.));
#20426=DIRECTION('ref_axis',(0.,1.,1.22464679914735E-16));
#20427=DIRECTION('center_axis',(-1.,0.,0.));
#20428=DIRECTION('ref_axis',(0.,0.,1.));
#20429=DIRECTION('center_axis',(1.,0.,0.));
#20430=DIRECTION('ref_axis',(0.,1.,0.));
#20431=DIRECTION('center_axis',(0.,-1.,0.));
#20432=DIRECTION('ref_axis',(-0.707106781186549,0.,0.707106781186546));
#20433=DIRECTION('center_axis',(0.,-1.,0.));
#20434=DIRECTION('ref_axis',(0.,0.,1.));
#20435=DIRECTION('',(0.,-1.,0.));
#20436=DIRECTION('center_axis',(2.96059473233374E-15,1.,0.));
#20437=DIRECTION('ref_axis',(-1.,2.96059473233374E-15,1.48029736616687E-15));
#20438=DIRECTION('',(0.,1.,0.));
#20439=DIRECTION('center_axis',(0.,0.,1.));
#20440=DIRECTION('ref_axis',(1.,0.,0.));
#20441=DIRECTION('center_axis',(-1.,0.,0.));
#20442=DIRECTION('ref_axis',(0.,-1.,0.));
#20443=DIRECTION('center_axis',(0.,0.,-1.));
#20444=DIRECTION('ref_axis',(-0.707106781186547,-0.707106781186548,0.));
#20445=DIRECTION('center_axis',(0.,0.,1.));
#20446=DIRECTION('ref_axis',(-0.707106781186547,-0.707106781186548,0.));
#20447=DIRECTION('center_axis',(1.,0.,0.));
#20448=DIRECTION('ref_axis',(0.,-0.707106781186547,0.707106781186548));
#20449=DIRECTION('center_axis',(-1.,0.,0.));
#20450=DIRECTION('ref_axis',(0.,-1.,1.48029736616688E-15));
#20451=DIRECTION('',(-1.,0.,0.));
#20452=DIRECTION('',(1.,0.,0.));
#20453=DIRECTION('center_axis',(0.,0.,1.));
#20454=DIRECTION('ref_axis',(1.,0.,0.));
#20455=DIRECTION('center_axis',(-2.96059473233376E-15,-1.,0.));
#20456=DIRECTION('ref_axis',(1.,-2.96059473233376E-15,0.));
#20457=DIRECTION('center_axis',(0.,0.,-1.));
#20458=DIRECTION('ref_axis',(0.707106781186547,-0.707106781186548,0.));
#20459=DIRECTION('center_axis',(0.,0.,1.));
#20460=DIRECTION('ref_axis',(0.707106781186547,-0.707106781186548,0.));
#20461=DIRECTION('center_axis',(0.,1.,0.));
#20462=DIRECTION('ref_axis',(0.707106781186549,0.,0.707106781186546));
#20463=DIRECTION('center_axis',(-2.96059473233374E-15,-1.,0.));
#20464=DIRECTION('ref_axis',(1.,-2.96059473233374E-15,1.48029736616687E-15));
#20465=DIRECTION('',(0.,-1.,0.));
#20466=DIRECTION('',(0.,1.,0.));
#20467=DIRECTION('center_axis',(0.,0.,1.));
#20468=DIRECTION('ref_axis',(1.,0.,0.));
#20469=DIRECTION('center_axis',(1.,0.,0.));
#20470=DIRECTION('ref_axis',(0.,1.,0.));
#20471=DIRECTION('center_axis',(0.,0.,-1.));
#20472=DIRECTION('ref_axis',(0.707106781186547,0.707106781186548,0.));
#20473=DIRECTION('center_axis',(0.,0.,1.));
#20474=DIRECTION('ref_axis',(0.707106781186547,0.707106781186548,0.));
#20475=DIRECTION('center_axis',(-1.,0.,0.));
#20476=DIRECTION('ref_axis',(0.,0.707106781186547,0.707106781186548));
#20477=DIRECTION('center_axis',(1.,0.,0.));
#20478=DIRECTION('ref_axis',(0.,1.,1.48029736616688E-15));
#20479=DIRECTION('',(1.,0.,0.));
#20480=DIRECTION('',(-1.,0.,0.));
#20481=DIRECTION('center_axis',(0.,0.,1.));
#20482=DIRECTION('ref_axis',(1.,0.,0.));
#20483=DIRECTION('center_axis',(0.,0.,-1.));
#20484=DIRECTION('ref_axis',(-0.707106781186547,0.707106781186548,0.));
#20485=DIRECTION('center_axis',(0.,0.,1.));
#20486=DIRECTION('ref_axis',(-0.707106781186547,0.707106781186548,0.));
#20487=DIRECTION('center_axis',(0.,0.,1.));
#20488=DIRECTION('ref_axis',(1.48029736616687E-15,-1.,0.));
#20489=DIRECTION('',(0.,0.,1.));
#20490=DIRECTION('center_axis',(0.,0.,-1.));
#20491=DIRECTION('ref_axis',(0.707106781186547,-0.707106781186548,0.));
#20492=DIRECTION('',(0.,0.,1.));
#20493=DIRECTION('center_axis',(0.,-1.,0.));
#20494=DIRECTION('ref_axis',(1.,0.,0.));
#20495=DIRECTION('',(0.,0.,1.));
#20496=DIRECTION('',(-1.,0.,0.));
#20497=DIRECTION('center_axis',(0.,0.,1.));
#20498=DIRECTION('ref_axis',(-1.,0.,0.));
#20499=DIRECTION('',(0.,0.,1.));
#20500=DIRECTION('center_axis',(0.,0.,-1.));
#20501=DIRECTION('ref_axis',(-0.707106781186547,-0.707106781186548,0.));
#20502=DIRECTION('center_axis',(-1.,0.,0.));
#20503=DIRECTION('ref_axis',(0.,-1.,0.));
#20504=DIRECTION('',(0.,0.,1.));
#20505=DIRECTION('',(0.,1.,0.));
#20506=DIRECTION('center_axis',(-1.,0.,0.));
#20507=DIRECTION('ref_axis',(0.,1.,0.));
#20508=DIRECTION('center_axis',(0.,0.,1.));
#20509=DIRECTION('ref_axis',(1.,0.,0.));
#20510=DIRECTION('center_axis',(0.,0.,-1.));
#20511=DIRECTION('ref_axis',(1.,0.,0.));
#20512=DIRECTION('center_axis',(0.,0.,-1.));
#20513=DIRECTION('ref_axis',(1.,0.,0.));
#20514=DIRECTION('center_axis',(0.,0.,-1.));
#20515=DIRECTION('ref_axis',(1.,0.,0.));
#20516=DIRECTION('center_axis',(0.,-1.,0.));
#20517=DIRECTION('ref_axis',(-0.707106781186548,0.,-0.707106781186548));
#20518=DIRECTION('center_axis',(0.,-1.,0.));
#20519=DIRECTION('ref_axis',(-1.,0.,0.));
#20520=DIRECTION('',(0.,-1.,0.));
#20521=DIRECTION('center_axis',(2.96059473233374E-15,1.,0.));
#20522=DIRECTION('ref_axis',(0.,0.,-1.));
#20523=DIRECTION('center_axis',(0.,0.,1.));
#20524=DIRECTION('ref_axis',(1.,0.,0.));
#20525=DIRECTION('center_axis',(-1.,0.,0.));
#20526=DIRECTION('ref_axis',(0.,0.,-1.));
#20527=DIRECTION('center_axis',(0.,0.,1.));
#20528=DIRECTION('ref_axis',(-0.707106781186547,-0.707106781186548,0.));
#20529=DIRECTION('center_axis',(1.,0.,0.));
#20530=DIRECTION('ref_axis',(0.,-0.707106781186545,-0.70710678118655));
#20531=DIRECTION('center_axis',(-1.,0.,0.));
#20532=DIRECTION('ref_axis',(0.,0.,-1.));
#20533=DIRECTION('',(1.,0.,0.));
#20534=DIRECTION('center_axis',(0.,0.,1.));
#20535=DIRECTION('ref_axis',(1.,0.,0.));
#20536=DIRECTION('center_axis',(-2.96059473233376E-15,-1.,0.));
#20537=DIRECTION('ref_axis',(0.,0.,-1.));
#20538=DIRECTION('center_axis',(0.,0.,1.));
#20539=DIRECTION('ref_axis',(0.707106781186547,-0.707106781186548,0.));
#20540=DIRECTION('center_axis',(0.,1.,0.));
#20541=DIRECTION('ref_axis',(0.707106781186552,0.,-0.707106781186543));
#20542=DIRECTION('center_axis',(-2.96059473233373E-15,-1.,0.));
#20543=DIRECTION('ref_axis',(0.,0.,-1.));
#20544=DIRECTION('',(0.,-1.,0.));
#20545=DIRECTION('',(0.,1.,0.));
#20546=DIRECTION('center_axis',(0.,0.,1.));
#20547=DIRECTION('ref_axis',(1.,0.,0.));
#20548=DIRECTION('center_axis',(1.,0.,0.));
#20549=DIRECTION('ref_axis',(0.,0.,-1.));
#20550=DIRECTION('center_axis',(0.,0.,-1.));
#20551=DIRECTION('ref_axis',(0.707106781186547,0.707106781186548,0.));
#20552=DIRECTION('center_axis',(0.,0.,1.));
#20553=DIRECTION('ref_axis',(0.707106781186547,0.707106781186548,0.));
#20554=DIRECTION('center_axis',(-1.,0.,0.));
#20555=DIRECTION('ref_axis',(0.,0.707106781186545,-0.70710678118655));
#20556=DIRECTION('center_axis',(1.,0.,0.));
#20557=DIRECTION('ref_axis',(0.,0.,-1.));
#20558=DIRECTION('',(1.,0.,0.));
#20559=DIRECTION('',(-1.,0.,0.));
#20560=DIRECTION('center_axis',(0.,0.,1.));
#20561=DIRECTION('ref_axis',(1.,0.,0.));
#20562=DIRECTION('center_axis',(0.,0.,-1.));
#20563=DIRECTION('ref_axis',(-0.707106781186547,0.707106781186548,0.));
#20564=DIRECTION('center_axis',(0.,0.,1.));
#20565=DIRECTION('ref_axis',(-0.707106781186547,0.707106781186548,0.));
#20566=DIRECTION('center_axis',(0.,0.,1.));
#20567=DIRECTION('ref_axis',(1.,2.96059473233374E-15,0.));
#20568=DIRECTION('',(0.,0.,1.));
#20569=DIRECTION('',(0.,0.,1.));
#20570=DIRECTION('center_axis',(0.,1.,0.));
#20571=DIRECTION('ref_axis',(-1.,0.,0.));
#20572=DIRECTION('',(0.,0.,1.));
#20573=DIRECTION('center_axis',(0.,0.,1.));
#20574=DIRECTION('ref_axis',(1.48029736616688E-15,1.,0.));
#20575=DIRECTION('center_axis',(0.,0.,1.));
#20576=DIRECTION('ref_axis',(1.,0.,0.));
#20577=DIRECTION('center_axis',(0.,0.,1.));
#20578=DIRECTION('ref_axis',(1.,0.,0.));
#20579=DIRECTION('center_axis',(0.,0.,1.));
#20580=DIRECTION('ref_axis',(1.,0.,0.));
#20581=DIRECTION('center_axis',(0.,-1.,0.));
#20582=DIRECTION('ref_axis',(-0.707106781186549,0.,0.707106781186546));
#20583=DIRECTION('center_axis',(0.,-1.,0.));
#20584=DIRECTION('ref_axis',(0.,0.,1.));
#20585=DIRECTION('',(0.,-1.,0.));
#20586=DIRECTION('center_axis',(2.96059473233374E-15,1.,0.));
#20587=DIRECTION('ref_axis',(-1.,2.96059473233374E-15,1.48029736616687E-15));
#20588=DIRECTION('',(0.,1.,0.));
#20589=DIRECTION('center_axis',(0.,0.,1.));
#20590=DIRECTION('ref_axis',(1.,0.,0.));
#20591=DIRECTION('center_axis',(-1.,0.,0.));
#20592=DIRECTION('ref_axis',(0.,-1.,0.));
#20593=DIRECTION('center_axis',(0.,0.,-1.));
#20594=DIRECTION('ref_axis',(-0.707106781186547,-0.707106781186548,0.));
#20595=DIRECTION('center_axis',(0.,0.,1.));
#20596=DIRECTION('ref_axis',(-0.707106781186547,-0.707106781186548,0.));
#20597=DIRECTION('center_axis',(1.,0.,0.));
#20598=DIRECTION('ref_axis',(0.,-0.707106781186547,0.707106781186548));
#20599=DIRECTION('center_axis',(-1.,0.,0.));
#20600=DIRECTION('ref_axis',(0.,-1.,1.48029736616688E-15));
#20601=DIRECTION('',(-1.,0.,0.));
#20602=DIRECTION('',(1.,0.,0.));
#20603=DIRECTION('center_axis',(0.,0.,1.));
#20604=DIRECTION('ref_axis',(1.,0.,0.));
#20605=DIRECTION('center_axis',(0.,-1.,0.));
#20606=DIRECTION('ref_axis',(1.,0.,0.));
#20607=DIRECTION('center_axis',(0.,0.,-1.));
#20608=DIRECTION('ref_axis',(0.707106781186547,-0.707106781186548,0.));
#20609=DIRECTION('center_axis',(0.,0.,1.));
#20610=DIRECTION('ref_axis',(0.707106781186547,-0.707106781186548,0.));
#20611=DIRECTION('center_axis',(0.,1.,0.));
#20612=DIRECTION('ref_axis',(0.707106781186549,0.,0.707106781186546));
#20613=DIRECTION('center_axis',(-2.96059473233374E-15,-1.,0.));
#20614=DIRECTION('ref_axis',(1.,-2.96059473233374E-15,1.48029736616687E-15));
#20615=DIRECTION('',(0.,-1.,0.));
#20616=DIRECTION('',(0.,1.,0.));
#20617=DIRECTION('center_axis',(0.,0.,1.));
#20618=DIRECTION('ref_axis',(1.,0.,0.));
#20619=DIRECTION('center_axis',(1.,0.,0.));
#20620=DIRECTION('ref_axis',(0.,1.,0.));
#20621=DIRECTION('center_axis',(0.,0.,-1.));
#20622=DIRECTION('ref_axis',(0.707106781186547,0.707106781186548,0.));
#20623=DIRECTION('center_axis',(0.,0.,1.));
#20624=DIRECTION('ref_axis',(0.707106781186547,0.707106781186548,0.));
#20625=DIRECTION('center_axis',(-1.,0.,0.));
#20626=DIRECTION('ref_axis',(0.,0.707106781186547,0.707106781186548));
#20627=DIRECTION('center_axis',(1.,0.,0.));
#20628=DIRECTION('ref_axis',(0.,1.,1.48029736616688E-15));
#20629=DIRECTION('',(1.,0.,0.));
#20630=DIRECTION('',(-1.,0.,0.));
#20631=DIRECTION('center_axis',(0.,0.,1.));
#20632=DIRECTION('ref_axis',(1.,0.,0.));
#20633=DIRECTION('center_axis',(0.,0.,-1.));
#20634=DIRECTION('ref_axis',(-0.707106781186547,0.707106781186548,0.));
#20635=DIRECTION('center_axis',(0.,0.,1.));
#20636=DIRECTION('ref_axis',(-0.707106781186547,0.707106781186548,0.));
#20637=DIRECTION('center_axis',(0.,0.,1.));
#20638=DIRECTION('ref_axis',(-1.48029736616688E-15,-1.,0.));
#20639=DIRECTION('',(0.,0.,1.));
#20640=DIRECTION('center_axis',(0.,0.,-1.));
#20641=DIRECTION('ref_axis',(0.707106781186547,-0.707106781186548,0.));
#20642=DIRECTION('',(0.,0.,1.));
#20643=DIRECTION('center_axis',(0.,-1.,0.));
#20644=DIRECTION('ref_axis',(1.,0.,0.));
#20645=DIRECTION('',(0.,0.,1.));
#20646=DIRECTION('',(-1.,0.,0.));
#20647=DIRECTION('center_axis',(0.,0.,1.));
#20648=DIRECTION('ref_axis',(-1.,-2.96059473233374E-15,0.));
#20649=DIRECTION('',(0.,0.,1.));
#20650=DIRECTION('center_axis',(0.,0.,-1.));
#20651=DIRECTION('ref_axis',(-0.707106781186547,-0.707106781186548,0.));
#20652=DIRECTION('center_axis',(-1.,0.,0.));
#20653=DIRECTION('ref_axis',(0.,-1.,0.));
#20654=DIRECTION('',(0.,0.,1.));
#20655=DIRECTION('',(0.,1.,0.));
#20656=DIRECTION('center_axis',(-1.,0.,0.));
#20657=DIRECTION('ref_axis',(0.,1.,0.));
#20658=DIRECTION('center_axis',(0.,0.,1.));
#20659=DIRECTION('ref_axis',(1.,0.,0.));
#20660=DIRECTION('center_axis',(0.,0.,-1.));
#20661=DIRECTION('ref_axis',(1.,0.,0.));
#20662=DIRECTION('center_axis',(0.,0.,-1.));
#20663=DIRECTION('ref_axis',(1.,0.,0.));
#20664=DIRECTION('center_axis',(0.,0.,-1.));
#20665=DIRECTION('ref_axis',(1.,0.,0.));
#20666=DIRECTION('center_axis',(0.,-1.,0.));
#20667=DIRECTION('ref_axis',(-0.707106781186552,0.,-0.707106781186543));
#20668=DIRECTION('center_axis',(0.,-1.,0.));
#20669=DIRECTION('ref_axis',(-1.,0.,0.));
#20670=DIRECTION('',(0.,-1.,0.));
#20671=DIRECTION('center_axis',(2.96059473233373E-15,1.,0.));
#20672=DIRECTION('ref_axis',(0.,0.,-1.));
#20673=DIRECTION('center_axis',(0.,0.,1.));
#20674=DIRECTION('ref_axis',(1.,0.,0.));
#20675=DIRECTION('center_axis',(-1.,0.,0.));
#20676=DIRECTION('ref_axis',(0.,0.,-1.));
#20677=DIRECTION('center_axis',(0.,0.,1.));
#20678=DIRECTION('ref_axis',(-0.707106781186547,-0.707106781186548,0.));
#20679=DIRECTION('center_axis',(1.,0.,0.));
#20680=DIRECTION('ref_axis',(0.,-0.707106781186545,-0.70710678118655));
#20681=DIRECTION('center_axis',(-1.,0.,0.));
#20682=DIRECTION('ref_axis',(0.,0.,-1.));
#20683=DIRECTION('',(1.,0.,0.));
#20684=DIRECTION('center_axis',(0.,0.,1.));
#20685=DIRECTION('ref_axis',(1.,0.,0.));
#20686=DIRECTION('center_axis',(0.,-1.,0.));
#20687=DIRECTION('ref_axis',(0.,0.,-1.));
#20688=DIRECTION('center_axis',(0.,0.,1.));
#20689=DIRECTION('ref_axis',(0.707106781186547,-0.707106781186548,0.));
#20690=DIRECTION('center_axis',(0.,1.,0.));
#20691=DIRECTION('ref_axis',(0.707106781186548,0.,-0.707106781186548));
#20692=DIRECTION('center_axis',(-2.96059473233374E-15,-1.,0.));
#20693=DIRECTION('ref_axis',(0.,0.,-1.));
#20694=DIRECTION('',(0.,-1.,0.));
#20695=DIRECTION('',(0.,1.,0.));
#20696=DIRECTION('center_axis',(0.,0.,1.));
#20697=DIRECTION('ref_axis',(1.,0.,0.));
#20698=DIRECTION('center_axis',(1.,0.,0.));
#20699=DIRECTION('ref_axis',(0.,0.,-1.));
#20700=DIRECTION('center_axis',(0.,0.,-1.));
#20701=DIRECTION('ref_axis',(0.707106781186547,0.707106781186548,0.));
#20702=DIRECTION('center_axis',(0.,0.,1.));
#20703=DIRECTION('ref_axis',(0.707106781186547,0.707106781186548,0.));
#20704=DIRECTION('center_axis',(-1.,0.,0.));
#20705=DIRECTION('ref_axis',(0.,0.707106781186545,-0.70710678118655));
#20706=DIRECTION('center_axis',(1.,0.,0.));
#20707=DIRECTION('ref_axis',(0.,0.,-1.));
#20708=DIRECTION('',(1.,0.,0.));
#20709=DIRECTION('',(-1.,0.,0.));
#20710=DIRECTION('center_axis',(0.,0.,1.));
#20711=DIRECTION('ref_axis',(1.,0.,0.));
#20712=DIRECTION('center_axis',(0.,0.,-1.));
#20713=DIRECTION('ref_axis',(-0.707106781186547,0.707106781186548,0.));
#20714=DIRECTION('center_axis',(0.,0.,1.));
#20715=DIRECTION('ref_axis',(-0.707106781186547,0.707106781186548,0.));
#20716=DIRECTION('center_axis',(0.,0.,1.));
#20717=DIRECTION('ref_axis',(1.,0.,0.));
#20718=DIRECTION('',(0.,0.,1.));
#20719=DIRECTION('',(0.,0.,1.));
#20720=DIRECTION('center_axis',(0.,1.,0.));
#20721=DIRECTION('ref_axis',(-1.,0.,0.));
#20722=DIRECTION('',(0.,0.,1.));
#20723=DIRECTION('center_axis',(0.,0.,1.));
#20724=DIRECTION('ref_axis',(-1.48029736616687E-15,1.,0.));
#20725=DIRECTION('center_axis',(0.,0.,1.));
#20726=DIRECTION('ref_axis',(1.,0.,0.));
#20727=DIRECTION('center_axis',(0.,0.,1.));
#20728=DIRECTION('ref_axis',(1.,0.,0.));
#20729=DIRECTION('center_axis',(0.,0.,1.));
#20730=DIRECTION('ref_axis',(1.,0.,0.));
#20731=DIRECTION('center_axis',(0.754605522163505,7.28504717578445E-17,
0.656178714924787));
#20732=DIRECTION('ref_axis',(-0.656178714924787,0.,0.754605522163505));
#20733=DIRECTION('center_axis',(0.754605522163505,7.28504717578445E-17,
0.656178714924787));
#20734=DIRECTION('ref_axis',(-0.656178714924787,0.,0.754605522163505));
#20735=DIRECTION('center_axis',(-0.754605522163505,-7.28504717578445E-17,
0.656178714924787));
#20736=DIRECTION('ref_axis',(0.656178714924787,0.,0.754605522163505));
#20737=DIRECTION('center_axis',(0.754605522163505,7.28504717578445E-17,
0.656178714924787));
#20738=DIRECTION('ref_axis',(-0.656178714924787,0.,0.754605522163505));
#20739=DIRECTION('center_axis',(0.754605522163505,7.28504717578445E-17,
0.656178714924787));
#20740=DIRECTION('ref_axis',(-0.656178714924787,0.,0.754605522163505));
#20741=DIRECTION('center_axis',(-0.754605522163505,-7.28504717578445E-17,
0.656178714924787));
#20742=DIRECTION('ref_axis',(0.656178714924787,0.,0.754605522163505));
#20743=DIRECTION('center_axis',(0.,0.,-1.));
#20744=DIRECTION('ref_axis',(1.,0.,0.));
#20745=DIRECTION('',(0.,0.,-1.));
#20746=DIRECTION('center_axis',(0.,0.,-1.));
#20747=DIRECTION('ref_axis',(1.,0.,0.));
#20748=DIRECTION('',(0.,0.,-1.));
#20749=DIRECTION('center_axis',(0.,0.,-1.));
#20750=DIRECTION('ref_axis',(1.,0.,0.));
#20751=DIRECTION('',(0.,0.,-1.));
#20752=DIRECTION('center_axis',(0.,0.,-1.));
#20753=DIRECTION('ref_axis',(1.,0.,0.));
#20754=DIRECTION('',(0.,0.,-1.));
#20755=DIRECTION('center_axis',(0.,0.,-1.));
#20756=DIRECTION('ref_axis',(1.,0.,0.));
#20757=DIRECTION('',(0.,0.,-1.));
#20758=DIRECTION('center_axis',(0.,0.,-1.));
#20759=DIRECTION('ref_axis',(1.,0.,0.));
#20760=DIRECTION('',(0.,0.,-1.));
#20761=DIRECTION('center_axis',(1.,0.,0.));
#20762=DIRECTION('ref_axis',(0.,1.,0.));
#20763=DIRECTION('',(1.,0.,0.));
#20764=DIRECTION('center_axis',(-1.,0.,0.));
#20765=DIRECTION('ref_axis',(0.,0.,1.));
#20766=DIRECTION('center_axis',(1.,0.,0.));
#20767=DIRECTION('ref_axis',(0.,1.,0.));
#20768=DIRECTION('center_axis',(1.,0.,0.));
#20769=DIRECTION('ref_axis',(0.,1.,0.));
#20770=DIRECTION('center_axis',(1.,0.,0.));
#20771=DIRECTION('ref_axis',(0.,1.,0.));
#20772=DIRECTION('',(-1.,0.,0.));
#20773=DIRECTION('center_axis',(1.,0.,0.));
#20774=DIRECTION('ref_axis',(0.,1.,0.));
#20775=DIRECTION('center_axis',(1.,0.,0.));
#20776=DIRECTION('ref_axis',(0.,1.,0.));
#20777=DIRECTION('center_axis',(1.,0.,0.));
#20778=DIRECTION('ref_axis',(0.,1.,0.));
#20779=DIRECTION('',(-1.,0.,0.));
#20780=DIRECTION('center_axis',(1.,0.,0.));
#20781=DIRECTION('ref_axis',(0.,1.,0.));
#20782=DIRECTION('',(-1.,0.,0.));
#20783=DIRECTION('axis',(0.,0.,1.));
#20784=DIRECTION('refdir',(1.,0.,0.));
#20785=DIRECTION('center_axis',(1.,0.,0.));
#20786=DIRECTION('ref_axis',(0.,1.,0.));
#20787=DIRECTION('',(-1.,0.,0.));
#20788=DIRECTION('center_axis',(-1.,0.,0.));
#20789=DIRECTION('ref_axis',(0.,1.,0.));
#20790=DIRECTION('center_axis',(1.,0.,0.));
#20791=DIRECTION('ref_axis',(0.,1.,0.));
#20792=DIRECTION('',(-1.,0.,0.));
#20793=DIRECTION('center_axis',(1.,0.,0.));
#20794=DIRECTION('ref_axis',(0.,1.,0.));
#20795=DIRECTION('',(-1.,0.,0.));
#20796=DIRECTION('center_axis',(1.,0.,0.));
#20797=DIRECTION('ref_axis',(0.,1.,0.));
#20798=DIRECTION('',(-1.,0.,0.));
#20799=DIRECTION('center_axis',(1.,0.,0.));
#20800=DIRECTION('ref_axis',(0.,1.,0.));
#20801=DIRECTION('',(-1.,0.,0.));
#20802=DIRECTION('center_axis',(1.,0.,0.));
#20803=DIRECTION('ref_axis',(0.,1.,0.));
#20804=DIRECTION('',(-1.,0.,0.));
#20805=DIRECTION('center_axis',(1.,0.,0.));
#20806=DIRECTION('ref_axis',(0.,-0.979063397301506,-0.203555555228623));
#20807=DIRECTION('',(1.,0.,0.));
#20808=DIRECTION('center_axis',(1.,0.,0.));
#20809=DIRECTION('ref_axis',(0.,1.,4.09245417118841E-15));
#20810=DIRECTION('center_axis',(1.,0.,0.));
#20811=DIRECTION('ref_axis',(0.,1.,4.09245417118841E-15));
#20812=DIRECTION('',(1.,0.,0.));
#20813=DIRECTION('center_axis',(1.,0.,0.));
#20814=DIRECTION('ref_axis',(0.,1.,4.09245417118841E-15));
#20815=DIRECTION('center_axis',(1.,0.,0.));
#20816=DIRECTION('ref_axis',(0.,1.,4.09245417118841E-15));
#20817=DIRECTION('',(1.,0.,0.));
#20818=DIRECTION('center_axis',(1.,0.,0.));
#20819=DIRECTION('ref_axis',(0.,1.,4.09245417118841E-15));
#20820=DIRECTION('',(1.,0.,0.));
#20821=DIRECTION('center_axis',(1.,0.,0.));
#20822=DIRECTION('ref_axis',(0.,1.,4.09245417118841E-15));
#20823=DIRECTION('',(1.,0.,0.));
#20824=DIRECTION('center_axis',(1.,0.,0.));
#20825=DIRECTION('ref_axis',(0.,1.,4.09245417118841E-15));
#20826=DIRECTION('',(1.,0.,0.));
#20827=DIRECTION('center_axis',(-1.,0.,0.));
#20828=DIRECTION('ref_axis',(0.,-1.,0.));
#20829=DIRECTION('center_axis',(-1.,0.,0.));
#20830=DIRECTION('ref_axis',(0.,-1.,0.));
#20831=DIRECTION('',(-0.707106781186552,0.707106781186543,8.65956056235488E-17));
#20832=DIRECTION('center_axis',(1.,0.,0.));
#20833=DIRECTION('ref_axis',(0.,-1.,0.));
#20834=DIRECTION('center_axis',(1.,0.,0.));
#20835=DIRECTION('ref_axis',(0.,-1.,0.));
#20836=DIRECTION('center_axis',(1.,0.,0.));
#20837=DIRECTION('ref_axis',(0.,1.,0.));
#20838=DIRECTION('',(-1.,0.,0.));
#20839=DIRECTION('center_axis',(-1.,0.,0.));
#20840=DIRECTION('ref_axis',(0.,-1.,0.));
#20841=DIRECTION('center_axis',(-1.,0.,0.));
#20842=DIRECTION('ref_axis',(0.,-1.,0.));
#20843=DIRECTION('center_axis',(1.,0.,0.));
#20844=DIRECTION('ref_axis',(0.,0.,-1.));
#20845=DIRECTION('center_axis',(-1.,0.,0.));
#20846=DIRECTION('ref_axis',(0.,1.,4.09245417118841E-15));
#20847=DIRECTION('center_axis',(1.,0.,1.12244711165176E-15));
#20848=DIRECTION('ref_axis',(0.,-1.,-3.02741268154642E-17));
#20849=DIRECTION('',(-0.923879532511291,-0.38268343236508,-1.09545652359634E-15));
#20850=DIRECTION('center_axis',(1.,0.,0.));
#20851=DIRECTION('ref_axis',(0.,-1.,-6.12323399573677E-17));
#20852=DIRECTION('center_axis',(1.,0.,0.));
#20853=DIRECTION('ref_axis',(0.,-1.,-6.12323399573677E-17));
#20854=DIRECTION('center_axis',(1.,0.,0.));
#20855=DIRECTION('ref_axis',(0.,1.,0.));
#20856=DIRECTION('',(-0.707106781186546,0.707106781186549,8.65956056235495E-17));
#20857=DIRECTION('center_axis',(-1.,0.,0.));
#20858=DIRECTION('ref_axis',(0.,-1.,-6.12323399573677E-17));
#20859=DIRECTION('center_axis',(-1.,0.,0.));
#20860=DIRECTION('ref_axis',(0.,-1.,-6.12323399573677E-17));
#20861=DIRECTION('center_axis',(1.,0.,-2.65910050866385E-15));
#20862=DIRECTION('ref_axis',(0.,-1.,-3.14915276069828E-17));
#20863=DIRECTION('',(-0.382683432365087,-0.923879532511288,8.75356720626856E-16));
#20864=DIRECTION('center_axis',(1.,0.,0.));
#20865=DIRECTION('ref_axis',(0.,-1.,0.));
#20866=DIRECTION('center_axis',(-1.,0.,0.));
#20867=DIRECTION('ref_axis',(0.,0.,1.));
#20868=DIRECTION('',(0.,-0.866025403784439,-0.5));
#20869=DIRECTION('',(0.,-3.84592537276713E-16,-1.));
#20870=DIRECTION('',(0.,0.866025403784439,-0.5));
#20871=DIRECTION('',(0.,0.866025403784439,0.5));
#20872=DIRECTION('',(0.,-1.92296268638356E-16,1.));
#20873=DIRECTION('',(0.,-0.866025403784439,0.5));
#20874=DIRECTION('center_axis',(-0.707106781186546,0.353553390593275,-0.612372435695796));
#20875=DIRECTION('ref_axis',(-0.654653670707979,0.,0.755928946018453));
#20876=DIRECTION('',(0.654653670707981,6.27736560906509E-15,-0.755928946018451));
#20877=DIRECTION('',(0.,-0.866025403784439,-0.5));
#20878=DIRECTION('',(0.65465367070798,0.654653670707973,-0.377964473009229));
#20879=DIRECTION('center_axis',(-0.707106781186543,-0.353553390593276,-0.612372435695799));
#20880=DIRECTION('ref_axis',(-0.654653670707982,0.,0.75592894601845));
#20881=DIRECTION('',(0.654653670707982,-0.654653670707975,-0.377964473009223));
#20882=DIRECTION('',(0.,-0.866025403784439,0.5));
#20883=DIRECTION('center_axis',(-0.707106781186543,-0.353553390593276,0.612372435695799));
#20884=DIRECTION('ref_axis',(0.654653670707983,0.,0.75592894601845));
#20885=DIRECTION('',(0.654653670707981,3.69906210244107E-15,0.755928946018451));
#20886=DIRECTION('',(0.,0.866025403784439,0.5));
#20887=DIRECTION('',(-0.654653670707982,0.654653670707974,-0.377964473009224));
#20888=DIRECTION('center_axis',(-0.707106781186545,0.353553390593275,0.612372435695797));
#20889=DIRECTION('ref_axis',(0.65465367070798,0.,0.755928946018452));
#20890=DIRECTION('',(0.,0.866025403784439,-0.5));
#20891=DIRECTION('',(0.654653670707981,0.654653670707973,0.377964473009228));
#20892=DIRECTION('center_axis',(-0.707106781186543,-0.707106781186552,2.71947991102105E-16));
#20893=DIRECTION('ref_axis',(3.84592537276717E-16,0.,1.));
#20894=DIRECTION('',(0.,3.84592537276713E-16,1.));
#20895=DIRECTION('center_axis',(-0.707106781186544,0.707106781186551,1.35973995551053E-16));
#20896=DIRECTION('ref_axis',(1.92296268638359E-16,0.,1.));
#20897=DIRECTION('',(0.,1.92296268638356E-16,-1.));
#20898=DIRECTION('center_axis',(0.,0.5,0.866025403784439));
#20899=DIRECTION('ref_axis',(0.,-0.866025403784439,0.5));
#20900=DIRECTION('',(1.,0.,0.));
#20901=DIRECTION('',(0.,-0.866025403784439,0.5));
#20902=DIRECTION('',(1.,0.,0.));
#20903=DIRECTION('center_axis',(0.,1.,-3.84592537276713E-16));
#20904=DIRECTION('ref_axis',(0.,3.84592537276713E-16,1.));
#20905=DIRECTION('',(1.,0.,0.));
#20906=DIRECTION('',(0.,3.84592537276713E-16,1.));
#20907=DIRECTION('center_axis',(0.,0.5,-0.866025403784439));
#20908=DIRECTION('ref_axis',(0.,0.866025403784439,0.5));
#20909=DIRECTION('',(1.,0.,0.));
#20910=DIRECTION('',(0.,0.866025403784439,0.5));
#20911=DIRECTION('center_axis',(1.,0.,0.));
#20912=DIRECTION('ref_axis',(0.,0.,-1.));
#20913=DIRECTION('center_axis',(-1.,0.,0.));
#20914=DIRECTION('ref_axis',(0.,1.,0.));
#20915=DIRECTION('center_axis',(-1.,0.,0.));
#20916=DIRECTION('ref_axis',(0.,1.,0.));
#20917=DIRECTION('center_axis',(1.,0.,0.));
#20918=DIRECTION('ref_axis',(0.,0.888972258373966,0.457961050572524));
#20919=DIRECTION('center_axis',(1.,0.,0.));
#20920=DIRECTION('ref_axis',(0.,0.117347197905867,-0.993090950086467));
#20921=DIRECTION('center_axis',(-1.,0.,0.));
#20922=DIRECTION('ref_axis',(0.,1.,0.));
#20923=DIRECTION('center_axis',(0.,-0.5,-0.866025403784439));
#20924=DIRECTION('ref_axis',(0.,0.866025403784439,-0.5));
#20925=DIRECTION('',(1.,0.,0.));
#20926=DIRECTION('',(0.,0.866025403784439,-0.5));
#20927=DIRECTION('center_axis',(0.,-1.,-1.92296268638356E-16));
#20928=DIRECTION('ref_axis',(0.,1.92296268638356E-16,-1.));
#20929=DIRECTION('',(1.,0.,0.));
#20930=DIRECTION('',(0.,1.92296268638356E-16,-1.));
#20931=DIRECTION('center_axis',(0.,-0.5,0.866025403784439));
#20932=DIRECTION('ref_axis',(0.,-0.866025403784439,-0.5));
#20933=DIRECTION('',(0.,-0.866025403784439,-0.5));
#20934=DIRECTION('center_axis',(1.,0.,0.));
#20935=DIRECTION('ref_axis',(0.,0.,-1.));
#20936=DIRECTION('center_axis',(-1.,0.,0.));
#20937=DIRECTION('ref_axis',(0.,1.,0.));
#20938=DIRECTION('center_axis',(1.,0.,0.));
#20939=DIRECTION('ref_axis',(0.,0.,-1.));
#20940=DIRECTION('',(-0.707106781186552,-0.707106781186543,-8.65956056235488E-17));
#20941=DIRECTION('center_axis',(1.,0.,0.));
#20942=DIRECTION('ref_axis',(0.,0.,-1.));
#20943=DIRECTION('axis',(0.,0.,1.));
#20944=DIRECTION('refdir',(1.,0.,0.));
#20945=DIRECTION('center_axis',(0.,0.,1.));
#20946=DIRECTION('ref_axis',(1.,0.,0.));
#20947=DIRECTION('center_axis',(0.,0.,1.));
#20948=DIRECTION('ref_axis',(-1.,2.96059473233376E-15,0.));
#20949=DIRECTION('',(0.,-1.,0.));
#20950=DIRECTION('center_axis',(0.,0.,1.));
#20951=DIRECTION('ref_axis',(8.88178419700134E-15,1.,0.));
#20952=DIRECTION('',(-1.,0.,0.));
#20953=DIRECTION('center_axis',(0.,0.,1.));
#20954=DIRECTION('ref_axis',(1.,-5.92118946466753E-15,0.));
#20955=DIRECTION('',(0.,1.,0.));
#20956=DIRECTION('center_axis',(0.,0.,1.));
#20957=DIRECTION('ref_axis',(1.48029736616687E-15,-1.,0.));
#20958=DIRECTION('',(1.,0.,0.));
#20959=DIRECTION('center_axis',(0.,0.,1.));
#20960=DIRECTION('ref_axis',(1.,0.,0.));
#20961=DIRECTION('center_axis',(-1.,0.,0.));
#20962=DIRECTION('ref_axis',(0.,-1.,0.));
#20963=DIRECTION('',(0.,0.,1.));
#20964=DIRECTION('',(0.,-1.,0.));
#20965=DIRECTION('',(0.,0.,1.));
#20966=DIRECTION('center_axis',(0.,0.,1.));
#20967=DIRECTION('ref_axis',(8.88178419700134E-15,1.,0.));
#20968=DIRECTION('center_axis',(0.,0.,1.));
#20969=DIRECTION('ref_axis',(8.88178419700134E-15,1.,0.));
#20970=DIRECTION('',(0.,0.,1.));
#20971=DIRECTION('center_axis',(0.,1.,0.));
#20972=DIRECTION('ref_axis',(-1.,0.,0.));
#20973=DIRECTION('',(-1.,0.,0.));
#20974=DIRECTION('',(0.,0.,1.));
#20975=DIRECTION('center_axis',(0.,0.,1.));
#20976=DIRECTION('ref_axis',(1.,-5.92118946466753E-15,0.));
#20977=DIRECTION('center_axis',(0.,0.,1.));
#20978=DIRECTION('ref_axis',(1.,-5.92118946466753E-15,0.));
#20979=DIRECTION('',(0.,0.,1.));
#20980=DIRECTION('center_axis',(1.,0.,0.));
#20981=DIRECTION('ref_axis',(0.,1.,0.));
#20982=DIRECTION('',(0.,1.,0.));
#20983=DIRECTION('',(0.,0.,1.));
#20984=DIRECTION('center_axis',(0.,0.,1.));
#20985=DIRECTION('ref_axis',(1.48029736616687E-15,-1.,0.));
#20986=DIRECTION('center_axis',(0.,0.,1.));
#20987=DIRECTION('ref_axis',(1.48029736616687E-15,-1.,0.));
#20988=DIRECTION('',(0.,0.,1.));
#20989=DIRECTION('center_axis',(0.,-1.,0.));
#20990=DIRECTION('ref_axis',(1.,0.,0.));
#20991=DIRECTION('',(1.,0.,0.));
#20992=DIRECTION('',(0.,0.,1.));
#20993=DIRECTION('center_axis',(0.,0.,1.));
#20994=DIRECTION('ref_axis',(-1.,2.96059473233376E-15,0.));
#20995=DIRECTION('center_axis',(0.,0.,1.));
#20996=DIRECTION('ref_axis',(-1.,2.96059473233376E-15,0.));
#20997=DIRECTION('center_axis',(0.,0.,1.));
#20998=DIRECTION('ref_axis',(1.,0.,0.));
#20999=DIRECTION('center_axis',(0.,0.,1.));
#21000=DIRECTION('ref_axis',(1.,0.,0.));
#21001=DIRECTION('',(0.,0.,-1.));
#21002=DIRECTION('center_axis',(0.5,0.,-0.866025403784438));
#21003=DIRECTION('ref_axis',(0.866025403784438,0.,0.5));
#21004=DIRECTION('center_axis',(-0.5,0.,-0.866025403784438));
#21005=DIRECTION('ref_axis',(0.866025403784438,0.,-0.500000000000001));
#21006=DIRECTION('center_axis',(0.5,0.,-0.866025403784438));
#21007=DIRECTION('ref_axis',(0.866025403784438,0.,0.5));
#21008=DIRECTION('center_axis',(0.5,0.,0.866025403784438));
#21009=DIRECTION('ref_axis',(-0.866025403784438,0.,0.5));
#21010=DIRECTION('',(0.,-1.,0.));
#21011=DIRECTION('',(-0.866025403784438,0.,0.5));
#21012=DIRECTION('',(-0.866025403784438,0.,0.5));
#21013=DIRECTION('',(-0.866025403784438,0.,0.5));
#21014=DIRECTION('',(0.,-1.,0.));
#21015=DIRECTION('',(-0.866025403784438,0.,0.5));
#21016=DIRECTION('',(0.,-1.,0.));
#21017=DIRECTION('center_axis',(0.,1.,0.));
#21018=DIRECTION('ref_axis',(0.,0.,1.));
#21019=DIRECTION('center_axis',(0.,-1.,0.));
#21020=DIRECTION('ref_axis',(1.,0.,0.));
#21021=DIRECTION('center_axis',(0.,-1.,0.));
#21022=DIRECTION('ref_axis',(1.,0.,0.));
#21023=DIRECTION('',(0.,-1.,0.));
#21024=DIRECTION('center_axis',(0.,1.,0.));
#21025=DIRECTION('ref_axis',(1.,0.,0.));
#21026=DIRECTION('center_axis',(0.,1.,0.));
#21027=DIRECTION('ref_axis',(0.,0.,1.));
#21028=DIRECTION('',(0.866025403784439,0.,0.5));
#21029=DIRECTION('center_axis',(0.,-1.,0.));
#21030=DIRECTION('ref_axis',(1.,0.,0.));
#21031=DIRECTION('center_axis',(0.,1.,0.));
#21032=DIRECTION('ref_axis',(0.,0.,1.));
#21033=DIRECTION('',(0.866025403784439,0.,-0.5));
#21034=DIRECTION('center_axis',(0.,-1.,0.));
#21035=DIRECTION('ref_axis',(1.,0.,0.));
#21036=DIRECTION('center_axis',(0.,1.,0.));
#21037=DIRECTION('ref_axis',(0.,0.,1.));
#21038=DIRECTION('',(3.39346356420629E-16,0.,1.));
#21039=DIRECTION('center_axis',(0.,-1.,0.));
#21040=DIRECTION('ref_axis',(1.,0.,0.));
#21041=DIRECTION('center_axis',(0.,1.,0.));
#21042=DIRECTION('ref_axis',(0.,0.,1.));
#21043=DIRECTION('',(0.,0.,-1.));
#21044=DIRECTION('center_axis',(0.,-1.,0.));
#21045=DIRECTION('ref_axis',(1.,0.,0.));
#21046=DIRECTION('center_axis',(0.,-1.,0.));
#21047=DIRECTION('ref_axis',(1.,0.,0.));
#21048=DIRECTION('center_axis',(0.,1.,0.));
#21049=DIRECTION('ref_axis',(0.,0.,1.));
#21050=DIRECTION('center_axis',(0.,-1.,0.));
#21051=DIRECTION('ref_axis',(1.,0.,0.));
#21052=DIRECTION('center_axis',(0.,1.,0.));
#21053=DIRECTION('ref_axis',(0.,0.,1.));
#21054=DIRECTION('',(-0.866025403784438,0.,-0.5));
#21055=DIRECTION('center_axis',(0.,-1.,0.));
#21056=DIRECTION('ref_axis',(1.,0.,0.));
#21057=DIRECTION('center_axis',(0.,-1.,0.));
#21058=DIRECTION('ref_axis',(1.,0.,0.));
#21059=DIRECTION('center_axis',(0.,-1.,0.));
#21060=DIRECTION('ref_axis',(1.,0.,0.));
#21061=DIRECTION('',(0.,1.,0.));
#21062=DIRECTION('center_axis',(0.,1.,0.));
#21063=DIRECTION('ref_axis',(1.,0.,0.));
#21064=DIRECTION('center_axis',(0.,1.,0.));
#21065=DIRECTION('ref_axis',(1.,0.,0.));
#21066=DIRECTION('center_axis',(0.,1.,0.));
#21067=DIRECTION('ref_axis',(1.,0.,0.));
#21068=DIRECTION('center_axis',(0.,1.,0.));
#21069=DIRECTION('ref_axis',(1.,0.,0.));
#21070=DIRECTION('center_axis',(0.,1.,0.));
#21071=DIRECTION('ref_axis',(1.,0.,0.));
#21072=DIRECTION('center_axis',(0.,1.,0.));
#21073=DIRECTION('ref_axis',(1.,0.,0.));
#21074=DIRECTION('center_axis',(0.,1.,0.));
#21075=DIRECTION('ref_axis',(1.,0.,0.));
#21076=DIRECTION('center_axis',(0.,-1.,0.));
#21077=DIRECTION('ref_axis',(1.,0.,0.));
#21078=DIRECTION('',(-0.707106781186549,0.707106781186546,-8.65956056235495E-17));
#21079=DIRECTION('center_axis',(0.,-1.,0.));
#21080=DIRECTION('ref_axis',(0.,0.,-1.));
#21081=DIRECTION('center_axis',(0.,-1.,0.));
#21082=DIRECTION('ref_axis',(0.,0.,-1.));
#21083=DIRECTION('',(0.866025403784439,0.,0.5));
#21084=DIRECTION('',(3.39346356420629E-16,0.,1.));
#21085=DIRECTION('center_axis',(0.,-1.,0.));
#21086=DIRECTION('ref_axis',(0.,0.,-1.));
#21087=DIRECTION('',(3.39346356420629E-16,0.,1.));
#21088=DIRECTION('center_axis',(0.,-1.,0.));
#21089=DIRECTION('ref_axis',(0.,0.,-1.));
#21090=DIRECTION('',(0.866025403784439,0.,-0.5));
#21091=DIRECTION('',(0.866025403784439,0.,0.5));
#21092=DIRECTION('center_axis',(0.,-1.,0.));
#21093=DIRECTION('ref_axis',(0.,0.,-1.));
#21094=DIRECTION('',(-0.866025403784438,0.,-0.5));
#21095=DIRECTION('center_axis',(0.,-1.,0.));
#21096=DIRECTION('ref_axis',(0.,0.,-1.));
#21097=DIRECTION('',(0.,0.,-1.));
#21098=DIRECTION('',(0.866025403784439,0.,-0.5));
#21099=DIRECTION('center_axis',(0.,1.,0.));
#21100=DIRECTION('ref_axis',(1.,0.,0.));
#21101=DIRECTION('',(0.866025403784439,0.,0.5));
#21102=DIRECTION('',(0.866025403784439,0.,-0.5));
#21103=DIRECTION('',(0.,0.,-1.));
#21104=DIRECTION('',(-0.866025403784438,0.,-0.5));
#21105=DIRECTION('',(3.39346356420629E-16,0.,1.));
#21106=DIRECTION('center_axis',(0.,-1.,0.));
#21107=DIRECTION('ref_axis',(1.,0.,0.));
#21108=DIRECTION('center_axis',(-0.5,0.,-0.866025403784439));
#21109=DIRECTION('ref_axis',(0.866025403784439,0.,-0.5));
#21110=DIRECTION('',(0.,-1.,0.));
#21111=DIRECTION('',(0.,-1.,0.));
#21112=DIRECTION('center_axis',(-1.,0.,0.));
#21113=DIRECTION('ref_axis',(0.,0.,-1.));
#21114=DIRECTION('',(0.,0.,-1.));
#21115=DIRECTION('',(0.,-1.,0.));
#21116=DIRECTION('center_axis',(-0.5,0.,0.866025403784438));
#21117=DIRECTION('ref_axis',(-0.866025403784438,0.,-0.5));
#21118=DIRECTION('',(-0.866025403784438,0.,-0.5));
#21119=DIRECTION('center_axis',(1.,0.,-3.39346356420629E-16));
#21120=DIRECTION('ref_axis',(3.39346356420629E-16,0.,1.));
#21121=DIRECTION('',(0.,-1.,0.));
#21122=DIRECTION('center_axis',(0.5,0.,-0.866025403784439));
#21123=DIRECTION('ref_axis',(0.866025403784439,0.,0.5));
#21124=DIRECTION('center_axis',(0.,-1.,0.));
#21125=DIRECTION('ref_axis',(0.,0.,-1.));
#21126=DIRECTION('center_axis',(0.,1.,0.));
#21127=DIRECTION('ref_axis',(0.,0.,1.));
#21128=DIRECTION('center_axis',(0.,-1.,0.));
#21129=DIRECTION('ref_axis',(1.,0.,0.));
#21130=DIRECTION('center_axis',(0.,-1.,0.));
#21131=DIRECTION('ref_axis',(1.,0.,0.));
#21132=DIRECTION('center_axis',(0.,-1.,0.));
#21133=DIRECTION('ref_axis',(1.,0.,0.));
#21134=DIRECTION('',(0.514495755427528,0.857492925712543,6.30075580059222E-17));
#21135=DIRECTION('center_axis',(0.,-1.,0.));
#21136=DIRECTION('ref_axis',(1.,0.,0.));
#21137=DIRECTION('',(0.,1.,0.));
#21138=DIRECTION('axis',(0.,0.,1.));
#21139=DIRECTION('refdir',(1.,0.,0.));
#21140=DIRECTION('center_axis',(2.1030317852139E-15,-0.547750005235842,
0.836642057133238));
#21141=DIRECTION('ref_axis',(1.,0.,-2.51365774321693E-15));
#21142=DIRECTION('',(1.,0.,-2.56395024851142E-15));
#21143=DIRECTION('',(-0.586730430533741,0.677497944020818,0.443558268701256));
#21144=DIRECTION('',(-0.58673043053375,-0.677497944020814,-0.443558268701251));
#21145=DIRECTION('center_axis',(-0.724553275351853,-0.547750005235845,0.418321028566619));
#21146=DIRECTION('ref_axis',(0.500000000000001,0.,0.866025403784438));
#21147=DIRECTION('',(0.500000000000001,0.,0.866025403784438));
#21148=DIRECTION('',(-0.677497944020805,0.677497944020814,-0.286344323664975));
#21149=DIRECTION('',(0.0907675134870613,-0.677497944020816,-0.72990259236623));
#21150=DIRECTION('center_axis',(0.724553275351854,-0.547750005235844,0.418321028566617));
#21151=DIRECTION('ref_axis',(0.499999999999999,0.,-0.866025403784439));
#21152=DIRECTION('',(0.500000000000003,0.,-0.866025403784437));
#21153=DIRECTION('',(0.0907675134870613,0.677497944020816,0.72990259236623));
#21154=DIRECTION('',(-0.677497944020804,-0.677497944020816,0.286344323664975));
#21155=DIRECTION('center_axis',(0.353553390593277,-0.707106781186542,0.612372435695799));
#21156=DIRECTION('ref_axis',(0.866025403784439,0.,-0.5));
#21157=DIRECTION('',(0.866025403784439,0.,-0.5));
#21158=DIRECTION('',(-0.866025403784439,0.,0.5));
#21159=DIRECTION('center_axis',(-0.724553275351849,-0.547750005235848,-0.418321028566621));
#21160=DIRECTION('ref_axis',(-0.500000000000005,0.,0.866025403784436));
#21161=DIRECTION('',(-0.500000000000002,0.,0.866025403784437));
#21162=DIRECTION('',(-0.0907675134870579,0.677497944020813,-0.729902592366233));
#21163=DIRECTION('',(0.677497944020807,-0.677497944020816,-0.286344323664964));
#21164=DIRECTION('center_axis',(0.724553275351851,-0.547750005235849,-0.418321028566616));
#21165=DIRECTION('ref_axis',(-0.499999999999999,0.,-0.866025403784439));
#21166=DIRECTION('',(0.677497944020806,0.677497944020818,0.286344323664964));
#21167=DIRECTION('',(-0.0907675134870605,-0.67749794402081,0.729902592366236));
#21168=DIRECTION('',(-0.499999999999999,0.,-0.866025403784439));
#21169=DIRECTION('center_axis',(0.,-0.547750005235853,-0.83664205713323));
#21170=DIRECTION('ref_axis',(-1.,0.,0.));
#21171=DIRECTION('',(-1.,0.,0.));
#21172=DIRECTION('',(0.586730430533742,0.677497944020812,-0.443558268701264));
#21173=DIRECTION('',(0.58673043053374,-0.677497944020813,0.443558268701265));
#21174=DIRECTION('center_axis',(0.353553390593275,-0.707106781186545,-0.612372435695797));
#21175=DIRECTION('ref_axis',(-0.866025403784439,0.,-0.499999999999999));
#21176=DIRECTION('',(-0.866025403784439,0.,-0.499999999999999));
#21177=DIRECTION('',(0.866025403784439,0.,0.499999999999999));
#21178=DIRECTION('center_axis',(-0.353553390593275,-0.707106781186544,-0.612372435695797));
#21179=DIRECTION('ref_axis',(-0.866025403784439,0.,0.5));
#21180=DIRECTION('',(-0.866025403784439,0.,0.5));
#21181=DIRECTION('',(0.866025403784439,0.,-0.5));
#21182=DIRECTION('center_axis',(0.,0.,-1.));
#21183=DIRECTION('ref_axis',(-1.,0.,0.));
#21184=DIRECTION('',(-1.,0.,0.));
#21185=DIRECTION('',(0.,-1.,0.));
#21186=DIRECTION('',(0.,1.,0.));
#21187=DIRECTION('center_axis',(0.866025403784439,0.,-0.499999999999999));
#21188=DIRECTION('ref_axis',(-0.499999999999999,0.,-0.866025403784439));
#21189=DIRECTION('',(-0.499999999999999,0.,-0.866025403784439));
#21190=DIRECTION('',(0.,-1.,0.));
#21191=DIRECTION('',(0.,1.,0.));
#21192=DIRECTION('center_axis',(0.707106781186554,-0.707106781186541,0.));
#21193=DIRECTION('ref_axis',(0.,0.,-1.));
#21194=DIRECTION('',(0.,0.,-1.));
#21195=DIRECTION('',(0.,0.,1.));
#21196=DIRECTION('center_axis',(-0.707106781186552,-0.707106781186543,-1.43130521632687E-16));
#21197=DIRECTION('ref_axis',(-2.0241712488248E-16,0.,1.));
#21198=DIRECTION('',(-2.0241712488248E-16,0.,1.));
#21199=DIRECTION('',(2.0241712488248E-16,0.,-1.));
#21200=DIRECTION('center_axis',(-0.866025403784437,0.,-0.500000000000002));
#21201=DIRECTION('ref_axis',(-0.500000000000002,0.,0.866025403784437));
#21202=DIRECTION('',(-0.500000000000002,0.,0.866025403784437));
#21203=DIRECTION('',(0.,-1.,0.));
#21204=DIRECTION('',(0.,1.,0.));
#21205=DIRECTION('center_axis',(0.866025403784437,0.,0.500000000000003));
#21206=DIRECTION('ref_axis',(0.500000000000003,0.,-0.866025403784437));
#21207=DIRECTION('',(0.500000000000003,0.,-0.866025403784437));
#21208=DIRECTION('',(0.,-1.,0.));
#21209=DIRECTION('',(0.,1.,0.));
#21210=DIRECTION('center_axis',(-0.353553390593277,-0.70710678118654,0.612372435695801));
#21211=DIRECTION('ref_axis',(0.866025403784439,0.,0.5));
#21212=DIRECTION('',(0.866025403784439,0.,0.5));
#21213=DIRECTION('',(-0.866025403784439,0.,-0.5));
#21214=DIRECTION('center_axis',(-0.866025403784438,0.,0.500000000000001));
#21215=DIRECTION('ref_axis',(0.500000000000001,0.,0.866025403784438));
#21216=DIRECTION('',(0.500000000000001,0.,0.866025403784438));
#21217=DIRECTION('',(0.,-1.,0.));
#21218=DIRECTION('',(0.,1.,0.));
#21219=DIRECTION('center_axis',(2.56395024851142E-15,0.,1.));
#21220=DIRECTION('ref_axis',(1.,0.,-2.56395024851142E-15));
#21221=DIRECTION('',(1.,0.,-2.56395024851142E-15));
#21222=DIRECTION('',(0.,-1.,0.));
#21223=DIRECTION('',(0.,1.,0.));
#21224=DIRECTION('center_axis',(-0.5,0.,-0.866025403784439));
#21225=DIRECTION('ref_axis',(-0.866025403784439,0.,0.5));
#21226=DIRECTION('',(-0.866025403784439,0.,0.5));
#21227=DIRECTION('center_axis',(-1.,0.,-2.0241712488248E-16));
#21228=DIRECTION('ref_axis',(-2.0241712488248E-16,0.,1.));
#21229=DIRECTION('',(-2.0241712488248E-16,0.,1.));
#21230=DIRECTION('center_axis',(-0.5,0.,0.866025403784439));
#21231=DIRECTION('ref_axis',(0.866025403784439,0.,0.5));
#21232=DIRECTION('',(0.866025403784439,0.,0.5));
#21233=DIRECTION('center_axis',(0.,1.,0.));
#21234=DIRECTION('ref_axis',(1.,0.,0.));
#21235=DIRECTION('center_axis',(0.,-1.,0.));
#21236=DIRECTION('ref_axis',(1.,0.,0.));
#21237=DIRECTION('center_axis',(0.,-1.,0.));
#21238=DIRECTION('ref_axis',(-1.,0.,0.));
#21239=DIRECTION('center_axis',(0.,1.,0.));
#21240=DIRECTION('ref_axis',(-1.,0.,0.));
#21241=DIRECTION('center_axis',(0.,1.,0.));
#21242=DIRECTION('ref_axis',(-1.,0.,0.));
#21243=DIRECTION('',(-0.382683432365081,0.923879532511291,-4.68652040532618E-17));
#21244=DIRECTION('center_axis',(0.,-1.,0.));
#21245=DIRECTION('ref_axis',(-1.,0.,0.));
#21246=DIRECTION('center_axis',(0.,-1.,0.));
#21247=DIRECTION('ref_axis',(-1.,0.,0.));
#21248=DIRECTION('center_axis',(0.,-1.,0.));
#21249=DIRECTION('ref_axis',(1.,0.,0.));
#21250=DIRECTION('',(0.707106781186546,0.707106781186549,8.65956056235492E-17));
#21251=DIRECTION('center_axis',(0.,1.,0.));
#21252=DIRECTION('ref_axis',(-1.,0.,0.));
#21253=DIRECTION('center_axis',(0.,1.,0.));
#21254=DIRECTION('ref_axis',(-1.,0.,0.));
#21255=DIRECTION('center_axis',(0.,-1.,0.));
#21256=DIRECTION('ref_axis',(1.,0.,0.));
#21257=DIRECTION('center_axis',(0.,1.,0.));
#21258=DIRECTION('ref_axis',(1.,0.,0.));
#21259=DIRECTION('',(0.,1.,0.));
#21260=DIRECTION('center_axis',(0.,-1.,0.));
#21261=DIRECTION('ref_axis',(-1.,0.,0.));
#21262=DIRECTION('',(-0.923879532511288,0.382683432365086,-1.1314261122877E-16));
#21263=DIRECTION('center_axis',(0.,-1.,0.));
#21264=DIRECTION('ref_axis',(-1.,0.,0.));
#21265=DIRECTION('center_axis',(0.,1.,0.));
#21266=DIRECTION('ref_axis',(0.,0.,1.));
#21267=DIRECTION('center_axis',(0.,1.,0.));
#21268=DIRECTION('ref_axis',(-1.,0.,0.));
#21269=DIRECTION('center_axis',(0.,1.,0.));
#21270=DIRECTION('ref_axis',(-1.,0.,0.));
#21271=DIRECTION('',(0.707106781186549,0.707106781186546,8.65956056235495E-17));
#21272=DIRECTION('center_axis',(0.,-1.,0.));
#21273=DIRECTION('ref_axis',(-1.,0.,0.));
#21274=DIRECTION('center_axis',(0.,-1.,0.));
#21275=DIRECTION('ref_axis',(-1.,0.,0.));
#21276=DIRECTION('center_axis',(0.,-1.,0.));
#21277=DIRECTION('ref_axis',(1.,0.,0.));
#21278=DIRECTION('',(0.,1.,0.));
#21279=DIRECTION('center_axis',(0.,-1.,0.));
#21280=DIRECTION('ref_axis',(1.,0.,0.));
#21281=DIRECTION('center_axis',(0.,-1.,0.));
#21282=DIRECTION('ref_axis',(0.,0.,-1.));
#21283=DIRECTION('',(0.,0.,-1.));
#21284=DIRECTION('',(-0.866025403784439,0.,-0.499999999999999));
#21285=DIRECTION('',(0.866025403784439,0.,-0.5));
#21286=DIRECTION('center_axis',(0.,1.,0.));
#21287=DIRECTION('ref_axis',(0.,0.,1.));
#21288=DIRECTION('center_axis',(0.,-1.,0.));
#21289=DIRECTION('ref_axis',(1.,0.,0.));
#21290=DIRECTION('center_axis',(0.,-1.,0.));
#21291=DIRECTION('ref_axis',(0.,0.,-1.));
#21292=DIRECTION('center_axis',(0.,-1.,0.));
#21293=DIRECTION('ref_axis',(1.,0.,0.));
#21294=DIRECTION('center_axis',(0.,-1.,0.));
#21295=DIRECTION('ref_axis',(1.,0.,0.));
#21296=DIRECTION('center_axis',(0.,-1.,0.));
#21297=DIRECTION('ref_axis',(1.,0.,0.));
#21298=DIRECTION('',(0.,-1.,0.));
#21299=DIRECTION('center_axis',(0.,-1.,0.));
#21300=DIRECTION('ref_axis',(1.,0.,0.));
#21301=DIRECTION('center_axis',(0.,1.,0.));
#21302=DIRECTION('ref_axis',(1.,0.,0.));
#21303=DIRECTION('',(0.,1.,0.));
#21304=DIRECTION('center_axis',(0.,1.,0.));
#21305=DIRECTION('ref_axis',(0.,0.,1.));
#21306=DIRECTION('center_axis',(0.,-1.,0.));
#21307=DIRECTION('ref_axis',(1.,0.,0.));
#21308=DIRECTION('center_axis',(0.,-1.,0.));
#21309=DIRECTION('ref_axis',(0.,0.,-1.));
#21310=DIRECTION('center_axis',(0.,-1.,0.));
#21311=DIRECTION('ref_axis',(1.,0.,0.));
#21312=DIRECTION('center_axis',(0.,-1.,0.));
#21313=DIRECTION('ref_axis',(1.,0.,0.));
#21314=DIRECTION('',(0.,-1.,0.));
#21315=DIRECTION('center_axis',(1.,0.,0.));
#21316=DIRECTION('ref_axis',(0.,0.,-1.));
#21317=DIRECTION('center_axis',(0.5,0.,0.866025403784439));
#21318=DIRECTION('ref_axis',(0.866025403784439,0.,-0.5));
#21319=DIRECTION('center_axis',(0.5,0.,-0.866025403784439));
#21320=DIRECTION('ref_axis',(-0.866025403784439,0.,-0.499999999999999));
#21321=DIRECTION('center_axis',(0.,-1.,0.));
#21322=DIRECTION('ref_axis',(1.,0.,0.));
#21323=DIRECTION('center_axis',(0.,-1.,0.));
#21324=DIRECTION('ref_axis',(1.,0.,0.));
#21325=DIRECTION('',(0.,1.,0.));
#21326=DIRECTION('center_axis',(0.,1.,0.));
#21327=DIRECTION('ref_axis',(1.,0.,0.));
#21328=DIRECTION('center_axis',(0.,-1.,0.));
#21329=DIRECTION('ref_axis',(1.,0.,0.));
#21330=DIRECTION('',(-0.514495755427524,0.857492925712546,-6.30075580059217E-17));
#21331=DIRECTION('center_axis',(0.,-1.,0.));
#21332=DIRECTION('ref_axis',(0.,0.,-1.));
#21333=DIRECTION('axis',(0.,0.,1.));
#21334=DIRECTION('refdir',(1.,0.,0.));
#21335=DIRECTION('center_axis',(6.12323399573677E-17,0.,1.));
#21336=DIRECTION('ref_axis',(1.,0.,0.));
#21337=DIRECTION('center_axis',(1.22464679914735E-16,-1.,0.));
#21338=DIRECTION('ref_axis',(-1.,-1.22464679914735E-16,0.));
#21339=DIRECTION('axis',(0.,0.,1.));
#21340=DIRECTION('refdir',(1.,0.,0.));
#21341=DIRECTION('center_axis',(1.,0.,0.));
#21342=DIRECTION('ref_axis',(0.,1.,0.));
#21343=DIRECTION('center_axis',(1.,0.,0.));
#21344=DIRECTION('ref_axis',(0.,0.,-1.));
#21345=DIRECTION('',(-1.,0.,0.));
#21346=DIRECTION('center_axis',(1.,0.,0.));
#21347=DIRECTION('ref_axis',(0.,0.,-1.));
#21348=DIRECTION('center_axis',(-1.,0.,0.));
#21349=DIRECTION('ref_axis',(0.,0.,1.));
#21350=DIRECTION('center_axis',(1.,0.,0.));
#21351=DIRECTION('ref_axis',(0.,0.,-1.));
#21352=DIRECTION('center_axis',(1.,0.,0.));
#21353=DIRECTION('ref_axis',(0.,1.,0.));
#21354=DIRECTION('center_axis',(1.,0.,0.));
#21355=DIRECTION('ref_axis',(0.,0.,-1.));
#21356=DIRECTION('',(-0.707106781186547,0.707106781186548,8.65956056235494E-17));
#21357=DIRECTION('center_axis',(1.,0.,0.));
#21358=DIRECTION('ref_axis',(0.,1.,0.));
#21359=DIRECTION('center_axis',(1.,0.,0.));
#21360=DIRECTION('ref_axis',(0.,0.,-1.));
#21361=DIRECTION('',(-1.,0.,0.));
#21362=DIRECTION('center_axis',(-1.,0.,0.));
#21363=DIRECTION('ref_axis',(0.,1.,0.));
#21364=DIRECTION('center_axis',(1.,0.,0.));
#21365=DIRECTION('ref_axis',(0.,0.,-1.));
#21366=DIRECTION('',(-0.707106781186547,-0.707106781186548,-8.65956056235494E-17));
#21367=DIRECTION('center_axis',(1.,0.,0.));
#21368=DIRECTION('ref_axis',(0.,0.,-1.));
#21369=DIRECTION('axis',(0.,0.,1.));
#21370=DIRECTION('refdir',(1.,0.,0.));
#21371=DIRECTION('center_axis',(0.,0.,-1.));
#21372=DIRECTION('ref_axis',(1.,0.,0.));
#21373=DIRECTION('center_axis',(0.,0.,-1.));
#21374=DIRECTION('ref_axis',(1.,0.,0.));
#21375=DIRECTION('',(0.707106781186546,-8.65956056235491E-17,0.707106781186549));
#21376=DIRECTION('center_axis',(0.,0.,1.));
#21377=DIRECTION('ref_axis',(1.,0.,0.));
#21378=DIRECTION('center_axis',(0.,0.,-1.));
#21379=DIRECTION('ref_axis',(-1.,0.,0.));
#21380=DIRECTION('',(1.,0.,0.));
#21381=DIRECTION('',(0.,-1.,0.));
#21382=DIRECTION('',(-1.,0.,0.));
#21383=DIRECTION('',(0.,1.,0.));
#21384=DIRECTION('center_axis',(0.,0.,-1.));
#21385=DIRECTION('ref_axis',(1.,0.,0.));
#21386=DIRECTION('center_axis',(0.,0.,1.));
#21387=DIRECTION('ref_axis',(1.,0.,0.));
#21388=DIRECTION('center_axis',(0.,0.,1.));
#21389=DIRECTION('ref_axis',(1.,0.,0.));
#21390=DIRECTION('center_axis',(0.,0.,1.));
#21391=DIRECTION('ref_axis',(1.,0.,0.));
#21392=DIRECTION('center_axis',(0.,0.,1.));
#21393=DIRECTION('ref_axis',(1.,0.,0.));
#21394=DIRECTION('center_axis',(0.,0.,-1.));
#21395=DIRECTION('ref_axis',(1.,0.,0.));
#21396=DIRECTION('center_axis',(0.,0.,-1.));
#21397=DIRECTION('ref_axis',(1.,0.,0.));
#21398=DIRECTION('',(0.,0.,-1.));
#21399=DIRECTION('center_axis',(0.,0.,-1.));
#21400=DIRECTION('ref_axis',(1.,0.,0.));
#21401=DIRECTION('',(0.707106781186546,-8.65956056235491E-17,0.707106781186549));
#21402=DIRECTION('center_axis',(0.,0.,1.));
#21403=DIRECTION('ref_axis',(1.,0.,0.));
#21404=DIRECTION('center_axis',(0.,0.,-1.));
#21405=DIRECTION('ref_axis',(1.,0.,0.));
#21406=DIRECTION('center_axis',(0.,0.,-1.));
#21407=DIRECTION('ref_axis',(1.,0.,0.));
#21408=DIRECTION('',(0.,0.,-1.));
#21409=DIRECTION('center_axis',(0.,-0.707106781186541,0.707106781186554));
#21410=DIRECTION('ref_axis',(1.,0.,0.));
#21411=DIRECTION('',(0.,-0.707106781186554,-0.707106781186541));
#21412=DIRECTION('',(1.,0.,0.));
#21413=DIRECTION('',(0.,0.707106781186554,0.707106781186541));
#21414=DIRECTION('',(-1.,0.,0.));
#21415=DIRECTION('center_axis',(0.,1.,0.));
#21416=DIRECTION('ref_axis',(-0.707106781186548,0.,0.707106781186548));
#21417=DIRECTION('center_axis',(0.,-1.,0.));
#21418=DIRECTION('ref_axis',(-0.707106781186548,0.,0.707106781186548));
#21419=DIRECTION('',(0.707106781186551,-0.707106781186544,0.));
#21420=DIRECTION('center_axis',(0.,1.,0.));
#21421=DIRECTION('ref_axis',(-0.707106781186547,0.,0.707106781186547));
#21422=DIRECTION('center_axis',(-0.707106781186554,-0.707106781186541,0.));
#21423=DIRECTION('ref_axis',(0.,0.,1.));
#21424=DIRECTION('',(0.707106781186541,-0.707106781186554,0.));
#21425=DIRECTION('',(0.,0.,1.));
#21426=DIRECTION('',(0.,0.,-1.));
#21427=DIRECTION('center_axis',(0.,1.,0.));
#21428=DIRECTION('ref_axis',(-0.707106781186548,0.,-0.707106781186548));
#21429=DIRECTION('center_axis',(0.,-1.,0.));
#21430=DIRECTION('ref_axis',(-0.707106781186548,0.,-0.707106781186548));
#21431=DIRECTION('',(0.,-0.707106781186547,0.707106781186548));
#21432=DIRECTION('center_axis',(0.,1.,0.));
#21433=DIRECTION('ref_axis',(-0.707106781186547,0.,-0.707106781186547));
#21434=DIRECTION('center_axis',(0.,-0.707106781186543,-0.707106781186552));
#21435=DIRECTION('ref_axis',(-1.,0.,0.));
#21436=DIRECTION('',(0.,-0.707106781186552,0.707106781186543));
#21437=DIRECTION('',(-1.,0.,0.));
#21438=DIRECTION('',(1.,0.,0.));
#21439=DIRECTION('center_axis',(0.,1.,0.));
#21440=DIRECTION('ref_axis',(0.707106781186548,0.,-0.707106781186548));
#21441=DIRECTION('center_axis',(0.,-1.,0.));
#21442=DIRECTION('ref_axis',(0.707106781186548,0.,-0.707106781186548));
#21443=DIRECTION('',(-0.707106781186554,-0.707106781186541,0.));
#21444=DIRECTION('center_axis',(0.,1.,0.));
#21445=DIRECTION('ref_axis',(0.707106781186547,0.,-0.707106781186547));
#21446=DIRECTION('center_axis',(0.707106781186554,-0.707106781186541,0.));
#21447=DIRECTION('ref_axis',(0.,0.,-1.));
#21448=DIRECTION('',(-0.707106781186541,-0.707106781186554,0.));
#21449=DIRECTION('',(0.,0.,-1.));
#21450=DIRECTION('',(0.,0.,1.));
#21451=DIRECTION('center_axis',(0.,-1.,0.));
#21452=DIRECTION('ref_axis',(-0.707106781186548,0.,0.707106781186548));
#21453=DIRECTION('center_axis',(0.,1.,0.));
#21454=DIRECTION('ref_axis',(-0.707106781186548,0.,0.707106781186548));
#21455=DIRECTION('',(0.,-0.707106781186546,0.707106781186549));
#21456=DIRECTION('center_axis',(0.,-1.,0.));
#21457=DIRECTION('ref_axis',(-0.707106781186547,0.,0.707106781186547));
#21458=DIRECTION('center_axis',(0.,-0.707106781186543,-0.707106781186552));
#21459=DIRECTION('ref_axis',(-1.,0.,0.));
#21460=DIRECTION('',(0.,-0.707106781186552,0.707106781186543));
#21461=DIRECTION('',(-1.,0.,0.));
#21462=DIRECTION('center_axis',(0.,-1.,0.));
#21463=DIRECTION('ref_axis',(0.707106781186548,0.,0.707106781186548));
#21464=DIRECTION('center_axis',(0.,1.,0.));
#21465=DIRECTION('ref_axis',(0.707106781186548,0.,0.707106781186548));
#21466=DIRECTION('',(0.707106781186554,-0.707106781186541,0.));
#21467=DIRECTION('center_axis',(0.,-1.,0.));
#21468=DIRECTION('ref_axis',(0.707106781186547,0.,0.707106781186547));
#21469=DIRECTION('center_axis',(-0.707106781186548,-0.707106781186548,0.));
#21470=DIRECTION('ref_axis',(0.,0.,1.));
#21471=DIRECTION('',(0.707106781186547,-0.707106781186547,0.));
#21472=DIRECTION('',(0.,0.,1.));
#21473=DIRECTION('',(0.,0.,-1.));
#21474=DIRECTION('center_axis',(0.,1.,0.));
#21475=DIRECTION('ref_axis',(-0.707106781186555,0.,-0.70710678118654));
#21476=DIRECTION('center_axis',(0.,-1.,0.));
#21477=DIRECTION('ref_axis',(-0.707106781186555,0.,-0.70710678118654));
#21478=DIRECTION('',(0.,-0.707106781186547,0.707106781186548));
#21479=DIRECTION('center_axis',(0.,1.,0.));
#21480=DIRECTION('ref_axis',(-0.707106781186555,0.,-0.70710678118654));
#21481=DIRECTION('center_axis',(0.,-0.707106781186543,-0.707106781186552));
#21482=DIRECTION('ref_axis',(-1.,0.,0.));
#21483=DIRECTION('',(0.,-0.707106781186552,0.707106781186543));
#21484=DIRECTION('',(-1.,0.,0.));
#21485=DIRECTION('',(1.,0.,0.));
#21486=DIRECTION('center_axis',(0.,1.,0.));
#21487=DIRECTION('ref_axis',(0.70710678118654,0.,-0.707106781186555));
#21488=DIRECTION('center_axis',(0.,-1.,0.));
#21489=DIRECTION('ref_axis',(0.70710678118654,0.,-0.707106781186555));
#21490=DIRECTION('',(-0.707106781186529,-0.707106781186566,0.));
#21491=DIRECTION('center_axis',(0.,1.,0.));
#21492=DIRECTION('ref_axis',(0.70710678118654,0.,-0.707106781186555));
#21493=DIRECTION('center_axis',(0.707106781186548,-0.707106781186548,0.));
#21494=DIRECTION('ref_axis',(0.,0.,-1.));
#21495=DIRECTION('',(-0.707106781186547,-0.707106781186547,0.));
#21496=DIRECTION('',(0.,0.,-1.));
#21497=DIRECTION('',(0.,0.,1.));
#21498=DIRECTION('center_axis',(0.,1.,0.));
#21499=DIRECTION('ref_axis',(0.707106781186555,0.,0.70710678118654));
#21500=DIRECTION('center_axis',(0.,-1.,0.));
#21501=DIRECTION('ref_axis',(0.707106781186555,0.,0.70710678118654));
#21502=DIRECTION('center_axis',(0.,1.,0.));
#21503=DIRECTION('ref_axis',(0.707106781186555,0.,0.70710678118654));
#21504=DIRECTION('center_axis',(0.,1.,0.));
#21505=DIRECTION('ref_axis',(-0.707106781186548,0.,0.707106781186548));
#21506=DIRECTION('',(0.,1.,0.));
#21507=DIRECTION('center_axis',(0.,-1.,0.));
#21508=DIRECTION('ref_axis',(-0.707106781186548,0.,0.707106781186548));
#21509=DIRECTION('center_axis',(1.,0.,0.));
#21510=DIRECTION('ref_axis',(0.,0.,-1.));
#21511=DIRECTION('',(0.,-1.,0.));
#21512=DIRECTION('',(0.,0.,-1.));
#21513=DIRECTION('center_axis',(0.,1.,0.));
#21514=DIRECTION('ref_axis',(0.707106781186548,0.,-0.707106781186548));
#21515=DIRECTION('',(0.,1.,0.));
#21516=DIRECTION('center_axis',(0.,1.,0.));
#21517=DIRECTION('ref_axis',(0.707106781186548,0.,-0.707106781186548));
#21518=DIRECTION('center_axis',(0.,0.,-1.));
#21519=DIRECTION('ref_axis',(-1.,0.,0.));
#21520=DIRECTION('',(0.,-1.,0.));
#21521=DIRECTION('',(-1.,0.,0.));
#21522=DIRECTION('center_axis',(0.,1.,0.));
#21523=DIRECTION('ref_axis',(-0.707106781186548,0.,-0.707106781186548));
#21524=DIRECTION('',(0.,1.,0.));
#21525=DIRECTION('center_axis',(0.,1.,0.));
#21526=DIRECTION('ref_axis',(-0.707106781186548,0.,-0.707106781186548));
#21527=DIRECTION('center_axis',(-1.,0.,0.));
#21528=DIRECTION('ref_axis',(0.,0.,1.));
#21529=DIRECTION('',(0.,-1.,0.));
#21530=DIRECTION('',(0.,0.,1.));
#21531=DIRECTION('center_axis',(0.,1.,0.));
#21532=DIRECTION('ref_axis',(-0.707106781186548,0.,0.707106781186548));
#21533=DIRECTION('',(0.,1.,0.));
#21534=DIRECTION('center_axis',(0.,1.,0.));
#21535=DIRECTION('ref_axis',(-0.707106781186548,0.,0.707106781186548));
#21536=DIRECTION('center_axis',(0.,0.,1.));
#21537=DIRECTION('ref_axis',(1.,0.,0.));
#21538=DIRECTION('',(0.,-1.,0.));
#21539=DIRECTION('',(1.,0.,0.));
#21540=DIRECTION('center_axis',(0.,0.,1.));
#21541=DIRECTION('ref_axis',(1.,0.,0.));
#21542=DIRECTION('center_axis',(0.,0.,-1.));
#21543=DIRECTION('ref_axis',(1.,0.,0.));
#21544=DIRECTION('center_axis',(0.,0.,-1.));
#21545=DIRECTION('ref_axis',(1.,0.,0.));
#21546=DIRECTION('center_axis',(0.,0.,-1.));
#21547=DIRECTION('ref_axis',(1.,0.,0.));
#21548=DIRECTION('center_axis',(0.,0.,-1.));
#21549=DIRECTION('ref_axis',(1.,0.,0.));
#21550=DIRECTION('center_axis',(0.,0.,1.));
#21551=DIRECTION('ref_axis',(1.,0.,0.));
#21552=DIRECTION('center_axis',(0.,1.,0.));
#21553=DIRECTION('ref_axis',(1.,0.,0.));
#21554=DIRECTION('center_axis',(0.,0.707106781186541,0.707106781186554));
#21555=DIRECTION('ref_axis',(1.,0.,0.));
#21556=DIRECTION('',(0.,0.707106781186554,-0.707106781186541));
#21557=DIRECTION('',(-1.,0.,0.));
#21558=DIRECTION('',(0.,-0.707106781186554,0.707106781186541));
#21559=DIRECTION('center_axis',(0.,-1.,0.));
#21560=DIRECTION('ref_axis',(0.707106781186555,0.,0.70710678118654));
#21561=DIRECTION('center_axis',(0.,1.,0.));
#21562=DIRECTION('ref_axis',(0.707106781186555,0.,0.70710678118654));
#21563=DIRECTION('',(-0.707106781186535,0.70710678118656,0.));
#21564=DIRECTION('center_axis',(0.,-1.,0.));
#21565=DIRECTION('ref_axis',(0.707106781186555,0.,0.70710678118654));
#21566=DIRECTION('center_axis',(0.707106781186548,0.707106781186548,0.));
#21567=DIRECTION('ref_axis',(0.,0.,-1.));
#21568=DIRECTION('',(-0.707106781186547,0.707106781186547,0.));
#21569=DIRECTION('',(0.,0.,1.));
#21570=DIRECTION('',(0.,0.,-1.));
#21571=DIRECTION('center_axis',(0.,-1.,0.));
#21572=DIRECTION('ref_axis',(0.70710678118654,0.,-0.707106781186555));
#21573=DIRECTION('center_axis',(0.,1.,0.));
#21574=DIRECTION('ref_axis',(0.70710678118654,0.,-0.707106781186555));
#21575=DIRECTION('',(0.,0.707106781186553,0.707106781186542));
#21576=DIRECTION('center_axis',(0.,-1.,0.));
#21577=DIRECTION('ref_axis',(0.70710678118654,0.,-0.707106781186555));
#21578=DIRECTION('center_axis',(0.,0.707106781186543,-0.707106781186552));
#21579=DIRECTION('ref_axis',(-1.,0.,0.));
#21580=DIRECTION('',(0.,0.707106781186552,0.707106781186543));
#21581=DIRECTION('',(1.,0.,0.));
#21582=DIRECTION('',(-1.,0.,0.));
#21583=DIRECTION('center_axis',(0.,-1.,0.));
#21584=DIRECTION('ref_axis',(-0.707106781186555,0.,-0.70710678118654));
#21585=DIRECTION('center_axis',(0.,1.,0.));
#21586=DIRECTION('ref_axis',(-0.707106781186555,0.,-0.70710678118654));
#21587=DIRECTION('',(0.707106781186535,0.70710678118656,0.));
#21588=DIRECTION('center_axis',(0.,-1.,0.));
#21589=DIRECTION('ref_axis',(-0.707106781186555,0.,-0.70710678118654));
#21590=DIRECTION('center_axis',(-0.707106781186548,0.707106781186548,0.));
#21591=DIRECTION('ref_axis',(0.,0.,1.));
#21592=DIRECTION('',(0.707106781186547,0.707106781186547,0.));
#21593=DIRECTION('',(0.,0.,-1.));
#21594=DIRECTION('',(0.,0.,1.));
#21595=DIRECTION('center_axis',(0.,1.,0.));
#21596=DIRECTION('ref_axis',(0.707106781186548,0.,0.707106781186548));
#21597=DIRECTION('center_axis',(0.,-1.,0.));
#21598=DIRECTION('ref_axis',(0.707106781186548,0.,0.707106781186548));
#21599=DIRECTION('',(0.,0.707106781186554,0.707106781186541));
#21600=DIRECTION('center_axis',(0.,1.,0.));
#21601=DIRECTION('ref_axis',(0.707106781186547,0.,0.707106781186547));
#21602=DIRECTION('center_axis',(0.,0.707106781186543,-0.707106781186552));
#21603=DIRECTION('ref_axis',(-1.,0.,0.));
#21604=DIRECTION('',(0.,0.707106781186552,0.707106781186543));
#21605=DIRECTION('',(1.,0.,0.));
#21606=DIRECTION('center_axis',(0.,1.,0.));
#21607=DIRECTION('ref_axis',(-0.707106781186548,0.,0.707106781186548));
#21608=DIRECTION('',(-0.707106781186547,0.707106781186547,0.));
#21609=DIRECTION('center_axis',(0.,1.,0.));
#21610=DIRECTION('ref_axis',(-0.707106781186547,0.,0.707106781186547));
#21611=DIRECTION('center_axis',(0.707106781186554,0.707106781186541,0.));
#21612=DIRECTION('ref_axis',(0.,0.,-1.));
#21613=DIRECTION('',(-0.707106781186541,0.707106781186554,0.));
#21614=DIRECTION('',(0.,0.,1.));
#21615=DIRECTION('center_axis',(0.,-1.,0.));
#21616=DIRECTION('ref_axis',(0.707106781186548,0.,-0.707106781186548));
#21617=DIRECTION('',(0.,0.707106781186553,0.707106781186542));
#21618=DIRECTION('center_axis',(0.,-1.,0.));
#21619=DIRECTION('ref_axis',(0.707106781186547,0.,-0.707106781186547));
#21620=DIRECTION('center_axis',(0.,0.707106781186543,-0.707106781186552));
#21621=DIRECTION('ref_axis',(-1.,0.,0.));
#21622=DIRECTION('',(0.,0.707106781186552,0.707106781186543));
#21623=DIRECTION('',(1.,0.,0.));
#21624=DIRECTION('center_axis',(0.,-1.,0.));
#21625=DIRECTION('ref_axis',(-0.707106781186548,0.,-0.707106781186548));
#21626=DIRECTION('',(0.707106781186541,0.707106781186554,0.));
#21627=DIRECTION('center_axis',(0.,-1.,0.));
#21628=DIRECTION('ref_axis',(-0.707106781186547,0.,-0.707106781186547));
#21629=DIRECTION('center_axis',(-0.707106781186554,0.707106781186541,0.));
#21630=DIRECTION('ref_axis',(0.,0.,1.));
#21631=DIRECTION('',(0.707106781186541,0.707106781186554,0.));
#21632=DIRECTION('',(0.,0.,-1.));
#21633=DIRECTION('center_axis',(0.,-1.,0.));
#21634=DIRECTION('ref_axis',(-0.707106781186548,0.,0.707106781186548));
#21635=DIRECTION('center_axis',(0.,-1.,0.));
#21636=DIRECTION('ref_axis',(-0.707106781186547,0.,0.707106781186547));
#21637=DIRECTION('center_axis',(0.,1.,0.));
#21638=DIRECTION('ref_axis',(0.707106781186548,0.,0.707106781186548));
#21639=DIRECTION('',(0.,-1.,0.));
#21640=DIRECTION('center_axis',(-1.,0.,0.));
#21641=DIRECTION('ref_axis',(0.,0.,1.));
#21642=DIRECTION('',(0.,1.,0.));
#21643=DIRECTION('center_axis',(0.,1.,0.));
#21644=DIRECTION('ref_axis',(-0.707106781186555,0.,-0.70710678118654));
#21645=DIRECTION('',(0.,-1.,0.));
#21646=DIRECTION('center_axis',(0.,0.,-1.));
#21647=DIRECTION('ref_axis',(-1.,0.,0.));
#21648=DIRECTION('',(0.,1.,0.));
#21649=DIRECTION('center_axis',(0.,1.,0.));
#21650=DIRECTION('ref_axis',(0.70710678118654,0.,-0.707106781186555));
#21651=DIRECTION('',(0.,-1.,0.));
#21652=DIRECTION('center_axis',(1.,0.,0.));
#21653=DIRECTION('ref_axis',(0.,0.,-1.));
#21654=DIRECTION('',(0.,1.,0.));
#21655=DIRECTION('center_axis',(0.,1.,0.));
#21656=DIRECTION('ref_axis',(0.707106781186555,0.,0.70710678118654));
#21657=DIRECTION('center_axis',(0.,1.,0.));
#21658=DIRECTION('ref_axis',(0.,0.,1.));
#21659=DIRECTION('center_axis',(0.,0.,1.));
#21660=DIRECTION('ref_axis',(1.,0.,0.));
#21661=DIRECTION('',(0.707106781186548,8.65956056235493E-17,-0.707106781186548));
#21662=DIRECTION('center_axis',(0.,0.,1.));
#21663=DIRECTION('ref_axis',(1.,0.,0.));
#21664=DIRECTION('',(0.707106781186548,8.65956056235493E-17,-0.707106781186548));
#21665=DIRECTION('center_axis',(0.,0.,-1.));
#21666=DIRECTION('ref_axis',(1.,0.,0.));
#21667=DIRECTION('',(0.,0.,-1.));
#21668=DIRECTION('center_axis',(0.,0.,-1.));
#21669=DIRECTION('ref_axis',(1.,0.,0.));
#21670=DIRECTION('',(0.,0.,-1.));
#21671=DIRECTION('center_axis',(0.,0.,-1.));
#21672=DIRECTION('ref_axis',(1.,0.,0.));
#21673=DIRECTION('',(0.,0.,-1.));
#21674=DIRECTION('center_axis',(0.,0.,-1.));
#21675=DIRECTION('ref_axis',(1.,0.,0.));
#21676=DIRECTION('',(0.,0.,-1.));
#21677=DIRECTION('axis',(0.,0.,1.));
#21678=DIRECTION('refdir',(1.,0.,0.));
#21679=DIRECTION('center_axis',(1.,0.,0.));
#21680=DIRECTION('ref_axis',(0.,1.,0.));
#21681=DIRECTION('',(-1.,0.,0.));
#21682=DIRECTION('center_axis',(-1.,0.,0.));
#21683=DIRECTION('ref_axis',(0.,1.,0.));
#21684=DIRECTION('center_axis',(1.,0.,0.));
#21685=DIRECTION('ref_axis',(0.,1.,0.));
#21686=DIRECTION('',(-1.,0.,0.));
#21687=DIRECTION('center_axis',(1.,0.,0.));
#21688=DIRECTION('ref_axis',(0.,1.,0.));
#21689=DIRECTION('',(-1.,0.,0.));
#21690=DIRECTION('center_axis',(1.,0.,0.));
#21691=DIRECTION('ref_axis',(0.,1.,0.));
#21692=DIRECTION('',(-1.,0.,0.));
#21693=DIRECTION('center_axis',(1.,0.,0.));
#21694=DIRECTION('ref_axis',(0.,1.,0.));
#21695=DIRECTION('',(-1.,0.,0.));
#21696=DIRECTION('center_axis',(1.,0.,0.));
#21697=DIRECTION('ref_axis',(0.,1.,0.));
#21698=DIRECTION('',(-1.,0.,0.));
#21699=DIRECTION('center_axis',(1.,0.,0.));
#21700=DIRECTION('ref_axis',(0.,1.,0.));
#21701=DIRECTION('',(-1.,0.,0.));
#21702=DIRECTION('center_axis',(1.,0.,0.));
#21703=DIRECTION('ref_axis',(0.,1.,0.));
#21704=DIRECTION('',(-1.,0.,0.));
#21705=DIRECTION('center_axis',(1.,0.,0.));
#21706=DIRECTION('ref_axis',(0.,1.,0.));
#21707=DIRECTION('',(-1.,0.,0.));
#21708=DIRECTION('center_axis',(1.,0.,0.));
#21709=DIRECTION('ref_axis',(0.,1.,0.));
#21710=DIRECTION('',(-1.,0.,0.));
#21711=DIRECTION('center_axis',(-1.,0.,0.));
#21712=DIRECTION('ref_axis',(0.,1.,0.));
#21713=DIRECTION('center_axis',(1.,0.,0.));
#21714=DIRECTION('ref_axis',(0.,0.315640347057222,-0.948878902341915));
#21715=DIRECTION('',(1.,0.,0.));
#21716=DIRECTION('center_axis',(1.,0.,0.));
#21717=DIRECTION('ref_axis',(0.,1.,5.66627894982857E-14));
#21718=DIRECTION('center_axis',(1.,0.,0.));
#21719=DIRECTION('ref_axis',(0.,1.,5.66627894982857E-14));
#21720=DIRECTION('',(1.,0.,0.));
#21721=DIRECTION('center_axis',(1.,0.,0.));
#21722=DIRECTION('ref_axis',(0.,1.,5.66627894982857E-14));
#21723=DIRECTION('',(1.,0.,0.));
#21724=DIRECTION('center_axis',(1.,0.,0.));
#21725=DIRECTION('ref_axis',(0.,1.,5.66627894982857E-14));
#21726=DIRECTION('',(1.,0.,0.));
#21727=DIRECTION('center_axis',(1.,0.,0.));
#21728=DIRECTION('ref_axis',(0.,1.,5.66627894982857E-14));
#21729=DIRECTION('',(1.,0.,0.));
#21730=DIRECTION('center_axis',(1.,0.,0.));
#21731=DIRECTION('ref_axis',(0.,1.,5.66627894982857E-14));
#21732=DIRECTION('',(1.,0.,0.));
#21733=DIRECTION('center_axis',(1.,0.,0.));
#21734=DIRECTION('ref_axis',(0.,1.,5.66627894982857E-14));
#21735=DIRECTION('',(1.,0.,0.));
#21736=DIRECTION('center_axis',(1.,0.,0.));
#21737=DIRECTION('ref_axis',(0.,1.,5.66627894982857E-14));
#21738=DIRECTION('',(1.,0.,0.));
#21739=DIRECTION('center_axis',(1.,0.,0.));
#21740=DIRECTION('ref_axis',(0.,1.,5.66627894982857E-14));
#21741=DIRECTION('',(1.,0.,0.));
#21742=DIRECTION('center_axis',(1.,0.,6.92018220157537E-16));
#21743=DIRECTION('ref_axis',(0.,-1.,-3.00652077147108E-17));
#21744=DIRECTION('center_axis',(-1.,0.,0.));
#21745=DIRECTION('ref_axis',(0.,-1.,0.));
#21746=DIRECTION('center_axis',(-1.,0.,0.));
#21747=DIRECTION('ref_axis',(0.,-1.,0.));
#21748=DIRECTION('',(-0.923879532511287,-0.382683432365088,-6.97712130664736E-16));
#21749=DIRECTION('center_axis',(1.,0.,0.));
#21750=DIRECTION('ref_axis',(0.,-1.,-6.12323399573677E-17));
#21751=DIRECTION('center_axis',(1.,0.,0.));
#21752=DIRECTION('ref_axis',(0.,-1.,-6.12323399573677E-17));
#21753=DIRECTION('center_axis',(1.,0.,0.));
#21754=DIRECTION('ref_axis',(0.,1.,0.));
#21755=DIRECTION('',(-0.707106781186548,0.707106781186547,8.65956056235493E-17));
#21756=DIRECTION('center_axis',(-1.,0.,0.));
#21757=DIRECTION('ref_axis',(0.,-1.,-6.12323399573677E-17));
#21758=DIRECTION('center_axis',(-1.,0.,0.));
#21759=DIRECTION('ref_axis',(0.,-1.,-6.12323399573677E-17));
#21760=DIRECTION('center_axis',(1.,0.,0.));
#21761=DIRECTION('ref_axis',(0.,1.,0.));
#21762=DIRECTION('center_axis',(1.,0.,0.));
#21763=DIRECTION('ref_axis',(0.,0.,-1.));
#21764=DIRECTION('',(-1.,0.,0.));
#21765=DIRECTION('center_axis',(1.,0.,-1.61995324118126E-15));
#21766=DIRECTION('ref_axis',(0.,-1.,-3.20798861992349E-17));
#21767=DIRECTION('',(-0.382683432365089,-0.923879532511287,4.7714870511266E-16));
#21768=DIRECTION('center_axis',(1.,0.,0.));
#21769=DIRECTION('ref_axis',(0.,-1.,0.));
#21770=DIRECTION('center_axis',(-1.,0.,0.));
#21771=DIRECTION('ref_axis',(0.,0.,1.));
#21772=DIRECTION('center_axis',(1.,0.,0.));
#21773=DIRECTION('ref_axis',(0.,0.,-1.));
#21774=DIRECTION('center_axis',(-1.,0.,0.));
#21775=DIRECTION('ref_axis',(0.,1.,0.));
#21776=DIRECTION('center_axis',(1.,0.,0.));
#21777=DIRECTION('ref_axis',(0.,1.,5.66627894982857E-14));
#21778=DIRECTION('center_axis',(-1.,0.,0.));
#21779=DIRECTION('ref_axis',(0.,1.,5.66627894982857E-14));
#21780=DIRECTION('center_axis',(1.,0.,0.));
#21781=DIRECTION('ref_axis',(0.,-0.970927363150326,-0.23937429996964));
#21782=DIRECTION('center_axis',(-1.,0.,0.));
#21783=DIRECTION('ref_axis',(0.,1.,0.));
#21784=DIRECTION('center_axis',(-1.,0.,0.));
#21785=DIRECTION('ref_axis',(0.,1.,0.));
#21786=DIRECTION('center_axis',(1.,0.,0.));
#21787=DIRECTION('ref_axis',(0.,0.,-1.));
#21788=DIRECTION('',(-0.707106781186547,-0.707106781186548,-8.65956056235493E-17));
#21789=DIRECTION('center_axis',(1.,0.,0.));
#21790=DIRECTION('ref_axis',(0.,0.,-1.));
#21791=DIRECTION('center_axis',(-1.,0.,0.));
#21792=DIRECTION('ref_axis',(0.,1.,0.));
#21793=DIRECTION('center_axis',(1.,0.,0.));
#21794=DIRECTION('ref_axis',(0.,0.,-1.));
#21795=DIRECTION('',(-0.707106781186546,-0.707106781186549,-8.65956056235495E-17));
#21796=DIRECTION('center_axis',(1.,0.,0.));
#21797=DIRECTION('ref_axis',(0.,0.,-1.));
#21798=DIRECTION('axis',(0.,0.,1.));
#21799=DIRECTION('refdir',(1.,0.,0.));
#21800=DIRECTION('center_axis',(1.,0.,0.));
#21801=DIRECTION('ref_axis',(0.,1.,0.));
#21802=DIRECTION('',(-1.,0.,0.));
#21803=DIRECTION('center_axis',(1.,0.,0.));
#21804=DIRECTION('ref_axis',(0.,1.,0.));
#21805=DIRECTION('center_axis',(1.,0.,0.));
#21806=DIRECTION('ref_axis',(0.,1.,0.));
#21807=DIRECTION('',(-1.,0.,0.));
#21808=DIRECTION('center_axis',(1.,0.,0.));
#21809=DIRECTION('ref_axis',(0.,1.,0.));
#21810=DIRECTION('',(-1.,0.,0.));
#21811=DIRECTION('center_axis',(1.,0.,0.));
#21812=DIRECTION('ref_axis',(0.,1.,0.));
#21813=DIRECTION('',(-1.,0.,0.));
#21814=DIRECTION('center_axis',(1.,0.,0.));
#21815=DIRECTION('ref_axis',(0.,1.,0.));
#21816=DIRECTION('',(-1.,0.,0.));
#21817=DIRECTION('center_axis',(1.,0.,0.));
#21818=DIRECTION('ref_axis',(0.,1.,0.));
#21819=DIRECTION('',(-1.,0.,0.));
#21820=DIRECTION('center_axis',(1.,0.,0.));
#21821=DIRECTION('ref_axis',(0.,1.,0.));
#21822=DIRECTION('',(-1.,0.,0.));
#21823=DIRECTION('center_axis',(1.,0.,0.));
#21824=DIRECTION('ref_axis',(0.,1.,0.));
#21825=DIRECTION('',(-1.,0.,0.));
#21826=DIRECTION('center_axis',(1.,0.,0.));
#21827=DIRECTION('ref_axis',(0.,1.,0.));
#21828=DIRECTION('',(-1.,0.,0.));
#21829=DIRECTION('center_axis',(1.,0.,0.));
#21830=DIRECTION('ref_axis',(0.,1.,0.));
#21831=DIRECTION('',(-1.,0.,0.));
#21832=DIRECTION('center_axis',(1.,0.,0.));
#21833=DIRECTION('ref_axis',(0.,1.,0.));
#21834=DIRECTION('',(-1.,0.,0.));
#21835=DIRECTION('center_axis',(1.,0.,0.));
#21836=DIRECTION('ref_axis',(0.,1.,0.));
#21837=DIRECTION('',(-1.,0.,0.));
#21838=DIRECTION('center_axis',(1.,0.,0.));
#21839=DIRECTION('ref_axis',(0.,1.,0.));
#21840=DIRECTION('',(-1.,0.,0.));
#21841=DIRECTION('center_axis',(1.,0.,0.));
#21842=DIRECTION('ref_axis',(0.,1.,0.));
#21843=DIRECTION('',(-1.,0.,0.));
#21844=DIRECTION('center_axis',(1.,0.,0.));
#21845=DIRECTION('ref_axis',(0.,1.,0.));
#21846=DIRECTION('',(-1.,0.,0.));
#21847=DIRECTION('center_axis',(1.,0.,0.));
#21848=DIRECTION('ref_axis',(0.,1.,0.));
#21849=DIRECTION('',(-1.,0.,0.));
#21850=DIRECTION('center_axis',(1.,0.,0.));
#21851=DIRECTION('ref_axis',(0.,1.,0.));
#21852=DIRECTION('',(-1.,0.,0.));
#21853=DIRECTION('center_axis',(1.,0.,0.));
#21854=DIRECTION('ref_axis',(0.,1.,0.));
#21855=DIRECTION('',(-1.,0.,0.));
#21856=DIRECTION('center_axis',(1.,0.,0.));
#21857=DIRECTION('ref_axis',(0.,1.,0.));
#21858=DIRECTION('',(-1.,0.,0.));
#21859=DIRECTION('center_axis',(1.,0.,0.));
#21860=DIRECTION('ref_axis',(0.,1.,0.));
#21861=DIRECTION('',(-1.,0.,0.));
#21862=DIRECTION('center_axis',(1.,0.,0.));
#21863=DIRECTION('ref_axis',(0.,1.,0.));
#21864=DIRECTION('',(-1.,0.,0.));
#21865=DIRECTION('center_axis',(1.,0.,0.));
#21866=DIRECTION('ref_axis',(0.,1.,0.));
#21867=DIRECTION('',(-1.,0.,0.));
#21868=DIRECTION('center_axis',(1.,0.,0.));
#21869=DIRECTION('ref_axis',(0.,1.,0.));
#21870=DIRECTION('',(-1.,0.,0.));
#21871=DIRECTION('center_axis',(1.,0.,0.));
#21872=DIRECTION('ref_axis',(0.,1.,0.));
#21873=DIRECTION('',(-1.,0.,0.));
#21874=DIRECTION('center_axis',(1.,0.,0.));
#21875=DIRECTION('ref_axis',(0.,1.,0.));
#21876=DIRECTION('',(-1.,0.,0.));
#21877=DIRECTION('center_axis',(1.,0.,0.));
#21878=DIRECTION('ref_axis',(0.,1.,0.));
#21879=DIRECTION('',(-1.,0.,0.));
#21880=DIRECTION('center_axis',(1.,0.,0.));
#21881=DIRECTION('ref_axis',(0.,1.,0.));
#21882=DIRECTION('',(-1.,0.,0.));
#21883=DIRECTION('center_axis',(1.,0.,0.));
#21884=DIRECTION('ref_axis',(0.,1.,0.));
#21885=DIRECTION('',(-1.,0.,0.));
#21886=DIRECTION('center_axis',(1.,0.,0.));
#21887=DIRECTION('ref_axis',(0.,1.,0.));
#21888=DIRECTION('',(-1.,0.,0.));
#21889=DIRECTION('center_axis',(1.,0.,0.));
#21890=DIRECTION('ref_axis',(0.,1.,0.));
#21891=DIRECTION('',(-1.,0.,0.));
#21892=DIRECTION('center_axis',(1.,0.,0.));
#21893=DIRECTION('ref_axis',(0.,1.,0.));
#21894=DIRECTION('',(-1.,0.,0.));
#21895=DIRECTION('center_axis',(1.,0.,0.));
#21896=DIRECTION('ref_axis',(0.,1.,0.));
#21897=DIRECTION('',(-1.,0.,0.));
#21898=DIRECTION('center_axis',(1.,0.,0.));
#21899=DIRECTION('ref_axis',(0.,1.,0.));
#21900=DIRECTION('',(-1.,0.,0.));
#21901=DIRECTION('center_axis',(1.,0.,0.));
#21902=DIRECTION('ref_axis',(0.,1.,0.));
#21903=DIRECTION('',(-1.,0.,0.));
#21904=DIRECTION('center_axis',(1.,0.,0.));
#21905=DIRECTION('ref_axis',(0.,1.,0.));
#21906=DIRECTION('',(-1.,0.,0.));
#21907=DIRECTION('center_axis',(1.,0.,0.));
#21908=DIRECTION('ref_axis',(0.,1.,0.));
#21909=DIRECTION('',(-1.,0.,0.));
#21910=DIRECTION('center_axis',(1.,0.,0.));
#21911=DIRECTION('ref_axis',(0.,1.,0.));
#21912=DIRECTION('',(-1.,0.,0.));
#21913=DIRECTION('center_axis',(1.,0.,0.));
#21914=DIRECTION('ref_axis',(0.,1.,0.));
#21915=DIRECTION('',(-1.,0.,0.));
#21916=DIRECTION('center_axis',(1.,0.,0.));
#21917=DIRECTION('ref_axis',(0.,1.,0.));
#21918=DIRECTION('',(-1.,0.,0.));
#21919=DIRECTION('center_axis',(1.,0.,0.));
#21920=DIRECTION('ref_axis',(0.,1.,0.));
#21921=DIRECTION('',(-1.,0.,0.));
#21922=DIRECTION('center_axis',(1.,0.,0.));
#21923=DIRECTION('ref_axis',(0.,1.,0.));
#21924=DIRECTION('',(-1.,0.,0.));
#21925=DIRECTION('center_axis',(1.,0.,0.));
#21926=DIRECTION('ref_axis',(0.,1.,0.));
#21927=DIRECTION('',(-1.,0.,0.));
#21928=DIRECTION('center_axis',(1.,0.,0.));
#21929=DIRECTION('ref_axis',(0.,1.,0.));
#21930=DIRECTION('',(-1.,0.,0.));
#21931=DIRECTION('center_axis',(1.,0.,0.));
#21932=DIRECTION('ref_axis',(0.,1.,0.));
#21933=DIRECTION('',(-1.,0.,0.));
#21934=DIRECTION('center_axis',(1.,0.,0.));
#21935=DIRECTION('ref_axis',(0.,1.,-5.15647387410054E-13));
#21936=DIRECTION('',(1.,0.,0.));
#21937=DIRECTION('center_axis',(1.,0.,0.));
#21938=DIRECTION('ref_axis',(0.,1.,-5.15647387410054E-13));
#21939=DIRECTION('center_axis',(1.,0.,0.));
#21940=DIRECTION('ref_axis',(0.,1.,-5.15647387410054E-13));
#21941=DIRECTION('',(1.,0.,0.));
#21942=DIRECTION('center_axis',(1.,0.,0.));
#21943=DIRECTION('ref_axis',(0.,1.,-5.15647387410054E-13));
#21944=DIRECTION('center_axis',(1.,0.,0.));
#21945=DIRECTION('ref_axis',(0.,1.,-5.15647387410054E-13));
#21946=DIRECTION('',(1.,0.,0.));
#21947=DIRECTION('center_axis',(1.,0.,0.));
#21948=DIRECTION('ref_axis',(0.,1.,-5.15647387410054E-13));
#21949=DIRECTION('',(1.,0.,0.));
#21950=DIRECTION('center_axis',(1.,0.,0.));
#21951=DIRECTION('ref_axis',(0.,1.,-5.15647387410054E-13));
#21952=DIRECTION('',(1.,0.,0.));
#21953=DIRECTION('center_axis',(1.,0.,0.));
#21954=DIRECTION('ref_axis',(0.,1.,-5.15647387410054E-13));
#21955=DIRECTION('',(1.,0.,0.));
#21956=DIRECTION('center_axis',(1.,0.,0.));
#21957=DIRECTION('ref_axis',(0.,1.,-5.15647387410054E-13));
#21958=DIRECTION('',(1.,0.,0.));
#21959=DIRECTION('center_axis',(1.,0.,0.));
#21960=DIRECTION('ref_axis',(0.,1.,-5.15647387410054E-13));
#21961=DIRECTION('',(1.,0.,0.));
#21962=DIRECTION('center_axis',(1.,0.,0.));
#21963=DIRECTION('ref_axis',(0.,1.,-5.15647387410054E-13));
#21964=DIRECTION('',(1.,0.,0.));
#21965=DIRECTION('center_axis',(1.,0.,0.));
#21966=DIRECTION('ref_axis',(0.,1.,-5.15647387410054E-13));
#21967=DIRECTION('',(1.,0.,0.));
#21968=DIRECTION('center_axis',(1.,0.,0.));
#21969=DIRECTION('ref_axis',(0.,1.,-5.15647387410054E-13));
#21970=DIRECTION('',(1.,0.,0.));
#21971=DIRECTION('center_axis',(1.,0.,0.));
#21972=DIRECTION('ref_axis',(0.,1.,-5.15647387410054E-13));
#21973=DIRECTION('',(1.,0.,0.));
#21974=DIRECTION('center_axis',(1.,0.,0.));
#21975=DIRECTION('ref_axis',(0.,1.,-5.15647387410054E-13));
#21976=DIRECTION('',(1.,0.,0.));
#21977=DIRECTION('center_axis',(1.,0.,0.));
#21978=DIRECTION('ref_axis',(0.,1.,-5.15647387410054E-13));
#21979=DIRECTION('',(1.,0.,0.));
#21980=DIRECTION('center_axis',(1.,0.,0.));
#21981=DIRECTION('ref_axis',(0.,1.,-5.15647387410054E-13));
#21982=DIRECTION('',(1.,0.,0.));
#21983=DIRECTION('center_axis',(1.,0.,0.));
#21984=DIRECTION('ref_axis',(0.,1.,-5.15647387410054E-13));
#21985=DIRECTION('',(1.,0.,0.));
#21986=DIRECTION('center_axis',(1.,0.,0.));
#21987=DIRECTION('ref_axis',(0.,1.,-5.15647387410054E-13));
#21988=DIRECTION('',(1.,0.,0.));
#21989=DIRECTION('center_axis',(1.,0.,0.));
#21990=DIRECTION('ref_axis',(0.,1.,-5.15647387410054E-13));
#21991=DIRECTION('',(1.,0.,0.));
#21992=DIRECTION('center_axis',(1.,0.,0.));
#21993=DIRECTION('ref_axis',(0.,1.,-5.15647387410054E-13));
#21994=DIRECTION('',(1.,0.,0.));
#21995=DIRECTION('center_axis',(1.,0.,0.));
#21996=DIRECTION('ref_axis',(0.,1.,-5.15647387410054E-13));
#21997=DIRECTION('',(1.,0.,0.));
#21998=DIRECTION('center_axis',(1.,0.,0.));
#21999=DIRECTION('ref_axis',(0.,1.,-5.15647387410054E-13));
#22000=DIRECTION('',(1.,0.,0.));
#22001=DIRECTION('center_axis',(1.,0.,0.));
#22002=DIRECTION('ref_axis',(0.,1.,-5.15647387410054E-13));
#22003=DIRECTION('',(1.,0.,0.));
#22004=DIRECTION('center_axis',(1.,0.,0.));
#22005=DIRECTION('ref_axis',(0.,1.,-5.15647387410054E-13));
#22006=DIRECTION('',(1.,0.,0.));
#22007=DIRECTION('center_axis',(1.,0.,0.));
#22008=DIRECTION('ref_axis',(0.,1.,-5.15647387410054E-13));
#22009=DIRECTION('',(1.,0.,0.));
#22010=DIRECTION('center_axis',(1.,0.,0.));
#22011=DIRECTION('ref_axis',(0.,1.,-5.15647387410054E-13));
#22012=DIRECTION('',(1.,0.,0.));
#22013=DIRECTION('center_axis',(1.,0.,0.));
#22014=DIRECTION('ref_axis',(0.,1.,-5.15647387410054E-13));
#22015=DIRECTION('',(1.,0.,0.));
#22016=DIRECTION('center_axis',(1.,0.,0.));
#22017=DIRECTION('ref_axis',(0.,1.,-5.15647387410054E-13));
#22018=DIRECTION('',(1.,0.,0.));
#22019=DIRECTION('center_axis',(1.,0.,0.));
#22020=DIRECTION('ref_axis',(0.,1.,-5.15647387410054E-13));
#22021=DIRECTION('',(1.,0.,0.));
#22022=DIRECTION('center_axis',(1.,0.,0.));
#22023=DIRECTION('ref_axis',(0.,1.,-5.15647387410054E-13));
#22024=DIRECTION('',(1.,0.,0.));
#22025=DIRECTION('center_axis',(1.,0.,0.));
#22026=DIRECTION('ref_axis',(0.,1.,-5.15647387410054E-13));
#22027=DIRECTION('',(1.,0.,0.));
#22028=DIRECTION('center_axis',(1.,0.,0.));
#22029=DIRECTION('ref_axis',(0.,1.,-5.15647387410054E-13));
#22030=DIRECTION('',(1.,0.,0.));
#22031=DIRECTION('center_axis',(1.,0.,0.));
#22032=DIRECTION('ref_axis',(0.,1.,-5.15647387410054E-13));
#22033=DIRECTION('',(1.,0.,0.));
#22034=DIRECTION('center_axis',(1.,0.,0.));
#22035=DIRECTION('ref_axis',(0.,1.,-5.15647387410054E-13));
#22036=DIRECTION('',(1.,0.,0.));
#22037=DIRECTION('center_axis',(1.,0.,0.));
#22038=DIRECTION('ref_axis',(0.,1.,-5.15647387410054E-13));
#22039=DIRECTION('',(1.,0.,0.));
#22040=DIRECTION('center_axis',(1.,0.,0.));
#22041=DIRECTION('ref_axis',(0.,1.,-5.15647387410054E-13));
#22042=DIRECTION('',(1.,0.,0.));
#22043=DIRECTION('center_axis',(1.,0.,0.));
#22044=DIRECTION('ref_axis',(0.,1.,-5.15647387410054E-13));
#22045=DIRECTION('',(1.,0.,0.));
#22046=DIRECTION('center_axis',(1.,0.,0.));
#22047=DIRECTION('ref_axis',(0.,1.,-5.15647387410054E-13));
#22048=DIRECTION('',(1.,0.,0.));
#22049=DIRECTION('center_axis',(1.,0.,0.));
#22050=DIRECTION('ref_axis',(0.,1.,-5.15647387410054E-13));
#22051=DIRECTION('',(1.,0.,0.));
#22052=DIRECTION('center_axis',(1.,0.,0.));
#22053=DIRECTION('ref_axis',(0.,1.,-5.15647387410054E-13));
#22054=DIRECTION('',(1.,0.,0.));
#22055=DIRECTION('center_axis',(1.,0.,0.));
#22056=DIRECTION('ref_axis',(0.,1.,-5.15647387410054E-13));
#22057=DIRECTION('',(1.,0.,0.));
#22058=DIRECTION('center_axis',(1.,0.,0.));
#22059=DIRECTION('ref_axis',(0.,1.,-5.15647387410054E-13));
#22060=DIRECTION('',(1.,0.,0.));
#22061=DIRECTION('center_axis',(1.,0.,0.));
#22062=DIRECTION('ref_axis',(0.,1.,-5.15647387410054E-13));
#22063=DIRECTION('',(1.,0.,0.));
#22064=DIRECTION('center_axis',(1.,0.,0.));
#22065=DIRECTION('ref_axis',(0.,1.,-5.15647387410054E-13));
#22066=DIRECTION('',(1.,0.,0.));
#22067=DIRECTION('center_axis',(1.,0.,0.));
#22068=DIRECTION('ref_axis',(0.,1.,-5.15647387410054E-13));
#22069=DIRECTION('',(1.,0.,0.));
#22070=DIRECTION('center_axis',(1.,0.,0.));
#22071=DIRECTION('ref_axis',(0.,0.,-1.));
#22072=DIRECTION('center_axis',(1.,0.,0.));
#22073=DIRECTION('ref_axis',(0.,1.,0.));
#22074=DIRECTION('center_axis',(1.,0.,0.));
#22075=DIRECTION('ref_axis',(0.,1.,0.));
#22076=DIRECTION('center_axis',(-1.,0.,0.));
#22077=DIRECTION('ref_axis',(0.,1.,-5.15647387410054E-13));
#22078=DIRECTION('center_axis',(1.,0.,0.));
#22079=DIRECTION('ref_axis',(0.,1.,-5.15647387410054E-13));
#22080=DIRECTION('center_axis',(-1.,0.,0.));
#22081=DIRECTION('ref_axis',(0.,1.,0.));
#22082=DIRECTION('',(0.500490667348524,0.865741931465162,1.06022808525646E-16));
#22083=DIRECTION('center_axis',(1.,0.,0.));
#22084=DIRECTION('ref_axis',(0.,1.,0.));
#22085=DIRECTION('center_axis',(0.,-0.5,0.866025403784439));
#22086=DIRECTION('ref_axis',(0.,-0.866025403784439,-0.5));
#22087=DIRECTION('',(1.,0.,0.));
#22088=DIRECTION('',(0.,-0.866025403784439,-0.5));
#22089=DIRECTION('',(1.,0.,0.));
#22090=DIRECTION('center_axis',(0.,0.5,0.866025403784439));
#22091=DIRECTION('ref_axis',(0.,-0.866025403784439,0.5));
#22092=DIRECTION('',(1.,0.,0.));
#22093=DIRECTION('',(0.,-0.866025403784439,0.5));
#22094=DIRECTION('center_axis',(0.,1.,-4.43760619934668E-16));
#22095=DIRECTION('ref_axis',(0.,4.43760619934668E-16,1.));
#22096=DIRECTION('',(1.,0.,0.));
#22097=DIRECTION('',(0.,4.43760619934668E-16,1.));
#22098=DIRECTION('center_axis',(1.,0.,0.));
#22099=DIRECTION('ref_axis',(0.,0.,-1.));
#22100=DIRECTION('',(0.,0.866025403784439,0.5));
#22101=DIRECTION('',(0.,0.866025403784439,-0.5));
#22102=DIRECTION('',(0.,1.4792020664489E-16,-1.));
#22103=DIRECTION('center_axis',(-1.,0.,0.));
#22104=DIRECTION('ref_axis',(0.,1.,0.));
#22105=DIRECTION('center_axis',(0.,0.5,-0.866025403784439));
#22106=DIRECTION('ref_axis',(0.,0.866025403784439,0.5));
#22107=DIRECTION('',(1.,0.,0.));
#22108=DIRECTION('center_axis',(0.,-0.5,-0.866025403784439));
#22109=DIRECTION('ref_axis',(0.,0.866025403784439,-0.5));
#22110=DIRECTION('',(1.,0.,0.));
#22111=DIRECTION('center_axis',(0.,-1.,-1.4792020664489E-16));
#22112=DIRECTION('ref_axis',(0.,1.4792020664489E-16,-1.));
#22113=DIRECTION('center_axis',(1.,0.,0.));
#22114=DIRECTION('ref_axis',(0.,0.,-1.));
#22115=DIRECTION('center_axis',(-1.,0.,0.));
#22116=DIRECTION('ref_axis',(0.,0.,1.));
#22117=DIRECTION('center_axis',(1.,0.,0.));
#22118=DIRECTION('ref_axis',(0.,0.,-1.));
#22119=DIRECTION('center_axis',(1.,0.,0.));
#22120=DIRECTION('ref_axis',(0.,1.,0.));
#22121=DIRECTION('',(-0.707106781186546,0.707106781186549,8.65956056235495E-17));
#22122=DIRECTION('center_axis',(1.,0.,0.));
#22123=DIRECTION('ref_axis',(0.,1.,0.));
#22124=DIRECTION('axis',(0.,0.,1.));
#22125=DIRECTION('refdir',(1.,0.,0.));
#22126=DIRECTION('center_axis',(1.,0.,0.));
#22127=DIRECTION('ref_axis',(0.,1.,0.));
#22128=DIRECTION('',(-1.,0.,0.));
#22129=DIRECTION('center_axis',(1.,0.,0.));
#22130=DIRECTION('ref_axis',(0.,1.,0.));
#22131=DIRECTION('center_axis',(1.,0.,0.));
#22132=DIRECTION('ref_axis',(0.,1.,0.));
#22133=DIRECTION('',(-1.,0.,0.));
#22134=DIRECTION('center_axis',(1.,0.,0.));
#22135=DIRECTION('ref_axis',(0.,1.,0.));
#22136=DIRECTION('',(-1.,0.,0.));
#22137=DIRECTION('center_axis',(1.,0.,0.));
#22138=DIRECTION('ref_axis',(0.,1.,0.));
#22139=DIRECTION('',(-1.,0.,0.));
#22140=DIRECTION('center_axis',(1.,0.,0.));
#22141=DIRECTION('ref_axis',(0.,1.,0.));
#22142=DIRECTION('',(-1.,0.,0.));
#22143=DIRECTION('center_axis',(1.,0.,0.));
#22144=DIRECTION('ref_axis',(0.,1.,0.));
#22145=DIRECTION('',(-1.,0.,0.));
#22146=DIRECTION('center_axis',(1.,0.,0.));
#22147=DIRECTION('ref_axis',(0.,1.,0.));
#22148=DIRECTION('',(-1.,0.,0.));
#22149=DIRECTION('center_axis',(1.,0.,0.));
#22150=DIRECTION('ref_axis',(0.,1.,0.));
#22151=DIRECTION('',(-1.,0.,0.));
#22152=DIRECTION('center_axis',(1.,0.,0.));
#22153=DIRECTION('ref_axis',(0.,1.,0.));
#22154=DIRECTION('',(-1.,0.,0.));
#22155=DIRECTION('center_axis',(1.,0.,0.));
#22156=DIRECTION('ref_axis',(0.,1.,0.));
#22157=DIRECTION('',(-1.,0.,0.));
#22158=DIRECTION('center_axis',(1.,0.,0.));
#22159=DIRECTION('ref_axis',(0.,1.,0.));
#22160=DIRECTION('',(-1.,0.,0.));
#22161=DIRECTION('center_axis',(1.,0.,0.));
#22162=DIRECTION('ref_axis',(0.,1.,0.));
#22163=DIRECTION('',(-1.,0.,0.));
#22164=DIRECTION('center_axis',(1.,0.,0.));
#22165=DIRECTION('ref_axis',(0.,1.,0.));
#22166=DIRECTION('',(-1.,0.,0.));
#22167=DIRECTION('center_axis',(1.,0.,0.));
#22168=DIRECTION('ref_axis',(0.,1.,0.));
#22169=DIRECTION('',(-1.,0.,0.));
#22170=DIRECTION('center_axis',(1.,0.,0.));
#22171=DIRECTION('ref_axis',(0.,1.,0.));
#22172=DIRECTION('',(-1.,0.,0.));
#22173=DIRECTION('center_axis',(1.,0.,0.));
#22174=DIRECTION('ref_axis',(0.,1.,0.));
#22175=DIRECTION('',(-1.,0.,0.));
#22176=DIRECTION('center_axis',(1.,0.,0.));
#22177=DIRECTION('ref_axis',(0.,1.,0.));
#22178=DIRECTION('',(-1.,0.,0.));
#22179=DIRECTION('center_axis',(1.,0.,0.));
#22180=DIRECTION('ref_axis',(0.,1.,0.));
#22181=DIRECTION('',(-1.,0.,0.));
#22182=DIRECTION('center_axis',(1.,0.,0.));
#22183=DIRECTION('ref_axis',(0.,1.,0.));
#22184=DIRECTION('',(-1.,0.,0.));
#22185=DIRECTION('center_axis',(1.,0.,0.));
#22186=DIRECTION('ref_axis',(0.,1.,0.));
#22187=DIRECTION('',(-1.,0.,0.));
#22188=DIRECTION('center_axis',(1.,0.,0.));
#22189=DIRECTION('ref_axis',(0.,1.,0.));
#22190=DIRECTION('',(-1.,0.,0.));
#22191=DIRECTION('center_axis',(1.,0.,0.));
#22192=DIRECTION('ref_axis',(0.,1.,0.));
#22193=DIRECTION('',(-1.,0.,0.));
#22194=DIRECTION('center_axis',(1.,0.,0.));
#22195=DIRECTION('ref_axis',(0.,1.,0.));
#22196=DIRECTION('',(-1.,0.,0.));
#22197=DIRECTION('center_axis',(1.,0.,0.));
#22198=DIRECTION('ref_axis',(0.,1.,0.));
#22199=DIRECTION('',(-1.,0.,0.));
#22200=DIRECTION('center_axis',(1.,0.,0.));
#22201=DIRECTION('ref_axis',(0.,1.,0.));
#22202=DIRECTION('',(-1.,0.,0.));
#22203=DIRECTION('center_axis',(1.,0.,0.));
#22204=DIRECTION('ref_axis',(0.,1.,0.));
#22205=DIRECTION('',(-1.,0.,0.));
#22206=DIRECTION('center_axis',(1.,0.,0.));
#22207=DIRECTION('ref_axis',(0.,1.,0.));
#22208=DIRECTION('',(-1.,0.,0.));
#22209=DIRECTION('center_axis',(1.,0.,0.));
#22210=DIRECTION('ref_axis',(0.,1.,0.));
#22211=DIRECTION('',(-1.,0.,0.));
#22212=DIRECTION('center_axis',(1.,0.,0.));
#22213=DIRECTION('ref_axis',(0.,1.,0.));
#22214=DIRECTION('',(-1.,0.,0.));
#22215=DIRECTION('center_axis',(1.,0.,0.));
#22216=DIRECTION('ref_axis',(0.,1.,0.));
#22217=DIRECTION('',(-1.,0.,0.));
#22218=DIRECTION('center_axis',(1.,0.,0.));
#22219=DIRECTION('ref_axis',(0.,1.,0.));
#22220=DIRECTION('',(-1.,0.,0.));
#22221=DIRECTION('center_axis',(1.,0.,0.));
#22222=DIRECTION('ref_axis',(0.,1.,0.));
#22223=DIRECTION('',(-1.,0.,0.));
#22224=DIRECTION('center_axis',(1.,0.,0.));
#22225=DIRECTION('ref_axis',(0.,1.,0.));
#22226=DIRECTION('',(-1.,0.,0.));
#22227=DIRECTION('center_axis',(1.,0.,0.));
#22228=DIRECTION('ref_axis',(0.,1.,0.));
#22229=DIRECTION('',(-1.,0.,0.));
#22230=DIRECTION('center_axis',(1.,0.,0.));
#22231=DIRECTION('ref_axis',(0.,1.,0.));
#22232=DIRECTION('',(-1.,0.,0.));
#22233=DIRECTION('center_axis',(1.,0.,0.));
#22234=DIRECTION('ref_axis',(0.,1.,0.));
#22235=DIRECTION('',(-1.,0.,0.));
#22236=DIRECTION('center_axis',(1.,0.,0.));
#22237=DIRECTION('ref_axis',(0.,1.,0.));
#22238=DIRECTION('',(-1.,0.,0.));
#22239=DIRECTION('center_axis',(1.,0.,0.));
#22240=DIRECTION('ref_axis',(0.,1.,0.));
#22241=DIRECTION('',(-1.,0.,0.));
#22242=DIRECTION('center_axis',(1.,0.,0.));
#22243=DIRECTION('ref_axis',(0.,1.,0.));
#22244=DIRECTION('',(-1.,0.,0.));
#22245=DIRECTION('center_axis',(1.,0.,0.));
#22246=DIRECTION('ref_axis',(0.,1.,0.));
#22247=DIRECTION('',(-1.,0.,0.));
#22248=DIRECTION('center_axis',(1.,0.,0.));
#22249=DIRECTION('ref_axis',(0.,1.,0.));
#22250=DIRECTION('',(-1.,0.,0.));
#22251=DIRECTION('center_axis',(1.,0.,0.));
#22252=DIRECTION('ref_axis',(0.,1.,0.));
#22253=DIRECTION('',(-1.,0.,0.));
#22254=DIRECTION('center_axis',(1.,0.,0.));
#22255=DIRECTION('ref_axis',(0.,1.,0.));
#22256=DIRECTION('',(-1.,0.,0.));
#22257=DIRECTION('center_axis',(1.,0.,0.));
#22258=DIRECTION('ref_axis',(0.,1.,0.));
#22259=DIRECTION('',(-1.,0.,0.));
#22260=DIRECTION('center_axis',(1.,0.,0.));
#22261=DIRECTION('ref_axis',(0.,1.,0.));
#22262=DIRECTION('',(-1.,0.,0.));
#22263=DIRECTION('center_axis',(1.,0.,0.));
#22264=DIRECTION('ref_axis',(0.,1.,0.));
#22265=DIRECTION('',(-1.,0.,0.));
#22266=DIRECTION('center_axis',(1.,0.,0.));
#22267=DIRECTION('ref_axis',(0.,1.,0.));
#22268=DIRECTION('',(-1.,0.,0.));
#22269=DIRECTION('center_axis',(1.,0.,0.));
#22270=DIRECTION('ref_axis',(0.,1.,0.));
#22271=DIRECTION('',(-1.,0.,0.));
#22272=DIRECTION('center_axis',(1.,0.,0.));
#22273=DIRECTION('ref_axis',(0.,1.,0.));
#22274=DIRECTION('',(-1.,0.,0.));
#22275=DIRECTION('center_axis',(1.,0.,0.));
#22276=DIRECTION('ref_axis',(0.,1.,0.));
#22277=DIRECTION('',(-1.,0.,0.));
#22278=DIRECTION('center_axis',(1.,0.,0.));
#22279=DIRECTION('ref_axis',(0.,1.,0.));
#22280=DIRECTION('',(-1.,0.,0.));
#22281=DIRECTION('center_axis',(1.,0.,0.));
#22282=DIRECTION('ref_axis',(0.,1.,0.));
#22283=DIRECTION('',(-1.,0.,0.));
#22284=DIRECTION('center_axis',(1.,0.,0.));
#22285=DIRECTION('ref_axis',(0.,1.,0.));
#22286=DIRECTION('',(-1.,0.,0.));
#22287=DIRECTION('center_axis',(1.,0.,0.));
#22288=DIRECTION('ref_axis',(0.,1.,0.));
#22289=DIRECTION('',(-1.,0.,0.));
#22290=DIRECTION('center_axis',(1.,0.,0.));
#22291=DIRECTION('ref_axis',(0.,1.,0.));
#22292=DIRECTION('',(-1.,0.,0.));
#22293=DIRECTION('center_axis',(1.,0.,0.));
#22294=DIRECTION('ref_axis',(0.,1.,0.));
#22295=DIRECTION('',(-1.,0.,0.));
#22296=DIRECTION('center_axis',(1.,0.,0.));
#22297=DIRECTION('ref_axis',(0.,1.,0.));
#22298=DIRECTION('',(-1.,0.,0.));
#22299=DIRECTION('center_axis',(1.,0.,0.));
#22300=DIRECTION('ref_axis',(0.,1.,0.));
#22301=DIRECTION('',(-1.,0.,0.));
#22302=DIRECTION('center_axis',(1.,0.,0.));
#22303=DIRECTION('ref_axis',(0.,1.,0.));
#22304=DIRECTION('',(-1.,0.,0.));
#22305=DIRECTION('center_axis',(1.,0.,0.));
#22306=DIRECTION('ref_axis',(0.,1.,0.));
#22307=DIRECTION('',(-1.,0.,0.));
#22308=DIRECTION('center_axis',(1.,0.,0.));
#22309=DIRECTION('ref_axis',(0.,1.,0.));
#22310=DIRECTION('',(-1.,0.,0.));
#22311=DIRECTION('center_axis',(1.,0.,0.));
#22312=DIRECTION('ref_axis',(0.,1.,0.));
#22313=DIRECTION('',(-1.,0.,0.));
#22314=DIRECTION('center_axis',(1.,0.,0.));
#22315=DIRECTION('ref_axis',(0.,1.,0.));
#22316=DIRECTION('',(-1.,0.,0.));
#22317=DIRECTION('center_axis',(1.,0.,0.));
#22318=DIRECTION('ref_axis',(0.,1.,0.));
#22319=DIRECTION('',(-1.,0.,0.));
#22320=DIRECTION('center_axis',(1.,0.,0.));
#22321=DIRECTION('ref_axis',(0.,1.,0.));
#22322=DIRECTION('',(-1.,0.,0.));
#22323=DIRECTION('center_axis',(1.,0.,0.));
#22324=DIRECTION('ref_axis',(0.,1.,0.));
#22325=DIRECTION('',(-1.,0.,0.));
#22326=DIRECTION('center_axis',(1.,0.,0.));
#22327=DIRECTION('ref_axis',(0.,1.,0.));
#22328=DIRECTION('',(-1.,0.,0.));
#22329=DIRECTION('center_axis',(1.,0.,0.));
#22330=DIRECTION('ref_axis',(0.,1.,0.));
#22331=DIRECTION('',(-1.,0.,0.));
#22332=DIRECTION('center_axis',(1.,0.,0.));
#22333=DIRECTION('ref_axis',(0.,1.,0.));
#22334=DIRECTION('',(-1.,0.,0.));
#22335=DIRECTION('center_axis',(1.,0.,0.));
#22336=DIRECTION('ref_axis',(0.,1.,0.));
#22337=DIRECTION('',(-1.,0.,0.));
#22338=DIRECTION('center_axis',(1.,0.,0.));
#22339=DIRECTION('ref_axis',(0.,1.,0.));
#22340=DIRECTION('',(-1.,0.,0.));
#22341=DIRECTION('center_axis',(1.,0.,0.));
#22342=DIRECTION('ref_axis',(0.,1.,0.));
#22343=DIRECTION('',(-1.,0.,0.));
#22344=DIRECTION('center_axis',(1.,0.,0.));
#22345=DIRECTION('ref_axis',(0.,1.,0.));
#22346=DIRECTION('',(-1.,0.,0.));
#22347=DIRECTION('center_axis',(1.,0.,0.));
#22348=DIRECTION('ref_axis',(0.,1.,0.));
#22349=DIRECTION('',(-1.,0.,0.));
#22350=DIRECTION('center_axis',(1.,0.,0.));
#22351=DIRECTION('ref_axis',(0.,1.,0.));
#22352=DIRECTION('',(-1.,0.,0.));
#22353=DIRECTION('center_axis',(1.,0.,0.));
#22354=DIRECTION('ref_axis',(0.,1.,0.));
#22355=DIRECTION('',(-1.,0.,0.));
#22356=DIRECTION('center_axis',(1.,0.,0.));
#22357=DIRECTION('ref_axis',(0.,1.,0.));
#22358=DIRECTION('',(-1.,0.,0.));
#22359=DIRECTION('center_axis',(1.,0.,0.));
#22360=DIRECTION('ref_axis',(0.,1.,0.));
#22361=DIRECTION('',(-1.,0.,0.));
#22362=DIRECTION('center_axis',(1.,0.,0.));
#22363=DIRECTION('ref_axis',(0.,1.,0.));
#22364=DIRECTION('',(-1.,0.,0.));
#22365=DIRECTION('center_axis',(1.,0.,0.));
#22366=DIRECTION('ref_axis',(0.,1.,0.));
#22367=DIRECTION('',(-1.,0.,0.));
#22368=DIRECTION('center_axis',(1.,0.,0.));
#22369=DIRECTION('ref_axis',(0.,1.,0.));
#22370=DIRECTION('',(-1.,0.,0.));
#22371=DIRECTION('center_axis',(1.,0.,0.));
#22372=DIRECTION('ref_axis',(0.,1.,0.));
#22373=DIRECTION('',(-1.,0.,0.));
#22374=DIRECTION('center_axis',(1.,0.,0.));
#22375=DIRECTION('ref_axis',(0.,1.,0.));
#22376=DIRECTION('',(-1.,0.,0.));
#22377=DIRECTION('center_axis',(1.,0.,0.));
#22378=DIRECTION('ref_axis',(0.,1.,0.));
#22379=DIRECTION('',(-1.,0.,0.));
#22380=DIRECTION('center_axis',(1.,0.,0.));
#22381=DIRECTION('ref_axis',(0.,1.,0.));
#22382=DIRECTION('',(-1.,0.,0.));
#22383=DIRECTION('center_axis',(1.,0.,0.));
#22384=DIRECTION('ref_axis',(0.,1.,0.));
#22385=DIRECTION('',(-1.,0.,0.));
#22386=DIRECTION('center_axis',(1.,0.,0.));
#22387=DIRECTION('ref_axis',(0.,1.,0.));
#22388=DIRECTION('',(-1.,0.,0.));
#22389=DIRECTION('center_axis',(1.,0.,0.));
#22390=DIRECTION('ref_axis',(0.,1.,0.));
#22391=DIRECTION('',(-1.,0.,0.));
#22392=DIRECTION('center_axis',(1.,0.,0.));
#22393=DIRECTION('ref_axis',(0.,1.,-1.69495320649391E-12));
#22394=DIRECTION('',(1.,0.,0.));
#22395=DIRECTION('center_axis',(1.,0.,0.));
#22396=DIRECTION('ref_axis',(0.,1.,-1.69495320649391E-12));
#22397=DIRECTION('center_axis',(1.,0.,0.));
#22398=DIRECTION('ref_axis',(0.,1.,-1.69495320649391E-12));
#22399=DIRECTION('',(1.,0.,0.));
#22400=DIRECTION('center_axis',(1.,0.,0.));
#22401=DIRECTION('ref_axis',(0.,1.,-1.69495320649391E-12));
#22402=DIRECTION('center_axis',(1.,0.,0.));
#22403=DIRECTION('ref_axis',(0.,1.,-1.69495320649391E-12));
#22404=DIRECTION('',(1.,0.,0.));
#22405=DIRECTION('center_axis',(1.,0.,0.));
#22406=DIRECTION('ref_axis',(0.,1.,-1.69495320649391E-12));
#22407=DIRECTION('',(1.,0.,0.));
#22408=DIRECTION('center_axis',(1.,0.,0.));
#22409=DIRECTION('ref_axis',(0.,1.,-1.69495320649391E-12));
#22410=DIRECTION('',(1.,0.,0.));
#22411=DIRECTION('center_axis',(1.,0.,0.));
#22412=DIRECTION('ref_axis',(0.,1.,-1.69495320649391E-12));
#22413=DIRECTION('',(1.,0.,0.));
#22414=DIRECTION('center_axis',(1.,0.,0.));
#22415=DIRECTION('ref_axis',(0.,1.,-1.69495320649391E-12));
#22416=DIRECTION('',(1.,0.,0.));
#22417=DIRECTION('center_axis',(1.,0.,0.));
#22418=DIRECTION('ref_axis',(0.,1.,-1.69495320649391E-12));
#22419=DIRECTION('',(1.,0.,0.));
#22420=DIRECTION('center_axis',(1.,0.,0.));
#22421=DIRECTION('ref_axis',(0.,1.,-1.69495320649391E-12));
#22422=DIRECTION('',(1.,0.,0.));
#22423=DIRECTION('center_axis',(1.,0.,0.));
#22424=DIRECTION('ref_axis',(0.,1.,-1.69495320649391E-12));
#22425=DIRECTION('',(1.,0.,0.));
#22426=DIRECTION('center_axis',(1.,0.,0.));
#22427=DIRECTION('ref_axis',(0.,1.,-1.69495320649391E-12));
#22428=DIRECTION('',(1.,0.,0.));
#22429=DIRECTION('center_axis',(1.,0.,0.));
#22430=DIRECTION('ref_axis',(0.,1.,-1.69495320649391E-12));
#22431=DIRECTION('',(1.,0.,0.));
#22432=DIRECTION('center_axis',(1.,0.,0.));
#22433=DIRECTION('ref_axis',(0.,1.,-1.69495320649391E-12));
#22434=DIRECTION('',(1.,0.,0.));
#22435=DIRECTION('center_axis',(1.,0.,0.));
#22436=DIRECTION('ref_axis',(0.,1.,-1.69495320649391E-12));
#22437=DIRECTION('',(1.,0.,0.));
#22438=DIRECTION('center_axis',(1.,0.,0.));
#22439=DIRECTION('ref_axis',(0.,1.,-1.69495320649391E-12));
#22440=DIRECTION('',(1.,0.,0.));
#22441=DIRECTION('center_axis',(1.,0.,0.));
#22442=DIRECTION('ref_axis',(0.,1.,-1.69495320649391E-12));
#22443=DIRECTION('',(1.,0.,0.));
#22444=DIRECTION('center_axis',(1.,0.,0.));
#22445=DIRECTION('ref_axis',(0.,1.,-1.69495320649391E-12));
#22446=DIRECTION('',(1.,0.,0.));
#22447=DIRECTION('center_axis',(1.,0.,0.));
#22448=DIRECTION('ref_axis',(0.,1.,-1.69495320649391E-12));
#22449=DIRECTION('',(1.,0.,0.));
#22450=DIRECTION('center_axis',(1.,0.,0.));
#22451=DIRECTION('ref_axis',(0.,1.,-1.69495320649391E-12));
#22452=DIRECTION('',(1.,0.,0.));
#22453=DIRECTION('center_axis',(1.,0.,0.));
#22454=DIRECTION('ref_axis',(0.,1.,-1.69495320649391E-12));
#22455=DIRECTION('',(1.,0.,0.));
#22456=DIRECTION('center_axis',(1.,0.,0.));
#22457=DIRECTION('ref_axis',(0.,1.,-1.69495320649391E-12));
#22458=DIRECTION('',(1.,0.,0.));
#22459=DIRECTION('center_axis',(1.,0.,0.));
#22460=DIRECTION('ref_axis',(0.,1.,-1.69495320649391E-12));
#22461=DIRECTION('',(1.,0.,0.));
#22462=DIRECTION('center_axis',(1.,0.,0.));
#22463=DIRECTION('ref_axis',(0.,1.,-1.69495320649391E-12));
#22464=DIRECTION('',(1.,0.,0.));
#22465=DIRECTION('center_axis',(1.,0.,0.));
#22466=DIRECTION('ref_axis',(0.,1.,-1.69495320649391E-12));
#22467=DIRECTION('',(1.,0.,0.));
#22468=DIRECTION('center_axis',(1.,0.,0.));
#22469=DIRECTION('ref_axis',(0.,1.,-1.69495320649391E-12));
#22470=DIRECTION('',(1.,0.,0.));
#22471=DIRECTION('center_axis',(1.,0.,0.));
#22472=DIRECTION('ref_axis',(0.,1.,-1.69495320649391E-12));
#22473=DIRECTION('',(1.,0.,0.));
#22474=DIRECTION('center_axis',(1.,0.,0.));
#22475=DIRECTION('ref_axis',(0.,1.,-1.69495320649391E-12));
#22476=DIRECTION('',(1.,0.,0.));
#22477=DIRECTION('center_axis',(1.,0.,0.));
#22478=DIRECTION('ref_axis',(0.,1.,-1.69495320649391E-12));
#22479=DIRECTION('',(1.,0.,0.));
#22480=DIRECTION('center_axis',(1.,0.,0.));
#22481=DIRECTION('ref_axis',(0.,1.,-1.69495320649391E-12));
#22482=DIRECTION('',(1.,0.,0.));
#22483=DIRECTION('center_axis',(1.,0.,0.));
#22484=DIRECTION('ref_axis',(0.,1.,-1.69495320649391E-12));
#22485=DIRECTION('',(1.,0.,0.));
#22486=DIRECTION('center_axis',(1.,0.,0.));
#22487=DIRECTION('ref_axis',(0.,1.,-1.69495320649391E-12));
#22488=DIRECTION('',(1.,0.,0.));
#22489=DIRECTION('center_axis',(1.,0.,0.));
#22490=DIRECTION('ref_axis',(0.,1.,-1.69495320649391E-12));
#22491=DIRECTION('',(1.,0.,0.));
#22492=DIRECTION('center_axis',(1.,0.,0.));
#22493=DIRECTION('ref_axis',(0.,1.,-1.69495320649391E-12));
#22494=DIRECTION('',(1.,0.,0.));
#22495=DIRECTION('center_axis',(1.,0.,0.));
#22496=DIRECTION('ref_axis',(0.,1.,-1.69495320649391E-12));
#22497=DIRECTION('',(1.,0.,0.));
#22498=DIRECTION('center_axis',(1.,0.,0.));
#22499=DIRECTION('ref_axis',(0.,1.,-1.69495320649391E-12));
#22500=DIRECTION('',(1.,0.,0.));
#22501=DIRECTION('center_axis',(1.,0.,0.));
#22502=DIRECTION('ref_axis',(0.,1.,-1.69495320649391E-12));
#22503=DIRECTION('',(1.,0.,0.));
#22504=DIRECTION('center_axis',(1.,0.,0.));
#22505=DIRECTION('ref_axis',(0.,1.,-1.69495320649391E-12));
#22506=DIRECTION('',(1.,0.,0.));
#22507=DIRECTION('center_axis',(1.,0.,0.));
#22508=DIRECTION('ref_axis',(0.,1.,-1.69495320649391E-12));
#22509=DIRECTION('',(1.,0.,0.));
#22510=DIRECTION('center_axis',(1.,0.,0.));
#22511=DIRECTION('ref_axis',(0.,1.,-1.69495320649391E-12));
#22512=DIRECTION('',(1.,0.,0.));
#22513=DIRECTION('center_axis',(1.,0.,0.));
#22514=DIRECTION('ref_axis',(0.,1.,-1.69495320649391E-12));
#22515=DIRECTION('',(1.,0.,0.));
#22516=DIRECTION('center_axis',(1.,0.,0.));
#22517=DIRECTION('ref_axis',(0.,1.,-1.69495320649391E-12));
#22518=DIRECTION('',(1.,0.,0.));
#22519=DIRECTION('center_axis',(1.,0.,0.));
#22520=DIRECTION('ref_axis',(0.,1.,-1.69495320649391E-12));
#22521=DIRECTION('',(1.,0.,0.));
#22522=DIRECTION('center_axis',(1.,0.,0.));
#22523=DIRECTION('ref_axis',(0.,1.,-1.69495320649391E-12));
#22524=DIRECTION('',(1.,0.,0.));
#22525=DIRECTION('center_axis',(1.,0.,0.));
#22526=DIRECTION('ref_axis',(0.,1.,-1.69495320649391E-12));
#22527=DIRECTION('',(1.,0.,0.));
#22528=DIRECTION('center_axis',(1.,0.,0.));
#22529=DIRECTION('ref_axis',(0.,1.,-1.69495320649391E-12));
#22530=DIRECTION('',(1.,0.,0.));
#22531=DIRECTION('center_axis',(1.,0.,0.));
#22532=DIRECTION('ref_axis',(0.,1.,-1.69495320649391E-12));
#22533=DIRECTION('',(1.,0.,0.));
#22534=DIRECTION('center_axis',(1.,0.,0.));
#22535=DIRECTION('ref_axis',(0.,1.,-1.69495320649391E-12));
#22536=DIRECTION('',(1.,0.,0.));
#22537=DIRECTION('center_axis',(1.,0.,0.));
#22538=DIRECTION('ref_axis',(0.,1.,-1.69495320649391E-12));
#22539=DIRECTION('',(1.,0.,0.));
#22540=DIRECTION('center_axis',(1.,0.,0.));
#22541=DIRECTION('ref_axis',(0.,1.,-1.69495320649391E-12));
#22542=DIRECTION('',(1.,0.,0.));
#22543=DIRECTION('center_axis',(1.,0.,0.));
#22544=DIRECTION('ref_axis',(0.,1.,-1.69495320649391E-12));
#22545=DIRECTION('',(1.,0.,0.));
#22546=DIRECTION('center_axis',(1.,0.,0.));
#22547=DIRECTION('ref_axis',(0.,1.,-1.69495320649391E-12));
#22548=DIRECTION('',(1.,0.,0.));
#22549=DIRECTION('center_axis',(1.,0.,0.));
#22550=DIRECTION('ref_axis',(0.,1.,-1.69495320649391E-12));
#22551=DIRECTION('',(1.,0.,0.));
#22552=DIRECTION('center_axis',(1.,0.,0.));
#22553=DIRECTION('ref_axis',(0.,1.,-1.69495320649391E-12));
#22554=DIRECTION('',(1.,0.,0.));
#22555=DIRECTION('center_axis',(1.,0.,0.));
#22556=DIRECTION('ref_axis',(0.,1.,-1.69495320649391E-12));
#22557=DIRECTION('',(1.,0.,0.));
#22558=DIRECTION('center_axis',(1.,0.,0.));
#22559=DIRECTION('ref_axis',(0.,1.,-1.69495320649391E-12));
#22560=DIRECTION('',(1.,0.,0.));
#22561=DIRECTION('center_axis',(1.,0.,0.));
#22562=DIRECTION('ref_axis',(0.,1.,-1.69495320649391E-12));
#22563=DIRECTION('',(1.,0.,0.));
#22564=DIRECTION('center_axis',(1.,0.,0.));
#22565=DIRECTION('ref_axis',(0.,1.,-1.69495320649391E-12));
#22566=DIRECTION('',(1.,0.,0.));
#22567=DIRECTION('center_axis',(1.,0.,0.));
#22568=DIRECTION('ref_axis',(0.,1.,-1.69495320649391E-12));
#22569=DIRECTION('',(1.,0.,0.));
#22570=DIRECTION('center_axis',(1.,0.,0.));
#22571=DIRECTION('ref_axis',(0.,1.,-1.69495320649391E-12));
#22572=DIRECTION('',(1.,0.,0.));
#22573=DIRECTION('center_axis',(1.,0.,0.));
#22574=DIRECTION('ref_axis',(0.,1.,-1.69495320649391E-12));
#22575=DIRECTION('',(1.,0.,0.));
#22576=DIRECTION('center_axis',(1.,0.,0.));
#22577=DIRECTION('ref_axis',(0.,1.,-1.69495320649391E-12));
#22578=DIRECTION('',(1.,0.,0.));
#22579=DIRECTION('center_axis',(1.,0.,0.));
#22580=DIRECTION('ref_axis',(0.,1.,-1.69495320649391E-12));
#22581=DIRECTION('',(1.,0.,0.));
#22582=DIRECTION('center_axis',(1.,0.,0.));
#22583=DIRECTION('ref_axis',(0.,1.,-1.69495320649391E-12));
#22584=DIRECTION('',(1.,0.,0.));
#22585=DIRECTION('center_axis',(1.,0.,0.));
#22586=DIRECTION('ref_axis',(0.,1.,-1.69495320649391E-12));
#22587=DIRECTION('',(1.,0.,0.));
#22588=DIRECTION('center_axis',(1.,0.,0.));
#22589=DIRECTION('ref_axis',(0.,1.,-1.69495320649391E-12));
#22590=DIRECTION('',(1.,0.,0.));
#22591=DIRECTION('center_axis',(1.,0.,0.));
#22592=DIRECTION('ref_axis',(0.,1.,-1.69495320649391E-12));
#22593=DIRECTION('',(1.,0.,0.));
#22594=DIRECTION('center_axis',(1.,0.,0.));
#22595=DIRECTION('ref_axis',(0.,1.,-1.69495320649391E-12));
#22596=DIRECTION('',(1.,0.,0.));
#22597=DIRECTION('center_axis',(1.,0.,0.));
#22598=DIRECTION('ref_axis',(0.,1.,-1.69495320649391E-12));
#22599=DIRECTION('',(1.,0.,0.));
#22600=DIRECTION('center_axis',(1.,0.,0.));
#22601=DIRECTION('ref_axis',(0.,1.,-1.69495320649391E-12));
#22602=DIRECTION('',(1.,0.,0.));
#22603=DIRECTION('center_axis',(1.,0.,0.));
#22604=DIRECTION('ref_axis',(0.,1.,-1.69495320649391E-12));
#22605=DIRECTION('',(1.,0.,0.));
#22606=DIRECTION('center_axis',(1.,0.,0.));
#22607=DIRECTION('ref_axis',(0.,1.,-1.69495320649391E-12));
#22608=DIRECTION('',(1.,0.,0.));
#22609=DIRECTION('center_axis',(1.,0.,0.));
#22610=DIRECTION('ref_axis',(0.,1.,-1.69495320649391E-12));
#22611=DIRECTION('',(1.,0.,0.));
#22612=DIRECTION('center_axis',(1.,0.,0.));
#22613=DIRECTION('ref_axis',(0.,1.,-1.69495320649391E-12));
#22614=DIRECTION('',(1.,0.,0.));
#22615=DIRECTION('center_axis',(1.,0.,0.));
#22616=DIRECTION('ref_axis',(0.,1.,-1.69495320649391E-12));
#22617=DIRECTION('',(1.,0.,0.));
#22618=DIRECTION('center_axis',(1.,0.,0.));
#22619=DIRECTION('ref_axis',(0.,1.,-1.69495320649391E-12));
#22620=DIRECTION('',(1.,0.,0.));
#22621=DIRECTION('center_axis',(1.,0.,0.));
#22622=DIRECTION('ref_axis',(0.,1.,-1.69495320649391E-12));
#22623=DIRECTION('',(1.,0.,0.));
#22624=DIRECTION('center_axis',(1.,0.,0.));
#22625=DIRECTION('ref_axis',(0.,1.,-1.69495320649391E-12));
#22626=DIRECTION('',(1.,0.,0.));
#22627=DIRECTION('center_axis',(1.,0.,0.));
#22628=DIRECTION('ref_axis',(0.,1.,-1.69495320649391E-12));
#22629=DIRECTION('',(1.,0.,0.));
#22630=DIRECTION('center_axis',(1.,0.,0.));
#22631=DIRECTION('ref_axis',(0.,1.,-1.69495320649391E-12));
#22632=DIRECTION('',(1.,0.,0.));
#22633=DIRECTION('center_axis',(1.,0.,0.));
#22634=DIRECTION('ref_axis',(0.,1.,-1.69495320649391E-12));
#22635=DIRECTION('',(1.,0.,0.));
#22636=DIRECTION('center_axis',(1.,0.,0.));
#22637=DIRECTION('ref_axis',(0.,1.,-1.69495320649391E-12));
#22638=DIRECTION('',(1.,0.,0.));
#22639=DIRECTION('center_axis',(1.,0.,0.));
#22640=DIRECTION('ref_axis',(0.,1.,-1.69495320649391E-12));
#22641=DIRECTION('',(1.,0.,0.));
#22642=DIRECTION('center_axis',(1.,0.,0.));
#22643=DIRECTION('ref_axis',(0.,1.,-1.69495320649391E-12));
#22644=DIRECTION('',(1.,0.,0.));
#22645=DIRECTION('center_axis',(1.,0.,0.));
#22646=DIRECTION('ref_axis',(0.,1.,-1.69495320649391E-12));
#22647=DIRECTION('',(1.,0.,0.));
#22648=DIRECTION('center_axis',(1.,0.,0.));
#22649=DIRECTION('ref_axis',(0.,1.,-1.69495320649391E-12));
#22650=DIRECTION('',(1.,0.,0.));
#22651=DIRECTION('center_axis',(1.,0.,0.));
#22652=DIRECTION('ref_axis',(0.,1.,-1.69495320649391E-12));
#22653=DIRECTION('',(1.,0.,0.));
#22654=DIRECTION('center_axis',(1.,0.,0.));
#22655=DIRECTION('ref_axis',(0.,1.,-1.69495320649391E-12));
#22656=DIRECTION('',(1.,0.,0.));
#22657=DIRECTION('center_axis',(1.,0.,0.));
#22658=DIRECTION('ref_axis',(0.,1.,-1.69495320649391E-12));
#22659=DIRECTION('',(1.,0.,0.));
#22660=DIRECTION('center_axis',(1.,0.,0.));
#22661=DIRECTION('ref_axis',(0.,0.,-1.));
#22662=DIRECTION('center_axis',(1.,0.,0.));
#22663=DIRECTION('ref_axis',(0.,1.,0.));
#22664=DIRECTION('center_axis',(1.,0.,0.));
#22665=DIRECTION('ref_axis',(0.,1.,0.));
#22666=DIRECTION('center_axis',(-1.,0.,0.));
#22667=DIRECTION('ref_axis',(0.,1.,-1.69495320649391E-12));
#22668=DIRECTION('center_axis',(1.,0.,0.));
#22669=DIRECTION('ref_axis',(0.,1.,-1.69495320649391E-12));
#22670=DIRECTION('center_axis',(-1.,0.,0.));
#22671=DIRECTION('ref_axis',(0.,1.,0.));
#22672=DIRECTION('',(0.500490667348524,0.865741931465162,1.06022808525646E-16));
#22673=DIRECTION('center_axis',(1.,0.,0.));
#22674=DIRECTION('ref_axis',(0.,1.,0.));
#22675=DIRECTION('center_axis',(0.,-0.5,0.866025403784439));
#22676=DIRECTION('ref_axis',(0.,-0.866025403784439,-0.5));
#22677=DIRECTION('',(1.,0.,0.));
#22678=DIRECTION('',(0.,-0.866025403784439,-0.5));
#22679=DIRECTION('',(1.,0.,0.));
#22680=DIRECTION('center_axis',(0.,0.5,0.866025403784439));
#22681=DIRECTION('ref_axis',(0.,-0.866025403784439,0.5));
#22682=DIRECTION('',(1.,0.,0.));
#22683=DIRECTION('',(0.,-0.866025403784439,0.5));
#22684=DIRECTION('center_axis',(0.,1.,-4.43760619934668E-16));
#22685=DIRECTION('ref_axis',(0.,4.43760619934668E-16,1.));
#22686=DIRECTION('',(1.,0.,0.));
#22687=DIRECTION('',(0.,4.43760619934668E-16,1.));
#22688=DIRECTION('center_axis',(1.,0.,0.));
#22689=DIRECTION('ref_axis',(0.,0.,-1.));
#22690=DIRECTION('',(0.,0.866025403784439,0.5));
#22691=DIRECTION('',(0.,0.866025403784439,-0.5));
#22692=DIRECTION('',(0.,1.4792020664489E-16,-1.));
#22693=DIRECTION('center_axis',(-1.,0.,0.));
#22694=DIRECTION('ref_axis',(0.,1.,0.));
#22695=DIRECTION('center_axis',(0.,0.5,-0.866025403784439));
#22696=DIRECTION('ref_axis',(0.,0.866025403784439,0.5));
#22697=DIRECTION('',(1.,0.,0.));
#22698=DIRECTION('center_axis',(0.,-0.5,-0.866025403784439));
#22699=DIRECTION('ref_axis',(0.,0.866025403784439,-0.5));
#22700=DIRECTION('',(1.,0.,0.));
#22701=DIRECTION('center_axis',(0.,-1.,-1.4792020664489E-16));
#22702=DIRECTION('ref_axis',(0.,1.4792020664489E-16,-1.));
#22703=DIRECTION('center_axis',(1.,0.,0.));
#22704=DIRECTION('ref_axis',(0.,0.,-1.));
#22705=DIRECTION('center_axis',(-1.,0.,0.));
#22706=DIRECTION('ref_axis',(0.,0.,1.));
#22707=DIRECTION('center_axis',(1.,0.,0.));
#22708=DIRECTION('ref_axis',(0.,0.,-1.));
#22709=DIRECTION('center_axis',(1.,0.,0.));
#22710=DIRECTION('ref_axis',(0.,1.,0.));
#22711=DIRECTION('',(-0.707106781186552,0.707106781186543,8.65956056235488E-17));
#22712=DIRECTION('center_axis',(1.,0.,0.));
#22713=DIRECTION('ref_axis',(0.,1.,0.));
#22714=DIRECTION('axis',(0.,0.,1.));
#22715=DIRECTION('refdir',(1.,0.,0.));
#22716=DIRECTION('center_axis',(-1.,0.,-2.9053353178063E-15));
#22717=DIRECTION('ref_axis',(0.,1.,3.18680589015166E-17));
#22718=DIRECTION('center_axis',(-1.,0.,0.));
#22719=DIRECTION('ref_axis',(0.,1.,0.));
#22720=DIRECTION('',(-0.259092713651731,-0.965852455467491,-9.01813866303348E-16));
#22721=DIRECTION('center_axis',(1.,0.,0.));
#22722=DIRECTION('ref_axis',(0.,1.,6.12323399573677E-17));
#22723=DIRECTION('center_axis',(1.,0.,0.));
#22724=DIRECTION('ref_axis',(0.,1.,6.12323399573677E-17));
#22725=DIRECTION('center_axis',(1.,0.,0.));
#22726=DIRECTION('ref_axis',(0.,1.,6.12323399573677E-17));
#22727=DIRECTION('center_axis',(1.,0.,0.));
#22728=DIRECTION('ref_axis',(0.,1.,6.12323399573677E-17));
#22729=DIRECTION('center_axis',(1.,0.,0.));
#22730=DIRECTION('ref_axis',(0.,1.,6.12323399573677E-17));
#22731=DIRECTION('center_axis',(1.,0.,0.));
#22732=DIRECTION('ref_axis',(0.,1.,6.12323399573677E-17));
#22733=DIRECTION('center_axis',(-1.,0.,0.));
#22734=DIRECTION('ref_axis',(0.,1.,0.));
#22735=DIRECTION('center_axis',(-1.,0.,0.));
#22736=DIRECTION('ref_axis',(0.,1.,0.));
#22737=DIRECTION('center_axis',(-1.,0.,0.));
#22738=DIRECTION('ref_axis',(0.,1.,0.));
#22739=DIRECTION('center_axis',(-1.,0.,0.));
#22740=DIRECTION('ref_axis',(0.,1.,0.));
#22741=DIRECTION('center_axis',(-1.,0.,0.));
#22742=DIRECTION('ref_axis',(0.,1.,0.));
#22743=DIRECTION('center_axis',(-1.,0.,0.));
#22744=DIRECTION('ref_axis',(0.,1.,0.));
#22745=DIRECTION('center_axis',(1.,0.,0.));
#22746=DIRECTION('ref_axis',(0.,0.,-1.));
#22747=DIRECTION('center_axis',(-1.,0.,0.));
#22748=DIRECTION('ref_axis',(0.,1.,0.));
#22749=DIRECTION('center_axis',(0.369302787980288,0.804805310675672,-0.46465456276488));
#22750=DIRECTION('ref_axis',(-0.78285445475425,0.,-0.622204871944464));
#22751=DIRECTION('',(-1.04457232346762E-13,-0.499999999999998,-0.86602540378444));
#22752=DIRECTION('center_axis',(0.369302787980293,-9.03801697827166E-13,
-0.929309125528197));
#22753=DIRECTION('ref_axis',(-0.929309125528197,0.,-0.369302787980293));
#22754=DIRECTION('',(-1.06831260354642E-13,-1.,0.));
#22755=DIRECTION('center_axis',(0.369302787980294,0.804805310676573,0.464654562763313));
#22756=DIRECTION('ref_axis',(0.782854454753223,0.,-0.622204871945755));
#22757=DIRECTION('',(-1.06831260354642E-13,0.500000000000001,-0.866025403784438));
#22758=DIRECTION('center_axis',(0.369302787980299,-0.804805310676573,-0.464654562763311));
#22759=DIRECTION('ref_axis',(-0.782854454753218,0.,-0.622204871945762));
#22760=DIRECTION('',(-9.73351483231188E-14,-0.499999999999998,0.86602540378444));
#22761=DIRECTION('center_axis',(0.369302787980296,9.02065506036524E-13,
0.929309125528196));
#22762=DIRECTION('ref_axis',(0.929309125528196,0.,-0.369302787980296));
#22763=DIRECTION('',(-1.02083204338881E-13,1.,0.));
#22764=DIRECTION('center_axis',(0.369302787980293,-0.804805310675669,0.464654562764882));
#22765=DIRECTION('ref_axis',(0.782854454754247,0.,-0.622204871944466));
#22766=DIRECTION('',(-1.04457232346761E-13,0.500000000000001,0.866025403784438));
#22767=DIRECTION('center_axis',(0.,-0.866025403784438,0.500000000000001));
#22768=DIRECTION('ref_axis',(1.,0.,0.));
#22769=DIRECTION('',(1.,0.,0.));
#22770=DIRECTION('',(-1.,0.,0.));
#22771=DIRECTION('center_axis',(0.,0.,1.));
#22772=DIRECTION('ref_axis',(1.,0.,0.));
#22773=DIRECTION('',(1.,0.,0.));
#22774=DIRECTION('',(-1.,0.,0.));
#22775=DIRECTION('center_axis',(0.,-0.86602540378444,-0.499999999999998));
#22776=DIRECTION('ref_axis',(0.,0.499999999999998,-0.86602540378444));
#22777=DIRECTION('',(1.,0.,0.));
#22778=DIRECTION('',(-1.,0.,0.));
#22779=DIRECTION('center_axis',(0.,0.866025403784438,0.500000000000001));
#22780=DIRECTION('ref_axis',(1.,0.,0.));
#22781=DIRECTION('',(1.,0.,0.));
#22782=DIRECTION('',(-1.,0.,0.));
#22783=DIRECTION('center_axis',(0.,0.,-1.));
#22784=DIRECTION('ref_axis',(-1.,0.,0.));
#22785=DIRECTION('',(1.,0.,0.));
#22786=DIRECTION('',(-1.,0.,0.));
#22787=DIRECTION('center_axis',(0.,0.86602540378444,-0.499999999999998));
#22788=DIRECTION('ref_axis',(0.,0.499999999999998,0.86602540378444));
#22789=DIRECTION('',(1.,0.,0.));
#22790=DIRECTION('',(-1.,0.,0.));
#22791=DIRECTION('center_axis',(0.,0.5,0.866025403784439));
#22792=DIRECTION('ref_axis',(0.,-0.866025403784439,0.5));
#22793=DIRECTION('center_axis',(0.,1.,-4.43760619934668E-16));
#22794=DIRECTION('ref_axis',(0.,4.43760619934668E-16,1.));
#22795=DIRECTION('center_axis',(0.,0.5,-0.866025403784439));
#22796=DIRECTION('ref_axis',(0.,0.866025403784439,0.5));
#22797=DIRECTION('center_axis',(1.,0.,0.));
#22798=DIRECTION('ref_axis',(0.,1.,0.));
#22799=DIRECTION('center_axis',(-1.,0.,0.));
#22800=DIRECTION('ref_axis',(0.,1.,0.));
#22801=DIRECTION('',(0.500490667348524,-0.865741931465162,-1.06022808525646E-16));
#22802=DIRECTION('center_axis',(-1.,0.,0.));
#22803=DIRECTION('ref_axis',(0.,1.,0.));
#22804=DIRECTION('center_axis',(1.,0.,0.));
#22805=DIRECTION('ref_axis',(0.,1.,0.));
#22806=DIRECTION('',(0.78086880944303,0.624695047554425,7.6503079043073E-17));
#22807=DIRECTION('center_axis',(1.,0.,0.));
#22808=DIRECTION('ref_axis',(0.,0.,-1.));
#22809=DIRECTION('center_axis',(1.,0.,0.));
#22810=DIRECTION('ref_axis',(0.,1.,0.));
#22811=DIRECTION('',(1.,0.,0.));
#22812=DIRECTION('center_axis',(1.,0.,0.));
#22813=DIRECTION('ref_axis',(0.,0.,-1.));
#22814=DIRECTION('center_axis',(1.,0.,0.));
#22815=DIRECTION('ref_axis',(0.,1.,0.));
#22816=DIRECTION('',(0.78086880944303,-0.624695047554424,-7.65030790430729E-17));
#22817=DIRECTION('center_axis',(0.,-0.5,-0.866025403784439));
#22818=DIRECTION('ref_axis',(0.,0.866025403784439,-0.5));
#22819=DIRECTION('center_axis',(0.,-1.,-1.4792020664489E-16));
#22820=DIRECTION('ref_axis',(0.,1.4792020664489E-16,-1.));
#22821=DIRECTION('center_axis',(0.,-0.5,0.866025403784439));
#22822=DIRECTION('ref_axis',(0.,-0.866025403784439,-0.5));
#22823=DIRECTION('center_axis',(1.,0.,0.));
#22824=DIRECTION('ref_axis',(0.,0.,-1.));
#22825=DIRECTION('',(0.,0.,1.));
#22826=DIRECTION('',(1.,0.,0.));
#22827=DIRECTION('',(0.,0.,1.));
#22828=DIRECTION('',(-1.,0.,0.));
#22829=DIRECTION('',(0.,0.,1.));
#22830=DIRECTION('',(1.,0.,0.));
#22831=DIRECTION('',(0.,0.,1.));
#22832=DIRECTION('',(1.,0.,0.));
#22833=DIRECTION('',(0.,0.,1.));
#22834=DIRECTION('',(1.,0.,0.));
#22835=DIRECTION('',(0.,0.,1.));
#22836=DIRECTION('',(1.,0.,0.));
#22837=DIRECTION('',(0.,0.,1.));
#22838=DIRECTION('',(-1.,0.,0.));
#22839=DIRECTION('',(0.,0.,1.));
#22840=DIRECTION('',(1.,0.,0.));
#22841=DIRECTION('',(0.,0.,1.));
#22842=DIRECTION('',(-1.,0.,0.));
#22843=DIRECTION('',(0.,0.,1.));
#22844=DIRECTION('',(1.,0.,0.));
#22845=DIRECTION('',(0.,0.,1.));
#22846=DIRECTION('',(-1.,0.,0.));
#22847=DIRECTION('',(0.,0.,1.));
#22848=DIRECTION('',(1.,0.,0.));
#22849=DIRECTION('',(0.,0.,1.));
#22850=DIRECTION('',(1.,0.,0.));
#22851=DIRECTION('',(0.,0.,1.));
#22852=DIRECTION('',(-1.,0.,0.));
#22853=DIRECTION('',(0.,0.,1.));
#22854=DIRECTION('',(1.,0.,0.));
#22855=DIRECTION('',(0.,0.,-1.));
#22856=DIRECTION('',(1.,0.,0.));
#22857=DIRECTION('',(0.,0.,1.));
#22858=DIRECTION('',(1.,0.,0.));
#22859=DIRECTION('',(0.,0.,-1.));
#22860=DIRECTION('',(1.,0.,0.));
#22861=DIRECTION('',(0.,0.,1.));
#22862=DIRECTION('',(1.,0.,0.));
#22863=DIRECTION('',(0.,0.,1.));
#22864=DIRECTION('',(1.,0.,0.));
#22865=DIRECTION('',(0.,0.,1.));
#22866=DIRECTION('',(1.,0.,0.));
#22867=DIRECTION('',(0.,0.,1.));
#22868=DIRECTION('',(1.,0.,0.));
#22869=DIRECTION('',(-1.,0.,0.));
#22870=DIRECTION('',(0.,0.,1.));
#22871=DIRECTION('',(-1.,0.,0.));
#22872=DIRECTION('',(0.,0.,1.));
#22873=DIRECTION('',(0.,0.,1.));
#22874=DIRECTION('',(1.,0.,0.));
#22875=DIRECTION('',(-1.,0.,0.));
#22876=DIRECTION('',(0.,0.,1.));
#22877=DIRECTION('',(0.,1.,0.));
#22878=DIRECTION('',(0.,0.,1.));
#22879=DIRECTION('',(-1.,0.,0.));
#22880=DIRECTION('',(0.,0.,1.));
#22881=DIRECTION('',(0.,1.,0.));
#22882=DIRECTION('',(0.,0.,1.));
#22883=DIRECTION('',(1.,0.,0.));
#22884=DIRECTION('',(0.,0.,-1.));
#22885=DIRECTION('',(-1.,0.,0.));
#22886=DIRECTION('',(0.,0.,1.));
#22887=DIRECTION('',(1.,0.,0.));
#22888=DIRECTION('',(0.,0.,-1.));
#22889=DIRECTION('',(-1.,0.,0.));
#22890=DIRECTION('',(0.,0.,1.));
#22891=DIRECTION('',(0.,0.,1.));
#22892=DIRECTION('',(1.,0.,0.));
#22893=DIRECTION('',(0.,0.,1.));
#22894=DIRECTION('',(1.,0.,0.));
#22895=DIRECTION('',(-1.,0.,0.));
#22896=DIRECTION('',(0.,0.,1.));
#22897=DIRECTION('',(-1.,0.,0.));
#22898=DIRECTION('',(0.,0.,1.));
#22899=DIRECTION('',(0.,0.,1.));
#22900=DIRECTION('',(-1.,0.,0.));
#22901=DIRECTION('',(-1.,0.,0.));
#22902=DIRECTION('',(0.,0.,1.));
#22903=DIRECTION('',(0.,1.,0.));
#22904=DIRECTION('',(0.,0.,1.));
#22905=DIRECTION('',(-1.,0.,0.));
#22906=DIRECTION('',(0.,0.,1.));
#22907=DIRECTION('',(0.,1.,0.));
#22908=DIRECTION('',(0.,0.,1.));
#22909=DIRECTION('',(1.,0.,0.));
#22910=DIRECTION('',(0.,0.,-1.));
#22911=DIRECTION('',(-1.,0.,0.));
#22912=DIRECTION('',(0.,0.,1.));
#22913=DIRECTION('',(1.,0.,0.));
#22914=DIRECTION('',(0.,0.,-1.));
#22915=DIRECTION('',(-1.,0.,0.));
#22916=DIRECTION('',(0.,0.,1.));
#22917=DIRECTION('',(0.,0.,-1.));
#22918=DIRECTION('',(-1.,0.,0.));
#22919=DIRECTION('',(0.,0.,1.));
#22920=DIRECTION('',(1.,0.,0.));
#22921=DIRECTION('',(0.,0.,-1.));
#22922=DIRECTION('',(-1.,0.,0.));
#22923=DIRECTION('',(0.,0.,1.));
#22924=DIRECTION('',(1.,0.,0.));
#22925=DIRECTION('',(0.,0.,-1.));
#22926=DIRECTION('',(-1.,0.,0.));
#22927=DIRECTION('',(0.,0.,1.));
#22928=DIRECTION('',(1.,0.,0.));
#22929=DIRECTION('',(0.,0.,-1.));
#22930=DIRECTION('',(-1.,0.,0.));
#22931=DIRECTION('',(0.,0.,1.));
#22932=DIRECTION('',(1.,0.,0.));
#22933=DIRECTION('',(0.,0.,-1.));
#22934=DIRECTION('',(-1.,0.,0.));
#22935=DIRECTION('',(0.,0.,1.));
#22936=DIRECTION('',(1.,0.,0.));
#22937=DIRECTION('',(0.,0.,-1.));
#22938=DIRECTION('',(-1.,0.,0.));
#22939=DIRECTION('',(0.,0.,1.));
#22940=DIRECTION('',(1.,0.,0.));
#22941=CARTESIAN_POINT('',(0.,0.,0.));
#22942=CARTESIAN_POINT('',(0.,0.,0.));
#22943=CARTESIAN_POINT('Origin',(58.2244456071868,21.8438037119117,-77.));
#22944=CARTESIAN_POINT('',(58.6696447864562,21.6876074238235,-65.));
#22945=CARTESIAN_POINT('',(57.7792464279174,22.,-63.8675394171604));
#22946=CARTESIAN_POINT('Ctrl Pts',(57.7792464279174,22.,-63.8675394171605));
#22947=CARTESIAN_POINT('Ctrl Pts',(58.0193269966195,21.9157687268541,-64.0396955883018));
#22948=CARTESIAN_POINT('Ctrl Pts',(58.2665499426558,21.8290315802033,-64.2476809249266));
#22949=CARTESIAN_POINT('Ctrl Pts',(58.509255456617,21.7438793558854,-64.5516946338151));
#22950=CARTESIAN_POINT('Ctrl Pts',(58.5797344225006,21.71915210262,-64.6587247347519));
#22951=CARTESIAN_POINT('Ctrl Pts',(58.6491007720389,21.6948152061911,-64.8305933389432));
#22952=CARTESIAN_POINT('Ctrl Pts',(58.6696447864562,21.6876074238235,-64.9218325844837));
#22953=CARTESIAN_POINT('Ctrl Pts',(58.6696447864562,21.6876074238235,-65.));
#22954=CARTESIAN_POINT('',(57.7792464279174,22.,-63.));
#22955=CARTESIAN_POINT('',(57.7792464279174,22.,-77.));
#22956=CARTESIAN_POINT('',(58.6696447864562,21.6876074238235,-63.));
#22957=CARTESIAN_POINT('',(58.9671340002075,21.5832345653413,-63.));
#22958=CARTESIAN_POINT('',(58.6696447864562,21.6876074238235,-77.));
#22959=CARTESIAN_POINT('Origin',(69.,22.,-77.));
#22960=CARTESIAN_POINT('',(64.2207535720826,22.,-63.));
#22961=CARTESIAN_POINT('',(65.,22.,-63.));
#22962=CARTESIAN_POINT('',(55.7461918573286,22.,-63.));
#22963=CARTESIAN_POINT('Ctrl Pts',(57.7792464279174,22.,-63.8675394171604));
#22964=CARTESIAN_POINT('Ctrl Pts',(57.7052026398309,22.,-63.7886699029518));
#22965=CARTESIAN_POINT('Ctrl Pts',(57.6267561335641,22.,-63.716205257488));
#22966=CARTESIAN_POINT('Ctrl Pts',(57.3122246076983,22.,-63.4558552064108));
#22967=CARTESIAN_POINT('Ctrl Pts',(56.9894234086433,22.,-63.274575087265));
#22968=CARTESIAN_POINT('Ctrl Pts',(56.4120540241133,22.,-63.0659599554099));
#22969=CARTESIAN_POINT('Ctrl Pts',(56.0515769235887,22.,-63.));
#22970=CARTESIAN_POINT('Ctrl Pts',(55.7461918573286,22.,-63.));
#22971=CARTESIAN_POINT('',(53.,22.,-63.));
#22972=CARTESIAN_POINT('',(65.,22.,-63.));
#22973=CARTESIAN_POINT('',(53.,22.,-46.8343975045693));
#22974=CARTESIAN_POINT('',(53.,22.,-77.));
#22975=CARTESIAN_POINT('',(69.,22.,-41.8486611264283));
#22976=CARTESIAN_POINT('Ctrl Pts',(69.,22.,-41.8486611264284));
#22977=CARTESIAN_POINT('Ctrl Pts',(61.4497577287401,22.,-44.2291219194588));
#22978=CARTESIAN_POINT('Ctrl Pts',(53.,22.,-46.8343975045693));
#22979=CARTESIAN_POINT('',(69.,22.,-63.));
#22980=CARTESIAN_POINT('',(69.,22.,-77.));
#22981=CARTESIAN_POINT('',(66.2538081426714,22.,-63.));
#22982=CARTESIAN_POINT('',(65.,22.,-63.));
#22983=CARTESIAN_POINT('',(64.2207535720826,22.,-63.8675394171604));
#22984=CARTESIAN_POINT('Ctrl Pts',(66.2538081426714,22.,-63.));
#22985=CARTESIAN_POINT('Ctrl Pts',(65.9484230764113,22.,-63.));
#22986=CARTESIAN_POINT('Ctrl Pts',(65.5879459758867,22.,-63.0659599554099));
#22987=CARTESIAN_POINT('Ctrl Pts',(65.0105765913567,22.,-63.274575087265));
#22988=CARTESIAN_POINT('Ctrl Pts',(64.6877753923017,22.,-63.4558552064108));
#22989=CARTESIAN_POINT('Ctrl Pts',(64.3732438664359,22.,-63.716205257488));
#22990=CARTESIAN_POINT('Ctrl Pts',(64.2947973601691,22.,-63.7886699029518));
#22991=CARTESIAN_POINT('Ctrl Pts',(64.2207535720826,22.,-63.8675394171604));
#22992=CARTESIAN_POINT('',(64.2207535720826,22.,-77.));
#22993=CARTESIAN_POINT('Origin',(63.7755543928132,21.8438037119117,-77.));
#22994=CARTESIAN_POINT('',(63.3303552135438,21.6876074238235,-65.));
#22995=CARTESIAN_POINT('Ctrl Pts',(63.3303552135438,21.6876074238235,-65.));
#22996=CARTESIAN_POINT('Ctrl Pts',(63.3303552135438,21.6876074238235,-64.9218325844837));
#22997=CARTESIAN_POINT('Ctrl Pts',(63.3508992279611,21.6948152061911,-64.8305933389432));
#22998=CARTESIAN_POINT('Ctrl Pts',(63.4202655774994,21.71915210262,-64.6587247347519));
#22999=CARTESIAN_POINT('Ctrl Pts',(63.490744543383,21.7438793558854,-64.5516946338151));
#23000=CARTESIAN_POINT('Ctrl Pts',(63.7334500573442,21.8290315802033,-64.2476809249266));
#23001=CARTESIAN_POINT('Ctrl Pts',(63.9806730033805,21.9157687268541,-64.0396955883018));
#23002=CARTESIAN_POINT('Ctrl Pts',(64.2207535720826,22.,-63.8675394171604));
#23003=CARTESIAN_POINT('',(63.3303552135438,21.6876074238235,-63.));
#23004=CARTESIAN_POINT('',(63.3303552135438,21.6876074238235,-77.));
#23005=CARTESIAN_POINT('',(63.0328659997925,21.5832345653413,-63.));
#23006=CARTESIAN_POINT('Origin',(61.,25.,-77.));
#23007=CARTESIAN_POINT('',(56.95,25.,-76.5));
#23008=CARTESIAN_POINT('Origin',(61.,25.,-76.5));
#23009=CARTESIAN_POINT('',(56.95,25.,-65.));
#23010=CARTESIAN_POINT('',(56.95,25.,-77.));
#23011=CARTESIAN_POINT('Origin',(61.,25.,-65.));
#23012=CARTESIAN_POINT('Origin',(61.,25.,-63.));
#23013=CARTESIAN_POINT('Origin',(61.,25.,-65.));
#23014=CARTESIAN_POINT('Origin',(63.7755543928132,-21.8438037119117,-77.));
#23015=CARTESIAN_POINT('',(63.3303552135438,-21.6876074238235,-65.));
#23016=CARTESIAN_POINT('',(64.2207535720826,-22.,-63.8675394171604));
#23017=CARTESIAN_POINT('Ctrl Pts',(64.2207535720826,-22.,-63.8675394171605));
#23018=CARTESIAN_POINT('Ctrl Pts',(63.9806730033805,-21.9157687268541,-64.0396955883018));
#23019=CARTESIAN_POINT('Ctrl Pts',(63.7334500573442,-21.8290315802033,-64.2476809249266));
#23020=CARTESIAN_POINT('Ctrl Pts',(63.490744543383,-21.7438793558854,-64.5516946338151));
#23021=CARTESIAN_POINT('Ctrl Pts',(63.4202655774994,-21.71915210262,-64.6587247347519));
#23022=CARTESIAN_POINT('Ctrl Pts',(63.3508992279611,-21.6948152061911,-64.8305933389432));
#23023=CARTESIAN_POINT('Ctrl Pts',(63.3303552135438,-21.6876074238235,-64.9218325844837));
#23024=CARTESIAN_POINT('Ctrl Pts',(63.3303552135438,-21.6876074238235,-65.));
#23025=CARTESIAN_POINT('',(64.2207535720826,-22.,-63.));
#23026=CARTESIAN_POINT('',(64.2207535720826,-22.,-77.));
#23027=CARTESIAN_POINT('',(63.3303552135438,-21.6876074238235,-63.));
#23028=CARTESIAN_POINT('',(63.0328659997925,-21.5832345653413,-63.));
#23029=CARTESIAN_POINT('',(63.3303552135438,-21.6876074238235,-77.));
#23030=CARTESIAN_POINT('Origin',(53.,-22.,-77.));
#23031=CARTESIAN_POINT('',(57.7792464279174,-22.,-63.));
#23032=CARTESIAN_POINT('',(57.,-22.,-63.));
#23033=CARTESIAN_POINT('',(66.2538081426714,-22.,-63.));
#23034=CARTESIAN_POINT('Ctrl Pts',(64.2207535720826,-22.,-63.8675394171604));
#23035=CARTESIAN_POINT('Ctrl Pts',(64.2947973601691,-22.,-63.7886699029518));
#23036=CARTESIAN_POINT('Ctrl Pts',(64.3732438664359,-22.,-63.716205257488));
#23037=CARTESIAN_POINT('Ctrl Pts',(64.6877753923017,-22.,-63.4558552064108));
#23038=CARTESIAN_POINT('Ctrl Pts',(65.0105765913567,-22.,-63.274575087265));
#23039=CARTESIAN_POINT('Ctrl Pts',(65.5879459758867,-22.,-63.0659599554099));
#23040=CARTESIAN_POINT('Ctrl Pts',(65.9484230764113,-22.,-63.));
#23041=CARTESIAN_POINT('Ctrl Pts',(66.2538081426714,-22.,-63.));
#23042=CARTESIAN_POINT('',(69.,-22.,-63.));
#23043=CARTESIAN_POINT('',(57.,-22.,-63.));
#23044=CARTESIAN_POINT('',(69.,-22.,-41.8486611264284));
#23045=CARTESIAN_POINT('',(69.,-22.,-77.));
#23046=CARTESIAN_POINT('',(53.,-22.,-46.8343975045693));
#23047=CARTESIAN_POINT('Ctrl Pts',(53.,-22.,-46.8343975045693));
#23048=CARTESIAN_POINT('Ctrl Pts',(61.4497577287401,-22.,-44.2291219194588));
#23049=CARTESIAN_POINT('Ctrl Pts',(69.,-22.,-41.8486611264284));
#23050=CARTESIAN_POINT('',(53.,-22.,-63.));
#23051=CARTESIAN_POINT('',(53.,-22.,-77.));
#23052=CARTESIAN_POINT('',(55.7461918573286,-22.,-63.));
#23053=CARTESIAN_POINT('',(57.,-22.,-63.));
#23054=CARTESIAN_POINT('',(57.7792464279174,-22.,-63.8675394171604));
#23055=CARTESIAN_POINT('Ctrl Pts',(55.7461918573286,-22.,-63.));
#23056=CARTESIAN_POINT('Ctrl Pts',(56.0515769235887,-22.,-63.));
#23057=CARTESIAN_POINT('Ctrl Pts',(56.4120540241133,-22.,-63.0659599554099));
#23058=CARTESIAN_POINT('Ctrl Pts',(56.9894234086433,-22.,-63.274575087265));
#23059=CARTESIAN_POINT('Ctrl Pts',(57.3122246076983,-22.,-63.4558552064108));
#23060=CARTESIAN_POINT('Ctrl Pts',(57.6267561335641,-22.,-63.716205257488));
#23061=CARTESIAN_POINT('Ctrl Pts',(57.7052026398309,-22.,-63.7886699029518));
#23062=CARTESIAN_POINT('Ctrl Pts',(57.7792464279174,-22.,-63.8675394171604));
#23063=CARTESIAN_POINT('',(57.7792464279174,-22.,-77.));
#23064=CARTESIAN_POINT('Origin',(58.2244456071868,-21.8438037119117,-77.));
#23065=CARTESIAN_POINT('',(58.6696447864562,-21.6876074238235,-65.));
#23066=CARTESIAN_POINT('Ctrl Pts',(58.6696447864562,-21.6876074238235,-65.));
#23067=CARTESIAN_POINT('Ctrl Pts',(58.6696447864562,-21.6876074238235,-64.9218325844837));
#23068=CARTESIAN_POINT('Ctrl Pts',(58.6491007720389,-21.6948152061911,-64.8305933389432));
#23069=CARTESIAN_POINT('Ctrl Pts',(58.5797344225006,-21.71915210262,-64.6587247347519));
#23070=CARTESIAN_POINT('Ctrl Pts',(58.509255456617,-21.7438793558854,-64.5516946338151));
#23071=CARTESIAN_POINT('Ctrl Pts',(58.2665499426558,-21.8290315802033,-64.2476809249266));
#23072=CARTESIAN_POINT('Ctrl Pts',(58.0193269966195,-21.9157687268541,-64.0396955883018));
#23073=CARTESIAN_POINT('Ctrl Pts',(57.7792464279174,-22.,-63.8675394171605));
#23074=CARTESIAN_POINT('',(58.6696447864562,-21.6876074238235,-63.));
#23075=CARTESIAN_POINT('',(58.6696447864562,-21.6876074238235,-77.));
#23076=CARTESIAN_POINT('',(58.9671340002075,-21.5832345653413,-63.));
#23077=CARTESIAN_POINT('Origin',(61.,-25.,-77.));
#23078=CARTESIAN_POINT('',(56.95,-25.,-76.5));
#23079=CARTESIAN_POINT('Origin',(61.,-25.,-76.5));
#23080=CARTESIAN_POINT('',(56.95,-25.,-65.));
#23081=CARTESIAN_POINT('',(56.95,-25.,-77.));
#23082=CARTESIAN_POINT('Origin',(61.,-25.,-65.));
#23083=CARTESIAN_POINT('Origin',(61.,-25.,-63.));
#23084=CARTESIAN_POINT('Origin',(61.,-25.,-65.));
#23085=CARTESIAN_POINT('Origin',(61.,25.,-76.75));
#23086=CARTESIAN_POINT('',(56.45,25.,-77.));
#23087=CARTESIAN_POINT('Origin',(61.,25.,-77.));
#23088=CARTESIAN_POINT('',(56.7,25.,-76.75));
#23089=CARTESIAN_POINT('Origin',(61.,4.44089209850063E-15,-77.));
#23090=CARTESIAN_POINT('',(75.,25.,-77.));
#23091=CARTESIAN_POINT('',(69.,31.,-77.));
#23092=CARTESIAN_POINT('Origin',(69.,25.,-77.));
#23093=CARTESIAN_POINT('',(75.,-25.,-77.));
#23094=CARTESIAN_POINT('',(75.,-7.,-77.));
#23095=CARTESIAN_POINT('',(69.,-31.,-77.));
#23096=CARTESIAN_POINT('Origin',(69.,-25.,-77.));
#23097=CARTESIAN_POINT('',(53.,-31.,-77.));
#23098=CARTESIAN_POINT('',(57.,-31.,-77.));
#23099=CARTESIAN_POINT('',(47.,-25.,-77.));
#23100=CARTESIAN_POINT('Origin',(53.,-25.,-77.));
#23101=CARTESIAN_POINT('',(47.,25.,-77.));
#23102=CARTESIAN_POINT('',(47.,7.,-77.));
#23103=CARTESIAN_POINT('',(53.,31.,-77.));
#23104=CARTESIAN_POINT('Origin',(53.,25.,-77.));
#23105=CARTESIAN_POINT('',(65.,31.,-77.));
#23106=CARTESIAN_POINT('',(56.45,-25.,-77.));
#23107=CARTESIAN_POINT('Origin',(61.,-25.,-77.));
#23108=CARTESIAN_POINT('',(47.95,-1.5981640728873E-15,-77.));
#23109=CARTESIAN_POINT('Origin',(61.,0.,-77.));
#23110=CARTESIAN_POINT('Origin',(61.,-25.,-76.75));
#23111=CARTESIAN_POINT('',(56.7,-25.,-76.75));
#23112=CARTESIAN_POINT('Origin',(61.,25.,81.75));
#23113=CARTESIAN_POINT('',(56.45,25.,82.));
#23114=CARTESIAN_POINT('Origin',(61.,25.,82.));
#23115=CARTESIAN_POINT('',(56.95,25.,81.5));
#23116=CARTESIAN_POINT('',(56.7,25.,81.75));
#23117=CARTESIAN_POINT('Origin',(61.,25.,81.5));
#23118=CARTESIAN_POINT('Origin',(61.,4.44089209850063E-15,82.));
#23119=CARTESIAN_POINT('',(75.,25.,82.));
#23120=CARTESIAN_POINT('',(75.,-25.,82.));
#23121=CARTESIAN_POINT('',(75.,-7.,82.));
#23122=CARTESIAN_POINT('',(69.,31.,82.));
#23123=CARTESIAN_POINT('Origin',(69.,25.,82.));
#23124=CARTESIAN_POINT('',(53.,31.,82.));
#23125=CARTESIAN_POINT('',(65.,31.,82.));
#23126=CARTESIAN_POINT('',(47.,25.,82.));
#23127=CARTESIAN_POINT('Origin',(53.,25.,82.));
#23128=CARTESIAN_POINT('',(47.,-25.,82.));
#23129=CARTESIAN_POINT('',(47.,7.,82.));
#23130=CARTESIAN_POINT('',(53.,-31.,82.));
#23131=CARTESIAN_POINT('Origin',(53.,-25.,82.));
#23132=CARTESIAN_POINT('',(69.,-31.,82.));
#23133=CARTESIAN_POINT('',(57.,-31.,82.));
#23134=CARTESIAN_POINT('Origin',(69.,-25.,82.));
#23135=CARTESIAN_POINT('',(56.45,-25.,82.));
#23136=CARTESIAN_POINT('Origin',(61.,-25.,82.));
#23137=CARTESIAN_POINT('',(47.95,1.5981640728873E-15,82.));
#23138=CARTESIAN_POINT('Origin',(61.,0.,82.));
#23139=CARTESIAN_POINT('Origin',(61.,25.,82.));
#23140=CARTESIAN_POINT('',(56.95,25.,68.));
#23141=CARTESIAN_POINT('',(56.95,25.,82.));
#23142=CARTESIAN_POINT('Origin',(61.,25.,68.));
#23143=CARTESIAN_POINT('Origin',(61.,-25.,81.75));
#23144=CARTESIAN_POINT('',(56.95,-25.,81.5));
#23145=CARTESIAN_POINT('',(56.7,-25.,81.75));
#23146=CARTESIAN_POINT('Origin',(61.,-25.,81.5));
#23147=CARTESIAN_POINT('Origin',(61.,-25.,82.));
#23148=CARTESIAN_POINT('',(56.95,-25.,68.));
#23149=CARTESIAN_POINT('',(56.95,-25.,82.));
#23150=CARTESIAN_POINT('Origin',(61.,-25.,68.));
#23151=CARTESIAN_POINT('Origin',(68.8623677453688,0.,0.));
#23152=CARTESIAN_POINT('',(70.3988103045684,21.8767588341814,-41.0566760961604));
#23153=CARTESIAN_POINT('',(69.3999656809967,21.9899954602005,-41.7277913961831));
#23154=CARTESIAN_POINT('Ctrl Pts',(69.3999656809931,21.9899954602007,-41.7277913961841));
#23155=CARTESIAN_POINT('Ctrl Pts',(69.4678965900016,21.9865949536025,-41.7081546490098));
#23156=CARTESIAN_POINT('Ctrl Pts',(69.534827005295,21.9823737618781,-41.6848857973726));
#23157=CARTESIAN_POINT('Ctrl Pts',(69.8363491690282,21.9596786155451,-41.5614939978835));
#23158=CARTESIAN_POINT('Ctrl Pts',(70.0500315229559,21.9329167792109,-41.4208836080675));
#23159=CARTESIAN_POINT('Ctrl Pts',(70.2913558806513,21.8953193808038,-41.1842361292856));
#23160=CARTESIAN_POINT('Ctrl Pts',(70.3471478562352,21.8859334155795,-41.1220341127424));
#23161=CARTESIAN_POINT('Ctrl Pts',(70.398810304567,21.8767588341803,-41.0566760961595));
#23162=CARTESIAN_POINT('',(69.3999656809967,21.9899954602005,41.7277913961831));
#23163=CARTESIAN_POINT('Origin',(69.3999656809967,0.,9.04378927871628E-16));
#23164=CARTESIAN_POINT('',(70.3988103045684,21.8767588341814,41.0566760961604));
#23165=CARTESIAN_POINT('Ctrl Pts',(70.398810304567,21.8767588341803,41.0566760961595));
#23166=CARTESIAN_POINT('Ctrl Pts',(70.2886503403277,21.8963218164135,41.1960391538931));
#23167=CARTESIAN_POINT('Ctrl Pts',(70.1605038308314,21.9167166021157,41.3200714701435));
#23168=CARTESIAN_POINT('Ctrl Pts',(69.8499581892739,21.9564850241577,41.5472005422254));
#23169=CARTESIAN_POINT('Ctrl Pts',(69.6655971081557,21.9746882921927,41.6417814905459));
#23170=CARTESIAN_POINT('Ctrl Pts',(69.4462977513165,21.9875746254245,41.7139399145121));
#23171=CARTESIAN_POINT('Ctrl Pts',(69.4231883393022,21.9888329731391,41.7210784362578));
#23172=CARTESIAN_POINT('Ctrl Pts',(69.3999656809966,21.9899954602005,41.7277913961831));
#23173=CARTESIAN_POINT('Origin',(70.3988103045635,0.,8.91992201499275E-16));
#23174=CARTESIAN_POINT('Origin',(59.25,0.,0.));
#23175=CARTESIAN_POINT('Ctrl Pts',(69.3999656809967,21.9899954602005,-41.7277913961831));
#23176=CARTESIAN_POINT('Ctrl Pts',(69.2669412328493,21.9966544394525,-41.7662446937235));
#23177=CARTESIAN_POINT('Ctrl Pts',(69.1335296058873,22.,-41.8065615513282));
#23178=CARTESIAN_POINT('Ctrl Pts',(69.,22.,-41.8486611264283));
#23179=CARTESIAN_POINT('',(48.5,20.6143782776615,-48.8267079396664));
#23180=CARTESIAN_POINT('Ctrl Pts',(53.,22.,-46.8343975045693));
#23181=CARTESIAN_POINT('Ctrl Pts',(52.220819689021,22.,-47.0746386458849));
#23182=CARTESIAN_POINT('Ctrl Pts',(51.4345269237376,21.8835425868198,-47.3718185033061));
#23183=CARTESIAN_POINT('Ctrl Pts',(49.8969249897714,21.4203044222019,-48.0534285948251));
#23184=CARTESIAN_POINT('Ctrl Pts',(49.1505318652661,21.0569585581973,-48.4427922865552));
#23185=CARTESIAN_POINT('Ctrl Pts',(48.5,20.6143782776615,-48.8267079396664));
#23186=CARTESIAN_POINT('',(48.5,20.6143782776615,48.8267079396664));
#23187=CARTESIAN_POINT('Origin',(48.5,0.,0.));
#23188=CARTESIAN_POINT('',(53.,22.,46.8343975045693));
#23189=CARTESIAN_POINT('Ctrl Pts',(48.5,20.6143782776615,48.8267079396664));
#23190=CARTESIAN_POINT('Ctrl Pts',(49.1505318652661,21.0569585581973,48.4427922865552));
#23191=CARTESIAN_POINT('Ctrl Pts',(49.8969249897714,21.4203044222019,48.0534285948251));
#23192=CARTESIAN_POINT('Ctrl Pts',(51.4345269237376,21.8835425868198,47.3718185033061));
#23193=CARTESIAN_POINT('Ctrl Pts',(52.220819689021,22.,47.0746386458849));
#23194=CARTESIAN_POINT('Ctrl Pts',(53.,22.,46.8343975045693));
#23195=CARTESIAN_POINT('',(69.,22.,41.8486611264283));
#23196=CARTESIAN_POINT('Ctrl Pts',(53.,22.,46.8343975045693));
#23197=CARTESIAN_POINT('Ctrl Pts',(61.4497577287401,22.,44.2291219194588));
#23198=CARTESIAN_POINT('Ctrl Pts',(69.,22.,41.8486611264284));
#23199=CARTESIAN_POINT('Ctrl Pts',(69.,22.,41.8486611264283));
#23200=CARTESIAN_POINT('Ctrl Pts',(69.1335306008183,22.,41.8065612376436));
#23201=CARTESIAN_POINT('Ctrl Pts',(69.266941620321,21.9966544200563,41.7662445817172));
#23202=CARTESIAN_POINT('Ctrl Pts',(69.3999656809966,21.9899954602005,41.7277913961831));
#23203=CARTESIAN_POINT('Origin',(68.8623677453688,0.,0.));
#23204=CARTESIAN_POINT('',(70.3988103045684,-21.8767588341814,41.0566760961604));
#23205=CARTESIAN_POINT('',(69.3999656809967,-21.9899954602005,41.7277913961831));
#23206=CARTESIAN_POINT('Ctrl Pts',(69.3999656809931,-21.9899954602007,41.7277913961841));
#23207=CARTESIAN_POINT('Ctrl Pts',(69.4678965900016,-21.9865949536025,41.7081546490098));
#23208=CARTESIAN_POINT('Ctrl Pts',(69.534827005295,-21.9823737618781,41.6848857973726));
#23209=CARTESIAN_POINT('Ctrl Pts',(69.8363491690282,-21.9596786155451,41.5614939978835));
#23210=CARTESIAN_POINT('Ctrl Pts',(70.0500315229559,-21.9329167792109,41.4208836080676));
#23211=CARTESIAN_POINT('Ctrl Pts',(70.2913558806513,-21.8953193808038,41.1842361292856));
#23212=CARTESIAN_POINT('Ctrl Pts',(70.3471478562352,-21.8859334155794,41.1220341127424));
#23213=CARTESIAN_POINT('Ctrl Pts',(70.398810304567,-21.8767588341803,41.0566760961595));
#23214=CARTESIAN_POINT('',(69.3999656809967,-21.9899954602005,-41.7277913961831));
#23215=CARTESIAN_POINT('Origin',(69.3999656809967,0.,-7.2204335534144E-15));
#23216=CARTESIAN_POINT('',(70.3988103045683,-21.8767588341814,-41.0566760961604));
#23217=CARTESIAN_POINT('Ctrl Pts',(70.398810304567,-21.8767588341803,-41.0566760961595));
#23218=CARTESIAN_POINT('Ctrl Pts',(70.2886503403277,-21.8963218164135,-41.1960391538931));
#23219=CARTESIAN_POINT('Ctrl Pts',(70.1605038308314,-21.9167166021156,-41.3200714701435));
#23220=CARTESIAN_POINT('Ctrl Pts',(69.8499581892738,-21.9564850241576,-41.5472005422254));
#23221=CARTESIAN_POINT('Ctrl Pts',(69.6655971081557,-21.9746882921927,-41.6417814905459));
#23222=CARTESIAN_POINT('Ctrl Pts',(69.4462977513165,-21.9875746254244,-41.7139399145121));
#23223=CARTESIAN_POINT('Ctrl Pts',(69.4231883393022,-21.988832973139,-41.7210784362578));
#23224=CARTESIAN_POINT('Ctrl Pts',(69.3999656809966,-21.9899954602005,-41.7277913961831));
#23225=CARTESIAN_POINT('',(70.3988103045635,-46.5214276345238,-5.69723174443847E-15));
#23226=CARTESIAN_POINT('Origin',(70.3988103045635,0.,-7.12153968054809E-15));
#23227=CARTESIAN_POINT('Origin',(70.3988103045635,0.,-7.12153968054809E-15));
#23228=CARTESIAN_POINT('Origin',(59.25,0.,0.));
#23229=CARTESIAN_POINT('',(69.,-22.,41.8486611264284));
#23230=CARTESIAN_POINT('Ctrl Pts',(69.3999656809967,-21.9899954602005,41.7277913961831));
#23231=CARTESIAN_POINT('Ctrl Pts',(69.2669412328493,-21.9966544394524,41.7662446937235));
#23232=CARTESIAN_POINT('Ctrl Pts',(69.1335296058873,-22.,41.8065615513282));
#23233=CARTESIAN_POINT('Ctrl Pts',(69.,-22.,41.8486611264284));
#23234=CARTESIAN_POINT('',(53.,-22.,46.8343975045693));
#23235=CARTESIAN_POINT('Ctrl Pts',(69.,-22.,41.8486611264284));
#23236=CARTESIAN_POINT('Ctrl Pts',(61.4497577287401,-22.,44.2291219194588));
#23237=CARTESIAN_POINT('Ctrl Pts',(53.,-22.,46.8343975045693));
#23238=CARTESIAN_POINT('',(48.5,-20.6143782776615,48.8267079396664));
#23239=CARTESIAN_POINT('Ctrl Pts',(53.,-22.,46.8343975045693));
#23240=CARTESIAN_POINT('Ctrl Pts',(52.220819689021,-22.,47.0746386458849));
#23241=CARTESIAN_POINT('Ctrl Pts',(51.4345269237375,-21.8835425868198,47.3718185033061));
#23242=CARTESIAN_POINT('Ctrl Pts',(49.8969249897714,-21.4203044222019,48.0534285948251));
#23243=CARTESIAN_POINT('Ctrl Pts',(49.1505318652661,-21.0569585581973,48.4427922865552));
#23244=CARTESIAN_POINT('Ctrl Pts',(48.5,-20.6143782776615,48.8267079396664));
#23245=CARTESIAN_POINT('',(48.5,-20.6143782776615,-48.8267079396664));
#23246=CARTESIAN_POINT('Origin',(48.5,0.,0.));
#23247=CARTESIAN_POINT('Ctrl Pts',(48.5,-20.6143782776615,-48.8267079396664));
#23248=CARTESIAN_POINT('Ctrl Pts',(49.1505318652661,-21.0569585581973,-48.4427922865552));
#23249=CARTESIAN_POINT('Ctrl Pts',(49.8969249897714,-21.4203044222019,-48.0534285948251));
#23250=CARTESIAN_POINT('Ctrl Pts',(51.4345269237375,-21.8835425868198,-47.3718185033061));
#23251=CARTESIAN_POINT('Ctrl Pts',(52.220819689021,-22.,-47.0746386458849));
#23252=CARTESIAN_POINT('Ctrl Pts',(53.,-22.,-46.8343975045693));
#23253=CARTESIAN_POINT('Ctrl Pts',(69.,-22.,-41.8486611264283));
#23254=CARTESIAN_POINT('Ctrl Pts',(69.1335306008184,-22.,-41.8065612376436));
#23255=CARTESIAN_POINT('Ctrl Pts',(69.266941620321,-21.9966544200563,-41.7662445817172));
#23256=CARTESIAN_POINT('Ctrl Pts',(69.3999656809967,-21.9899954602005,-41.7277913961831));
#23257=CARTESIAN_POINT('Origin',(78.,0.,0.));
#23258=CARTESIAN_POINT('',(80.,-4.19758713816547E-15,34.2759001296373));
#23259=CARTESIAN_POINT('Origin',(80.,0.,0.));
#23260=CARTESIAN_POINT('',(79.5364425591947,-4.35438709334811E-15,35.5562689289663));
#23261=CARTESIAN_POINT('Origin',(78.,-4.19758713816547E-15,34.2759001296373));
#23262=CARTESIAN_POINT('',(79.5364425591948,-35.5562689289663,-4.35438709334811E-15));
#23263=CARTESIAN_POINT('Origin',(79.5364425591947,0.,-5.44298386668513E-15));
#23264=CARTESIAN_POINT('Origin',(79.5364425591947,0.,-5.44298386668513E-15));
#23265=CARTESIAN_POINT('Origin',(75.,0.,0.));
#23266=CARTESIAN_POINT('',(75.,-41.,-5.02105187650415E-15));
#23267=CARTESIAN_POINT('',(77.,-14.,-35.9716555081915));
#23268=CARTESIAN_POINT('Ctrl Pts',(70.398810304567,-21.8767588341803,-41.0566760961595));
#23269=CARTESIAN_POINT('Ctrl Pts',(71.2727530473023,-21.7215579273257,-39.9510536156882));
#23270=CARTESIAN_POINT('Ctrl Pts',(72.1553913142385,-21.4169490490281,-38.9085591876444));
#23271=CARTESIAN_POINT('Ctrl Pts',(73.0068003967573,-20.9242725668871,-38.0135049004133));
#23272=CARTESIAN_POINT('Ctrl Pts',(73.6552875413432,-20.5490189177681,-37.3317748004022));
#23273=CARTESIAN_POINT('Ctrl Pts',(74.3605604649236,-20.0126010939214,-36.6628462695613));
#23274=CARTESIAN_POINT('Ctrl Pts',(75.2978777322535,-18.9556514474071,-35.9519067932131));
#23275=CARTESIAN_POINT('Ctrl Pts',(75.5909608136772,-18.5615213463442,-35.7620681117759));
#23276=CARTESIAN_POINT('Ctrl Pts',(76.10601454772,-17.7084765949661,-35.5027149353752));
#23277=CARTESIAN_POINT('Ctrl Pts',(76.3278529636206,-17.2494659834457,-35.4332534860856));
#23278=CARTESIAN_POINT('Ctrl Pts',(76.6706196605434,-16.3224653535192,-35.4171046265844));
#23279=CARTESIAN_POINT('Ctrl Pts',(76.7982138286546,-15.8499176073548,-35.4643373367294));
#23280=CARTESIAN_POINT('Ctrl Pts',(76.9611527928263,-14.9146287542956,-35.6556385052494));
#23281=CARTESIAN_POINT('Ctrl Pts',(77.,-14.4521831933392,-35.795667925265));
#23282=CARTESIAN_POINT('Ctrl Pts',(77.,-14.,-35.9716555081914));
#23283=CARTESIAN_POINT('',(77.,14.,-35.9716555081914));
#23284=CARTESIAN_POINT('Origin',(77.,0.,0.));
#23285=CARTESIAN_POINT('Ctrl Pts',(77.,14.,-35.9716555081914));
#23286=CARTESIAN_POINT('Ctrl Pts',(77.,14.4521831933392,-35.795667925265));
#23287=CARTESIAN_POINT('Ctrl Pts',(76.9611527928263,14.9146287542956,-35.6556385052494));
#23288=CARTESIAN_POINT('Ctrl Pts',(76.7982138286546,15.8499176073548,-35.4643373367294));
#23289=CARTESIAN_POINT('Ctrl Pts',(76.6706196605434,16.3224653535192,-35.4171046265844));
#23290=CARTESIAN_POINT('Ctrl Pts',(76.3278529636206,17.2494659834456,-35.4332534860856));
#23291=CARTESIAN_POINT('Ctrl Pts',(76.10601454772,17.7084765949661,-35.5027149353752));
#23292=CARTESIAN_POINT('Ctrl Pts',(75.5909608136772,18.5615213463443,-35.7620681117759));
#23293=CARTESIAN_POINT('Ctrl Pts',(75.2978777322535,18.9556514474071,-35.9519067932131));
#23294=CARTESIAN_POINT('Ctrl Pts',(74.3605604649237,20.0126010939214,-36.6628462695613));
#23295=CARTESIAN_POINT('Ctrl Pts',(73.6552875413432,20.5490189177681,-37.3317748004022));
#23296=CARTESIAN_POINT('Ctrl Pts',(72.1553913142392,21.4169490490277,-38.9085591876437));
#23297=CARTESIAN_POINT('Ctrl Pts',(71.2727530473009,21.7215579273259,-39.9510536156899));
#23298=CARTESIAN_POINT('Ctrl Pts',(70.398810304567,21.8767588341803,-41.0566760961595));
#23299=CARTESIAN_POINT('',(77.,14.,35.9716555081914));
#23300=CARTESIAN_POINT('Ctrl Pts',(70.398810304567,21.8767588341803,41.0566760961595));
#23301=CARTESIAN_POINT('Ctrl Pts',(71.2727530473009,21.7215579273259,39.9510536156899));
#23302=CARTESIAN_POINT('Ctrl Pts',(72.1553913142392,21.4169490490277,38.9085591876437));
#23303=CARTESIAN_POINT('Ctrl Pts',(73.6552875413432,20.5490189177681,37.3317748004022));
#23304=CARTESIAN_POINT('Ctrl Pts',(74.3605604649237,20.0126010939214,36.6628462695613));
#23305=CARTESIAN_POINT('Ctrl Pts',(75.2978777322535,18.9556514474071,35.9519067932131));
#23306=CARTESIAN_POINT('Ctrl Pts',(75.5909608136772,18.5615213463442,35.7620681117759));
#23307=CARTESIAN_POINT('Ctrl Pts',(76.10601454772,17.7084765949661,35.5027149353752));
#23308=CARTESIAN_POINT('Ctrl Pts',(76.3278529636206,17.2494659834457,35.4332534860856));
#23309=CARTESIAN_POINT('Ctrl Pts',(76.6706196605434,16.3224653535192,35.4171046265844));
#23310=CARTESIAN_POINT('Ctrl Pts',(76.7982138286546,15.8499176073548,35.4643373367294));
#23311=CARTESIAN_POINT('Ctrl Pts',(76.9611527928263,14.9146287542956,35.6556385052494));
#23312=CARTESIAN_POINT('Ctrl Pts',(77.,14.4521831933392,35.795667925265));
#23313=CARTESIAN_POINT('Ctrl Pts',(77.,14.,35.9716555081914));
#23314=CARTESIAN_POINT('',(77.,-14.,35.9716555081915));
#23315=CARTESIAN_POINT('Origin',(77.,0.,0.));
#23316=CARTESIAN_POINT('Ctrl Pts',(77.,-14.,35.9716555081914));
#23317=CARTESIAN_POINT('Ctrl Pts',(77.,-14.4521831941371,35.7956679249545));
#23318=CARTESIAN_POINT('Ctrl Pts',(76.9611527928323,-14.9146287542614,35.6556385052564));
#23319=CARTESIAN_POINT('Ctrl Pts',(76.7982138286546,-15.8499176073548,35.4643373367294));
#23320=CARTESIAN_POINT('Ctrl Pts',(76.6706196605434,-16.3224653535192,35.4171046265844));
#23321=CARTESIAN_POINT('Ctrl Pts',(76.3278529636206,-17.2494659834457,35.4332534860856));
#23322=CARTESIAN_POINT('Ctrl Pts',(76.10601454772,-17.7084765949661,35.5027149353752));
#23323=CARTESIAN_POINT('Ctrl Pts',(75.5909608136772,-18.5615213463442,35.7620681117759));
#23324=CARTESIAN_POINT('Ctrl Pts',(75.2978777322535,-18.9556514474071,35.9519067932131));
#23325=CARTESIAN_POINT('Ctrl Pts',(74.3605604649236,-20.0126010939214,36.6628462695613));
#23326=CARTESIAN_POINT('Ctrl Pts',(73.6552875413432,-20.5490189177681,37.3317748004022));
#23327=CARTESIAN_POINT('Ctrl Pts',(73.0068003967573,-20.9242725668871,38.0135049004133));
#23328=CARTESIAN_POINT('Ctrl Pts',(72.1553913142392,-21.4169490490277,38.9085591876437));
#23329=CARTESIAN_POINT('Ctrl Pts',(71.2727530473009,-21.7215579273259,39.9510536156899));
#23330=CARTESIAN_POINT('Ctrl Pts',(70.398810304567,-21.8767588341803,41.0566760961595));
#23331=CARTESIAN_POINT('Origin',(80.,0.,0.));
#23332=CARTESIAN_POINT('',(80.,2.,-8.));
#23333=CARTESIAN_POINT('',(80.,1.99999999999999,-33.));
#23334=CARTESIAN_POINT('',(80.,2.,-16.5));
#23335=CARTESIAN_POINT('',(80.,-2.00000000000001,-33.));
#23336=CARTESIAN_POINT('',(80.,-1.,-33.));
#23337=CARTESIAN_POINT('',(80.,-2.,-8.));
#23338=CARTESIAN_POINT('',(80.,-2.,-4.));
#23339=CARTESIAN_POINT('',(80.,0.999999999999999,-8.));
#23340=CARTESIAN_POINT('',(80.,5.92820323027551,5.73205080756888));
#23341=CARTESIAN_POINT('',(80.,27.5788383248865,18.2320508075689));
#23342=CARTESIAN_POINT('',(80.,13.2894191624432,9.98205080756887));
#23343=CARTESIAN_POINT('',(80.,29.5788383248865,14.7679491924311));
#23344=CARTESIAN_POINT('',(80.,29.0788383248865,15.6339745962156));
#23345=CARTESIAN_POINT('',(80.,7.92820323027551,2.26794919243112));
#23346=CARTESIAN_POINT('',(80.,4.46410161513776,0.267949192431122));
#23347=CARTESIAN_POINT('',(80.,6.42820323027551,4.86602540378444));
#23348=CARTESIAN_POINT('',(80.,-2.,8.));
#23349=CARTESIAN_POINT('',(80.,-2.,33.));
#23350=CARTESIAN_POINT('',(80.,-2.,16.5));
#23351=CARTESIAN_POINT('',(80.,2.,33.));
#23352=CARTESIAN_POINT('',(80.,1.,33.));
#23353=CARTESIAN_POINT('',(80.,2.,8.));
#23354=CARTESIAN_POINT('',(80.,2.,4.));
#23355=CARTESIAN_POINT('',(80.,-1.,8.));
#23356=CARTESIAN_POINT('',(80.,-7.92820323027551,2.26794919243112));
#23357=CARTESIAN_POINT('',(80.,-29.5788383248865,14.7679491924311));
#23358=CARTESIAN_POINT('',(80.,-15.2894191624432,6.51794919243112));
#23359=CARTESIAN_POINT('',(80.,-27.5788383248865,18.2320508075689));
#23360=CARTESIAN_POINT('',(80.,-28.0788383248865,17.3660254037844));
#23361=CARTESIAN_POINT('',(80.,-5.92820323027551,5.73205080756888));
#23362=CARTESIAN_POINT('',(80.,-2.46410161513775,3.73205080756888));
#23363=CARTESIAN_POINT('',(80.,-7.42820323027551,3.13397459621556));
#23364=CARTESIAN_POINT('',(80.,-5.92820323027551,-5.73205080756888));
#23365=CARTESIAN_POINT('',(80.,-27.5788383248865,-18.2320508075689));
#23366=CARTESIAN_POINT('',(80.,-13.2894191624432,-9.98205080756888));
#23367=CARTESIAN_POINT('',(80.,-29.5788383248865,-14.7679491924311));
#23368=CARTESIAN_POINT('',(80.,-29.0788383248865,-15.6339745962156));
#23369=CARTESIAN_POINT('',(80.,-7.92820323027551,-2.26794919243112));
#23370=CARTESIAN_POINT('',(80.,-4.46410161513775,-0.267949192431123));
#23371=CARTESIAN_POINT('',(80.,-6.42820323027551,-4.86602540378444));
#23372=CARTESIAN_POINT('',(80.,7.92820323027551,-2.26794919243113));
#23373=CARTESIAN_POINT('',(80.,29.5788383248865,-14.7679491924311));
#23374=CARTESIAN_POINT('',(80.,15.2894191624432,-6.51794919243113));
#23375=CARTESIAN_POINT('',(80.,27.5788383248865,-18.2320508075689));
#23376=CARTESIAN_POINT('',(80.,28.0788383248865,-17.3660254037845));
#23377=CARTESIAN_POINT('',(80.,5.92820323027551,-5.73205080756888));
#23378=CARTESIAN_POINT('',(80.,2.46410161513775,-3.73205080756888));
#23379=CARTESIAN_POINT('',(80.,7.42820323027551,-3.13397459621557));
#23380=CARTESIAN_POINT('Origin',(46.5,0.,-2.20309881449055E-15));
#23381=CARTESIAN_POINT('',(48.5,-29.0466953015038,65.0006740405344));
#23382=CARTESIAN_POINT('',(48.0857864376269,-30.6065287460451,65.6281854386855));
#23383=CARTESIAN_POINT('Ctrl Pts',(48.0857864376269,-30.6065287460451,65.6281854386855));
#23384=CARTESIAN_POINT('Ctrl Pts',(48.1301492537468,-30.5806858219106,65.576544441517));
#23385=CARTESIAN_POINT('Ctrl Pts',(48.1707278411709,-30.5469525825928,65.5268107752811));
#23386=CARTESIAN_POINT('Ctrl Pts',(48.2441371413255,-30.4644482587098,65.4324498012713));
#23387=CARTESIAN_POINT('Ctrl Pts',(48.2762461582976,-30.4166263879609,65.3887900387193));
#23388=CARTESIAN_POINT('Ctrl Pts',(48.3631644375932,-30.2517748834464,65.2649170060744));
#23389=CARTESIAN_POINT('Ctrl Pts',(48.4031257978626,-30.1193145924239,65.1990939013729));
#23390=CARTESIAN_POINT('Ctrl Pts',(48.4773089651312,-29.7481720100829,65.0666632800059));
#23391=CARTESIAN_POINT('Ctrl Pts',(48.4999999982949,-29.4453272025579,65.007596110854));
#23392=CARTESIAN_POINT('Ctrl Pts',(48.5,-29.0466953013294,65.0006740505758));
#23393=CARTESIAN_POINT('',(48.0857864376272,-31.3127256445526,-65.2941922269196));
#23394=CARTESIAN_POINT('Origin',(48.0857864376269,0.,-2.20309881449055E-15));
#23395=CARTESIAN_POINT('',(48.2311293323885,-31.4232291377153,-64.9999999933255));
#23396=CARTESIAN_POINT('Ctrl Pts',(48.2311293323885,-31.4232291377153,-64.9999999933255));
#23397=CARTESIAN_POINT('Ctrl Pts',(48.1867097281574,-31.3902501884761,-65.1012175444252));
#23398=CARTESIAN_POINT('Ctrl Pts',(48.1379693104345,-31.3533479994135,-65.1994072998738));
#23399=CARTESIAN_POINT('Ctrl Pts',(48.0857864376269,-31.3127256445523,-65.29419222692));
#23400=CARTESIAN_POINT('',(48.5,-31.2619954337637,-63.9647228889383));
#23401=CARTESIAN_POINT('Ctrl Pts',(48.5,-31.2619954300771,-63.9647228854569));
#23402=CARTESIAN_POINT('Ctrl Pts',(48.5,-31.3066103800828,-64.0246074793082));
#23403=CARTESIAN_POINT('Ctrl Pts',(48.4959556515835,-31.3454934513646,-64.0880064784246));
#23404=CARTESIAN_POINT('Ctrl Pts',(48.4796166024191,-31.409284557683,-64.2199289334738));
#23405=CARTESIAN_POINT('Ctrl Pts',(48.4676779476615,-31.4339507060007,-64.2871111751952));
#23406=CARTESIAN_POINT('Ctrl Pts',(48.420825382814,-31.4874720705551,-64.4950891861979));
#23407=CARTESIAN_POINT('Ctrl Pts',(48.3762987971587,-31.4934261407582,-64.6350319244059));
#23408=CARTESIAN_POINT('Ctrl Pts',(48.2959416031664,-31.4655323782762,-64.8476351547665));
#23409=CARTESIAN_POINT('Ctrl Pts',(48.2645571018583,-31.4480472944176,-64.9238291895505));
#23410=CARTESIAN_POINT('Ctrl Pts',(48.2311293323885,-31.4232291377153,-64.9999999933256));
#23411=CARTESIAN_POINT('Origin',(48.5,0.,-2.20309881449055E-15));
#23412=CARTESIAN_POINT('Origin',(48.5,53.,0.));
#23413=CARTESIAN_POINT('',(48.5,-28.9686269665969,-63.));
#23414=CARTESIAN_POINT('Ctrl Pts',(48.5,-31.2619954330609,-63.964722889462));
#23415=CARTESIAN_POINT('Ctrl Pts',(48.5,-31.1786502720937,-63.8528525155057));
#23416=CARTESIAN_POINT('Ctrl Pts',(48.5,-31.0821687424774,-63.7502960288675));
#23417=CARTESIAN_POINT('Ctrl Pts',(48.5,-30.7662183987535,-63.4685459818617));
#23418=CARTESIAN_POINT('Ctrl Pts',(48.5,-30.4573223491148,-63.2950310532685));
#23419=CARTESIAN_POINT('Ctrl Pts',(48.5,-29.8155012575532,-63.0638354527098));
#23420=CARTESIAN_POINT('Ctrl Pts',(48.5,-29.3555738612142,-63.));
#23421=CARTESIAN_POINT('Ctrl Pts',(48.5,-28.9686269665969,-63.));
#23422=CARTESIAN_POINT('',(48.5,-20.6143782776615,-63.));
#23423=CARTESIAN_POINT('',(48.5,26.5,-63.));
#23424=CARTESIAN_POINT('',(48.5,-20.6143782776615,-77.));
#23425=CARTESIAN_POINT('',(48.5,-20.6143782776615,65.));
#23426=CARTESIAN_POINT('',(48.5,-20.6143782776615,-77.));
#23427=CARTESIAN_POINT('',(48.5,-28.9686269665969,65.));
#23428=CARTESIAN_POINT('',(48.5,26.5,65.));
#23429=CARTESIAN_POINT('Ctrl Pts',(48.5,-28.9686269665969,65.));
#23430=CARTESIAN_POINT('Ctrl Pts',(48.5,-28.9943212164188,65.));
#23431=CARTESIAN_POINT('Ctrl Pts',(48.5,-29.0203628803793,65.0002168001558));
#23432=CARTESIAN_POINT('Ctrl Pts',(48.5,-29.0466953013294,65.0006740505758));
#23433=CARTESIAN_POINT('',(48.5,-62.,4.50000000000001));
#23434=CARTESIAN_POINT('Origin',(48.5,-62.,7.59281015471359E-15));
#23435=CARTESIAN_POINT('',(48.5,-31.,58.1935750346352));
#23436=CARTESIAN_POINT('Origin',(48.5,-31.,53.6935750346352));
#23437=CARTESIAN_POINT('',(48.5,-31.,-49.1935750346352));
#23438=CARTESIAN_POINT('Origin',(48.5,-31.,-53.6935750346352));
#23439=CARTESIAN_POINT('Origin',(46.6715728752538,0.,0.));
#23440=CARTESIAN_POINT('',(46.671572875469,-29.8356437966493,66.6245777415471));
#23441=CARTESIAN_POINT('Ctrl Pts',(46.6715728756007,-29.8356437965537,66.62457774159));
#23442=CARTESIAN_POINT('Ctrl Pts',(46.9003594149229,-30.0980676345434,66.5070597861704));
#23443=CARTESIAN_POINT('Ctrl Pts',(47.1258706110947,-30.2962111663502,66.3731410562788));
#23444=CARTESIAN_POINT('Ctrl Pts',(47.5020219686064,-30.5347787801062,66.1177462694265));
#23445=CARTESIAN_POINT('Ctrl Pts',(47.6577886183648,-30.5990942737804,66.0001438773577));
#23446=CARTESIAN_POINT('Ctrl Pts',(47.8979638703951,-30.6386169314764,65.801001256245));
#23447=CARTESIAN_POINT('Ctrl Pts',(47.9949018863232,-30.6355802321398,65.7149190292199));
#23448=CARTESIAN_POINT('Ctrl Pts',(48.0857864376269,-30.6065287460451,65.6281854386855));
#23449=CARTESIAN_POINT('',(46.6715728756007,-73.,-8.93992163377568E-15));
#23450=CARTESIAN_POINT('Origin',(46.6715728752538,0.,0.));
#23451=CARTESIAN_POINT('',(46.6715728752538,-29.8939769234005,-66.5984244836407));
#23452=CARTESIAN_POINT('Origin',(46.6715728752538,0.,0.));
#23453=CARTESIAN_POINT('Ctrl Pts',(48.0857864376272,-31.3127256445525,-65.2941922269195));
#23454=CARTESIAN_POINT('Ctrl Pts',(47.8770411481129,-31.1502254836754,-65.6036293796078));
#23455=CARTESIAN_POINT('Ctrl Pts',(47.6239041583091,-30.9374332353599,-65.8819860357444));
#23456=CARTESIAN_POINT('Ctrl Pts',(47.1265432809023,-30.4403912323438,-66.3084804710889));
#23457=CARTESIAN_POINT('Ctrl Pts',(46.8987540346771,-30.187746067397,-66.4665605832628));
#23458=CARTESIAN_POINT('Ctrl Pts',(46.6715728752538,-29.8939769234005,-66.5984244836407));
#23459=CARTESIAN_POINT('Origin',(43.5,0.,0.));
#23460=CARTESIAN_POINT('',(46.0618680733842,-28.9827534908495,67.0000000003308));
#23461=CARTESIAN_POINT('Ctrl Pts',(46.6715728756007,-29.8356437965537,66.62457774159));
#23462=CARTESIAN_POINT('Ctrl Pts',(46.4403768088297,-29.570456170775,66.7433333691705));
#23463=CARTESIAN_POINT('Ctrl Pts',(46.235774905439,-29.2857068488205,66.8689489186728));
#23464=CARTESIAN_POINT('Ctrl Pts',(46.0618680734383,-28.9827534909439,67.0000000006207));
#23465=CARTESIAN_POINT('',(45.,-25.,68.585712797929));
#23466=CARTESIAN_POINT('Ctrl Pts',(46.0618680734383,-28.9827534909439,67.0000000006207));
#23467=CARTESIAN_POINT('Ctrl Pts',(45.9012005717238,-28.7028636293842,67.1210743119957));
#23468=CARTESIAN_POINT('Ctrl Pts',(45.757046826217,-28.4123616493805,67.244642097791));
#23469=CARTESIAN_POINT('Ctrl Pts',(45.2085080184809,-27.1145210836178,67.7862582857373));
#23470=CARTESIAN_POINT('Ctrl Pts',(45.,-26.0264488036591,68.211564611016));
#23471=CARTESIAN_POINT('Ctrl Pts',(45.,-25.,68.585712797929));
#23472=CARTESIAN_POINT('',(45.,25.,68.585712797929));
#23473=CARTESIAN_POINT('Origin',(45.,0.,0.));
#23474=CARTESIAN_POINT('',(46.0618680733842,28.9827534908495,67.0000000003308));
#23475=CARTESIAN_POINT('Ctrl Pts',(45.,25.,68.585712797929));
#23476=CARTESIAN_POINT('Ctrl Pts',(45.,26.0264488036591,68.211564611016));
#23477=CARTESIAN_POINT('Ctrl Pts',(45.2085080184809,27.1145210836178,67.7862582857373));
#23478=CARTESIAN_POINT('Ctrl Pts',(45.757046826217,28.4123616493805,67.244642097791));
#23479=CARTESIAN_POINT('Ctrl Pts',(45.9012005717238,28.7028636293842,67.1210743119957));
#23480=CARTESIAN_POINT('Ctrl Pts',(46.0618680734383,28.9827534909439,67.0000000006207));
#23481=CARTESIAN_POINT('',(46.6715728753143,29.8356437962946,66.624577741706));
#23482=CARTESIAN_POINT('Ctrl Pts',(46.0618680734383,28.9827534909439,67.0000000006207));
#23483=CARTESIAN_POINT('Ctrl Pts',(46.2356286911114,29.2854521370245,66.8690591014966));
#23484=CARTESIAN_POINT('Ctrl Pts',(46.4402143281585,29.5702698013771,66.7434168286244));
#23485=CARTESIAN_POINT('Ctrl Pts',(46.6715728753514,29.8356437962676,66.6245777417181));
#23486=CARTESIAN_POINT('',(46.6715728752538,29.8939769234005,-66.5984244836407));
#23487=CARTESIAN_POINT('Origin',(46.6715728752538,0.,0.));
#23488=CARTESIAN_POINT('',(45.,25.,-68.585712797929));
#23489=CARTESIAN_POINT('Ctrl Pts',(46.6715728752538,29.8939769234005,-66.5984244836407));
#23490=CARTESIAN_POINT('Ctrl Pts',(46.2545757421566,29.3547557522879,-66.8404642221305));
#23491=CARTESIAN_POINT('Ctrl Pts',(45.9004614465488,28.751680051953,-67.1030373856642));
#23492=CARTESIAN_POINT('Ctrl Pts',(45.2085080184809,27.1145210836178,-67.7862582857373));
#23493=CARTESIAN_POINT('Ctrl Pts',(45.,26.0264488036591,-68.211564611016));
#23494=CARTESIAN_POINT('Ctrl Pts',(45.,25.,-68.585712797929));
#23495=CARTESIAN_POINT('',(45.,-25.,-68.585712797929));
#23496=CARTESIAN_POINT('Origin',(45.,0.,0.));
#23497=CARTESIAN_POINT('Ctrl Pts',(45.,-25.,-68.585712797929));
#23498=CARTESIAN_POINT('Ctrl Pts',(45.,-26.0264488036591,-68.211564611016));
#23499=CARTESIAN_POINT('Ctrl Pts',(45.2085080184809,-27.1145210836178,-67.7862582857373));
#23500=CARTESIAN_POINT('Ctrl Pts',(45.9004614465488,-28.751680051953,-67.1030373856642));
#23501=CARTESIAN_POINT('Ctrl Pts',(46.2545757421565,-29.3547557522879,-66.8404642221305));
#23502=CARTESIAN_POINT('Ctrl Pts',(46.6715728752538,-29.8939769234005,-66.5984244836407));
#23503=CARTESIAN_POINT('',(40.5,-73.,0.));
#23504=CARTESIAN_POINT('',(43.5,-73.,-8.93992163377568E-15));
#23505=CARTESIAN_POINT('Origin',(40.5,0.,0.));
#23506=CARTESIAN_POINT('Origin',(46.5,0.,-4.16333634234434E-16));
#23507=CARTESIAN_POINT('',(48.0857864376272,31.3127256445526,-65.2941922269197));
#23508=CARTESIAN_POINT('',(48.2311293298322,31.4232291358174,-64.9999999991507));
#23509=CARTESIAN_POINT('Ctrl Pts',(48.0857864376269,31.3127256445523,-65.29419222692));
#23510=CARTESIAN_POINT('Ctrl Pts',(48.1379693066647,31.3533479964789,-65.1994073067213));
#23511=CARTESIAN_POINT('Ctrl Pts',(48.1867097226798,31.3902501843818,-65.1012175564133));
#23512=CARTESIAN_POINT('Ctrl Pts',(48.2311293298322,31.4232291358174,-64.9999999991507));
#23513=CARTESIAN_POINT('',(48.0857864376269,30.6065287460451,65.6281854386855));
#23514=CARTESIAN_POINT('Origin',(48.0857864376269,0.,-4.16333634234434E-16));
#23515=CARTESIAN_POINT('',(48.5,29.0466953015038,65.0006740405345));
#23516=CARTESIAN_POINT('Ctrl Pts',(48.5,29.0466953013294,65.0006740505758));
#23517=CARTESIAN_POINT('Ctrl Pts',(48.4999999991287,29.2503863229646,65.0042110518181));
#23518=CARTESIAN_POINT('Ctrl Pts',(48.4947069418067,29.4582861404335,65.022120804513));
#23519=CARTESIAN_POINT('Ctrl Pts',(48.4614290981404,29.8188223615094,65.093668653765));
#23520=CARTESIAN_POINT('Ctrl Pts',(48.4373072643951,29.9796369412407,65.1412137624121));
#23521=CARTESIAN_POINT('Ctrl Pts',(48.3647629082104,30.2376016389712,65.2605302175309));
#23522=CARTESIAN_POINT('Ctrl Pts',(48.3231006418053,30.3406889822552,65.3242242320176));
#23523=CARTESIAN_POINT('Ctrl Pts',(48.2166759088974,30.5047262139872,65.4694903771709));
#23524=CARTESIAN_POINT('Ctrl Pts',(48.1563934129581,30.5653976622582,65.5459946552306));
#23525=CARTESIAN_POINT('Ctrl Pts',(48.0857864376269,30.6065287460451,65.6281854386855));
#23526=CARTESIAN_POINT('',(48.5,31.2619954337637,-63.9647228889383));
#23527=CARTESIAN_POINT('Origin',(48.5,0.,-4.16333634234434E-16));
#23528=CARTESIAN_POINT('Ctrl Pts',(48.2311293298322,31.4232291358174,-64.9999999991507));
#23529=CARTESIAN_POINT('Ctrl Pts',(48.2715171949672,31.4532147553691,-64.9079694452346));
#23530=CARTESIAN_POINT('Ctrl Pts',(48.3105502826012,31.4736788152368,-64.8122557494851));
#23531=CARTESIAN_POINT('Ctrl Pts',(48.3948971358411,31.4925877457303,-64.5781032722722));
#23532=CARTESIAN_POINT('Ctrl Pts',(48.4357433706305,31.479360669589,-64.4404239144226));
#23533=CARTESIAN_POINT('Ctrl Pts',(48.4876874516577,31.3991541018519,-64.1828530709004));
#23534=CARTESIAN_POINT('Ctrl Pts',(48.5,31.3397623793345,-64.0691058819803));
#23535=CARTESIAN_POINT('Ctrl Pts',(48.5,31.261995430077,-63.9647228854568));
#23536=CARTESIAN_POINT('Origin',(48.5,53.,0.));
#23537=CARTESIAN_POINT('',(48.5,28.9686269665969,65.));
#23538=CARTESIAN_POINT('Ctrl Pts',(48.5,29.0466953013294,65.0006740505758));
#23539=CARTESIAN_POINT('Ctrl Pts',(48.5,29.0203628803793,65.0002168001558));
#23540=CARTESIAN_POINT('Ctrl Pts',(48.5,28.9943212164188,65.));
#23541=CARTESIAN_POINT('Ctrl Pts',(48.5,28.9686269665969,65.));
#23542=CARTESIAN_POINT('',(48.5,20.6143782776615,65.));
#23543=CARTESIAN_POINT('',(48.5,26.5,65.));
#23544=CARTESIAN_POINT('',(48.5,20.6143782776615,-77.));
#23545=CARTESIAN_POINT('',(48.5,20.6143782776615,-63.));
#23546=CARTESIAN_POINT('',(48.5,20.6143782776615,-77.));
#23547=CARTESIAN_POINT('',(48.5,28.9686269665969,-63.));
#23548=CARTESIAN_POINT('',(48.5,26.5,-63.));
#23549=CARTESIAN_POINT('Ctrl Pts',(48.5,28.9686269665969,-63.));
#23550=CARTESIAN_POINT('Ctrl Pts',(48.5,29.3555738612142,-63.));
#23551=CARTESIAN_POINT('Ctrl Pts',(48.5,29.8155012575532,-63.0638354527098));
#23552=CARTESIAN_POINT('Ctrl Pts',(48.5,30.4573223491148,-63.2950310532685));
#23553=CARTESIAN_POINT('Ctrl Pts',(48.5,30.7662183987536,-63.4685459818617));
#23554=CARTESIAN_POINT('Ctrl Pts',(48.5,31.0821687424774,-63.7502960288675));
#23555=CARTESIAN_POINT('Ctrl Pts',(48.5,31.1786502720937,-63.8528525155057));
#23556=CARTESIAN_POINT('Ctrl Pts',(48.5,31.2619954330609,-63.964722889462));
#23557=CARTESIAN_POINT('',(48.5,31.,-49.1935750346352));
#23558=CARTESIAN_POINT('Origin',(48.5,31.,-53.6935750346352));
#23559=CARTESIAN_POINT('',(48.5,31.,58.1935750346352));
#23560=CARTESIAN_POINT('Origin',(48.5,31.,53.6935750346352));
#23561=CARTESIAN_POINT('',(48.5,62.,4.5));
#23562=CARTESIAN_POINT('Origin',(48.5,62.,0.));
#23563=CARTESIAN_POINT('Origin',(46.6715728752538,0.,0.));
#23564=CARTESIAN_POINT('Ctrl Pts',(48.0857864376269,30.6065287460451,65.6281854386856));
#23565=CARTESIAN_POINT('Ctrl Pts',(47.9999019239268,30.6339819569562,65.7101473578198));
#23566=CARTESIAN_POINT('Ctrl Pts',(47.9086549996909,30.6381886023579,65.791498635381));
#23567=CARTESIAN_POINT('Ctrl Pts',(47.6860457696345,30.606362608182,65.9774777549062));
#23568=CARTESIAN_POINT('Ctrl Pts',(47.5541390304854,30.5542981832038,66.0778114080422));
#23569=CARTESIAN_POINT('Ctrl Pts',(47.244379598631,30.3822100790379,66.2963162354507));
#23570=CARTESIAN_POINT('Ctrl Pts',(47.0481190367442,30.2289549206708,66.4196105770725));
#23571=CARTESIAN_POINT('Ctrl Pts',(46.7881288893781,29.9653860177436,66.5635667604956));
#23572=CARTESIAN_POINT('Ctrl Pts',(46.7298294631265,29.9024655481068,66.5946537999311));
#23573=CARTESIAN_POINT('Ctrl Pts',(46.6715728753514,29.8356437962676,66.6245777417181));
#23574=CARTESIAN_POINT('Ctrl Pts',(46.6715728752538,29.8939769234005,-66.5984244836407));
#23575=CARTESIAN_POINT('Ctrl Pts',(46.9438337493957,30.2460388819865,-66.440394738235));
#23576=CARTESIAN_POINT('Ctrl Pts',(47.2187895890396,30.5412296642388,-66.2435626590178));
#23577=CARTESIAN_POINT('Ctrl Pts',(47.7030292472569,31.0032903130161,-65.7928556068471));
#23578=CARTESIAN_POINT('Ctrl Pts',(47.9098828723248,31.1757914999452,-65.5549458876211));
#23579=CARTESIAN_POINT('Ctrl Pts',(48.0857864376305,31.3127256445551,-65.2941922269146));
#23580=CARTESIAN_POINT('Origin',(40.5,0.,0.));
#23581=CARTESIAN_POINT('',(38.5,-71.,-1.73899845478924E-14));
#23582=CARTESIAN_POINT('Origin',(40.5,-71.,0.));
#23583=CARTESIAN_POINT('Origin',(38.5,0.,0.));
#23584=CARTESIAN_POINT('Origin',(38.5,72.,0.));
#23585=CARTESIAN_POINT('',(38.5,-31.,-49.1935750346352));
#23586=CARTESIAN_POINT('Origin',(38.5,-31.,-53.6935750346352));
#23587=CARTESIAN_POINT('',(38.5,62.,4.5));
#23588=CARTESIAN_POINT('Origin',(38.5,62.,0.));
#23589=CARTESIAN_POINT('',(38.5,31.,58.1935750346352));
#23590=CARTESIAN_POINT('Origin',(38.5,31.,53.6935750346352));
#23591=CARTESIAN_POINT('',(38.5,-31.,58.1935750346352));
#23592=CARTESIAN_POINT('Origin',(38.5,-31.,53.6935750346352));
#23593=CARTESIAN_POINT('',(38.5,-62.,4.50000000000001));
#23594=CARTESIAN_POINT('Origin',(38.5,-62.,7.59281015471359E-15));
#23595=CARTESIAN_POINT('',(38.5,31.,-49.1935750346352));
#23596=CARTESIAN_POINT('Origin',(38.5,31.,-53.6935750346352));
#23597=CARTESIAN_POINT('',(38.5,-6.2659657814934E-15,51.1654934782503));
#23598=CARTESIAN_POINT('Origin',(38.5,0.,0.));
#23599=CARTESIAN_POINT('Origin',(53.,-25.,67.));
#23600=CARTESIAN_POINT('',(53.,-31.,65.));
#23601=CARTESIAN_POINT('Origin',(53.,-25.,65.));
#23602=CARTESIAN_POINT('',(53.,-33.,67.));
#23603=CARTESIAN_POINT('Origin',(53.,-31.,67.));
#23604=CARTESIAN_POINT('Origin',(53.,-25.,67.));
#23605=CARTESIAN_POINT('Origin',(57.,-31.,67.));
#23606=CARTESIAN_POINT('',(69.,-31.,65.));
#23607=CARTESIAN_POINT('',(69.,-33.,67.));
#23608=CARTESIAN_POINT('Origin',(69.,-31.,67.));
#23609=CARTESIAN_POINT('',(57.,-33.,67.));
#23610=CARTESIAN_POINT('',(57.,-31.,65.));
#23611=CARTESIAN_POINT('Origin',(69.,-25.,67.));
#23612=CARTESIAN_POINT('',(75.,-25.,65.));
#23613=CARTESIAN_POINT('',(77.,-25.,67.));
#23614=CARTESIAN_POINT('Origin',(75.,-25.,67.));
#23615=CARTESIAN_POINT('Origin',(69.,-25.,67.));
#23616=CARTESIAN_POINT('Origin',(69.,-25.,65.));
#23617=CARTESIAN_POINT('Origin',(75.,-7.,67.));
#23618=CARTESIAN_POINT('',(75.,-19.2915026221292,65.));
#23619=CARTESIAN_POINT('',(77.,-14.,67.));
#23620=CARTESIAN_POINT('Ctrl Pts',(77.,-14.,67.));
#23621=CARTESIAN_POINT('Ctrl Pts',(77.,-14.8922724470027,66.5538637764986));
#23622=CARTESIAN_POINT('Ctrl Pts',(76.8431824332822,-15.8525818385793,66.0701256324549));
#23623=CARTESIAN_POINT('Ctrl Pts',(76.1700160324087,-17.6794947918718,65.2991643782353));
#23624=CARTESIAN_POINT('Ctrl Pts',(75.6598443730912,-18.5433094298986,65.));
#23625=CARTESIAN_POINT('Ctrl Pts',(75.,-19.2915026221292,65.));
#23626=CARTESIAN_POINT('',(77.,-7.,67.));
#23627=CARTESIAN_POINT('',(75.,-7.,65.));
#23628=CARTESIAN_POINT('Origin',(77.,-14.,-77.));
#23629=CARTESIAN_POINT('',(77.,-14.,-77.));
#23630=CARTESIAN_POINT('',(77.,14.,67.));
#23631=CARTESIAN_POINT('',(77.,14.,-77.));
#23632=CARTESIAN_POINT('',(77.,25.,67.));
#23633=CARTESIAN_POINT('',(77.,-7.,67.));
#23634=CARTESIAN_POINT('',(77.,25.,80.));
#23635=CARTESIAN_POINT('',(77.,25.,65.));
#23636=CARTESIAN_POINT('',(77.,-25.,80.));
#23637=CARTESIAN_POINT('',(77.,-7.,80.));
#23638=CARTESIAN_POINT('',(77.,-25.,65.));
#23639=CARTESIAN_POINT('Origin',(61.,0.,65.));
#23640=CARTESIAN_POINT('',(53.,-22.,65.));
#23641=CARTESIAN_POINT('Origin',(53.,-14.,65.));
#23642=CARTESIAN_POINT('',(69.,-22.,65.));
#23643=CARTESIAN_POINT('',(57.,-22.,65.));
#23644=CARTESIAN_POINT('Origin',(69.,-14.,65.));
#23645=CARTESIAN_POINT('Origin',(75.,-7.,80.));
#23646=CARTESIAN_POINT('Origin',(75.,-25.,80.));
#23647=CARTESIAN_POINT('Origin',(75.,25.,80.));
#23648=CARTESIAN_POINT('Origin',(69.,25.,80.));
#23649=CARTESIAN_POINT('',(69.,33.,80.));
#23650=CARTESIAN_POINT('Origin',(69.,31.,80.));
#23651=CARTESIAN_POINT('Origin',(69.,25.,80.));
#23652=CARTESIAN_POINT('Origin',(65.,31.,80.));
#23653=CARTESIAN_POINT('',(53.,33.,80.));
#23654=CARTESIAN_POINT('Origin',(53.,31.,80.));
#23655=CARTESIAN_POINT('',(65.,33.,80.));
#23656=CARTESIAN_POINT('Origin',(53.,25.,80.));
#23657=CARTESIAN_POINT('',(45.,25.,80.));
#23658=CARTESIAN_POINT('Origin',(47.,25.,80.));
#23659=CARTESIAN_POINT('Origin',(53.,25.,80.));
#23660=CARTESIAN_POINT('Origin',(47.,7.,80.));
#23661=CARTESIAN_POINT('',(45.,-25.,80.));
#23662=CARTESIAN_POINT('Origin',(47.,-25.,80.));
#23663=CARTESIAN_POINT('',(45.,7.,80.));
#23664=CARTESIAN_POINT('Origin',(53.,-25.,80.));
#23665=CARTESIAN_POINT('',(53.,-33.,80.));
#23666=CARTESIAN_POINT('Origin',(53.,-31.,80.));
#23667=CARTESIAN_POINT('Origin',(53.,-25.,80.));
#23668=CARTESIAN_POINT('Origin',(57.,-31.,80.));
#23669=CARTESIAN_POINT('',(69.,-33.,80.));
#23670=CARTESIAN_POINT('Origin',(69.,-31.,80.));
#23671=CARTESIAN_POINT('',(57.,-33.,80.));
#23672=CARTESIAN_POINT('Origin',(69.,-25.,80.));
#23673=CARTESIAN_POINT('Origin',(69.,-25.,80.));
#23674=CARTESIAN_POINT('Origin',(53.,25.,65.));
#23675=CARTESIAN_POINT('',(53.,33.,67.));
#23676=CARTESIAN_POINT('',(53.,33.,65.));
#23677=CARTESIAN_POINT('Origin',(53.,25.,67.));
#23678=CARTESIAN_POINT('',(45.,25.,65.));
#23679=CARTESIAN_POINT('Origin',(69.,33.,65.));
#23680=CARTESIAN_POINT('',(69.,33.,67.));
#23681=CARTESIAN_POINT('',(69.,33.,65.));
#23682=CARTESIAN_POINT('',(65.,33.,67.));
#23683=CARTESIAN_POINT('Origin',(69.,25.,65.));
#23684=CARTESIAN_POINT('Origin',(69.,25.,67.));
#23685=CARTESIAN_POINT('Origin',(75.,-7.,67.));
#23686=CARTESIAN_POINT('',(75.,25.,65.));
#23687=CARTESIAN_POINT('Origin',(75.,25.,67.));
#23688=CARTESIAN_POINT('',(75.,19.2915026221292,65.));
#23689=CARTESIAN_POINT('Ctrl Pts',(75.,19.2915026221292,65.));
#23690=CARTESIAN_POINT('Ctrl Pts',(75.6598443730912,18.5433094298986,65.));
#23691=CARTESIAN_POINT('Ctrl Pts',(76.1700160324087,17.6794947918718,65.2991643782352));
#23692=CARTESIAN_POINT('Ctrl Pts',(76.8431824332822,15.8525818385793,66.0701256324549));
#23693=CARTESIAN_POINT('Ctrl Pts',(77.,14.8922724470027,66.5538637764986));
#23694=CARTESIAN_POINT('Ctrl Pts',(77.,14.,67.));
#23695=CARTESIAN_POINT('',(75.,-7.,65.));
#23696=CARTESIAN_POINT('Origin',(65.,31.,67.));
#23697=CARTESIAN_POINT('',(69.,31.,65.));
#23698=CARTESIAN_POINT('Origin',(69.,31.,67.));
#23699=CARTESIAN_POINT('',(53.,31.,65.));
#23700=CARTESIAN_POINT('',(65.,31.,65.));
#23701=CARTESIAN_POINT('Origin',(53.,31.,67.));
#23702=CARTESIAN_POINT('Origin',(53.,25.,67.));
#23703=CARTESIAN_POINT('Origin',(53.,25.,65.));
#23704=CARTESIAN_POINT('Origin',(69.,25.,67.));
#23705=CARTESIAN_POINT('Origin',(69.,25.,65.));
#23706=CARTESIAN_POINT('Origin',(61.,0.,65.));
#23707=CARTESIAN_POINT('',(69.,22.,65.));
#23708=CARTESIAN_POINT('Origin',(69.,14.,65.));
#23709=CARTESIAN_POINT('',(53.,22.,65.));
#23710=CARTESIAN_POINT('',(65.,22.,65.));
#23711=CARTESIAN_POINT('Origin',(53.,14.,65.));
#23712=CARTESIAN_POINT('Origin',(40.5,0.,0.));
#23713=CARTESIAN_POINT('',(39.5811541622525,-6.04841520276597E-15,49.3890581919384));
#23714=CARTESIAN_POINT('Origin',(40.5,-6.2659657814934E-15,51.1654934782503));
#23715=CARTESIAN_POINT('',(39.5811541622525,-49.3890581919384,-1.20968304055319E-14));
#23716=CARTESIAN_POINT('Origin',(39.5811541622525,0.,-3.02420760138299E-15));
#23717=CARTESIAN_POINT('Origin',(39.5811541622525,0.,-3.02420760138299E-15));
#23718=CARTESIAN_POINT('Origin',(44.2,0.,0.));
#23719=CARTESIAN_POINT('',(50.,-44.,-5.38844591624836E-15));
#23720=CARTESIAN_POINT('',(44.2,-47.,-5.75583995599256E-15));
#23721=CARTESIAN_POINT('Origin',(50.,0.,0.));
#23722=CARTESIAN_POINT('Ctrl Pts',(63.3333333333333,-6.59966329107444,-31.7128621774316));
#23723=CARTESIAN_POINT('Ctrl Pts',(62.1773896945574,-7.00835108389839,-33.1107619749047));
#23724=CARTESIAN_POINT('Ctrl Pts',(59.8510477373174,-7.17140712600759,-36.1605129538655));
#23725=CARTESIAN_POINT('Ctrl Pts',(57.183782288428,-6.08047773499016,-40.0089544705698));
#23726=CARTESIAN_POINT('Ctrl Pts',(55.3668393528774,-4.31463467556344,-42.7323184706779));
#23727=CARTESIAN_POINT('Ctrl Pts',(54.4252091326635,-2.64874627344738,-44.1725365377487));
#23728=CARTESIAN_POINT('Ctrl Pts',(53.9842199476096,-0.833885651421998,
-44.8528004529788));
#23729=CARTESIAN_POINT('Ctrl Pts',(53.9856754786376,0.833929869935245,-44.8504853272497));
#23730=CARTESIAN_POINT('Ctrl Pts',(54.3607684393205,2.38775013614543,-44.2719711995386));
#23731=CARTESIAN_POINT('Ctrl Pts',(55.2216130985053,4.14017606552555,-42.9536995244691));
#23732=CARTESIAN_POINT('Ctrl Pts',(57.007705320374,6.00979472992292,-40.2625095891802));
#23733=CARTESIAN_POINT('Ctrl Pts',(59.8499534347117,7.17041001211291,-36.1623598714334));
#23734=CARTESIAN_POINT('Ctrl Pts',(62.177413277237,7.00834274616208,-33.1107334560203));
#23735=CARTESIAN_POINT('Ctrl Pts',(63.3333333333333,6.59966329107444,-31.7128621774316));
#23736=CARTESIAN_POINT('Ctrl Pts',(63.1962492273341,-6.64812984154691,-31.5488996087769));
#23737=CARTESIAN_POINT('Ctrl Pts',(62.0093421297043,-7.04072991080625,-32.9391773083993));
#23738=CARTESIAN_POINT('Ctrl Pts',(59.6306065410736,-7.14633030805639,-35.9670953227804));
#23739=CARTESIAN_POINT('Ctrl Pts',(56.9648786541832,-5.94451145070926,-39.762309829984));
#23740=CARTESIAN_POINT('Ctrl Pts',(55.2199817816534,-4.11869812402828,-42.409002614623));
#23741=CARTESIAN_POINT('Ctrl Pts',(54.3627838804906,-2.46985625068407,-43.7767782773241));
#23742=CARTESIAN_POINT('Ctrl Pts',(53.9869023625283,-0.76523709649401,-44.4022656717365));
#23743=CARTESIAN_POINT('Ctrl Pts',(53.9876569730852,0.765132497213866,-44.4005227560803));
#23744=CARTESIAN_POINT('Ctrl Pts',(54.308269419325,2.22454580031585,-43.8679449989279));
#23745=CARTESIAN_POINT('Ctrl Pts',(55.0839094544005,3.93929433219883,-42.6222903885058));
#23746=CARTESIAN_POINT('Ctrl Pts',(56.7877816472993,5.86696731444184,-40.0130840027767));
#23747=CARTESIAN_POINT('Ctrl Pts',(59.6300671008111,7.14497282840818,-35.9685572168257));
#23748=CARTESIAN_POINT('Ctrl Pts',(62.0093663440767,7.04072190127938,-32.9391489450152));
#23749=CARTESIAN_POINT('Ctrl Pts',(63.1962492273341,6.64812984154691,-31.5488996087769));
#23750=CARTESIAN_POINT('Ctrl Pts',(62.9463311105498,-6.81360008562125,-31.2209941996293));
#23751=CARTESIAN_POINT('Ctrl Pts',(61.6902590726639,-7.19193133539315,-32.5959957954705));
#23752=CARTESIAN_POINT('Ctrl Pts',(59.1806872784941,-7.22378666187567,-35.5805956265476));
#23753=CARTESIAN_POINT('Ctrl Pts',(56.4330578953553,-5.84073365634425,-39.2697533297976));
#23754=CARTESIAN_POINT('Ctrl Pts',(54.7292640216373,-3.8844953708936,-41.7632573520683));
#23755=CARTESIAN_POINT('Ctrl Pts',(53.965245234288,-2.22567623138461,-42.9858057638349));
#23756=CARTESIAN_POINT('Ctrl Pts',(53.6755658826225,-0.666505530006447,
-43.501384002397));
#23757=CARTESIAN_POINT('Ctrl Pts',(53.6752225587962,0.6661183946874,-43.5007858534596));
#23758=CARTESIAN_POINT('Ctrl Pts',(53.9239413145957,2.00085102106527,-43.0603333980273));
#23759=CARTESIAN_POINT('Ctrl Pts',(54.6011329384079,3.69297684653767,-41.9602076461288));
#23760=CARTESIAN_POINT('Ctrl Pts',(56.2489427064185,5.75229252847979,-39.5150983136102));
#23761=CARTESIAN_POINT('Ctrl Pts',(59.1809320219284,7.22165892747492,-35.5812660792604));
#23762=CARTESIAN_POINT('Ctrl Pts',(61.6902846980866,7.19192361696785,-32.5959677437378));
#23763=CARTESIAN_POINT('Ctrl Pts',(62.9463311105498,6.81360008562125,-31.2209941996293));
#23764=CARTESIAN_POINT('Ctrl Pts',(62.7061595886978,-7.20521258113835,-30.8184466564059));
#23765=CARTESIAN_POINT('Ctrl Pts',(61.3525918084501,-7.61031511383114,-32.1841418341022));
#23766=CARTESIAN_POINT('Ctrl Pts',(58.6397135353473,-7.65456619081017,-35.1410675266432));
#23767=CARTESIAN_POINT('Ctrl Pts',(55.637456029258,-6.19006620504293,-38.7682879574204));
#23768=CARTESIAN_POINT('Ctrl Pts',(53.7521005295524,-4.10520928504339,-41.1834647166237));
#23769=CARTESIAN_POINT('Ctrl Pts',(52.896526947302,-2.33958599845526,-42.3384335758014));
#23770=CARTESIAN_POINT('Ctrl Pts',(52.5690532918678,-0.69710377877861,-42.8061313896708));
#23771=CARTESIAN_POINT('Ctrl Pts',(52.5687476409763,0.696653785021548,-42.8059981646796));
#23772=CARTESIAN_POINT('Ctrl Pts',(52.8497229834458,2.1025880600763,-42.405744459455));
#23773=CARTESIAN_POINT('Ctrl Pts',(53.6092348807766,3.90049216650729,-41.3724241088537));
#23774=CARTESIAN_POINT('Ctrl Pts',(55.4364449073139,6.09674247261476,-39.0101551866323));
#23775=CARTESIAN_POINT('Ctrl Pts',(58.6398745251078,7.65211573990002,-35.1414067287986));
#23776=CARTESIAN_POINT('Ctrl Pts',(61.3526194229065,7.61030684923857,-32.1841139722319));
#23777=CARTESIAN_POINT('Ctrl Pts',(62.7061595886978,7.20521258113835,-30.8184466564059));
#23778=CARTESIAN_POINT('Ctrl Pts',(62.5904039193511,-7.6583127936691,-30.5250624561552));
#23779=CARTESIAN_POINT('Ctrl Pts',(61.1584933846712,-8.11585881641404,-31.8989848492516));
#23780=CARTESIAN_POINT('Ctrl Pts',(58.2791899818164,-8.24150163010199,-34.8759107492543));
#23781=CARTESIAN_POINT('Ctrl Pts',(55.0265173915859,-6.82101714568871,-38.556644545297));
#23782=CARTESIAN_POINT('Ctrl Pts',(52.8925220087755,-4.67295100884693,-41.0601803137195));
#23783=CARTESIAN_POINT('Ctrl Pts',(51.8521821945375,-2.76155870131978,-42.3047892112534));
#23784=CARTESIAN_POINT('Ctrl Pts',(51.4059828265007,-0.845790495339543,
-42.843015607466));
#23785=CARTESIAN_POINT('Ctrl Pts',(51.4066822856346,0.845549070264003,-42.8421168527233));
#23786=CARTESIAN_POINT('Ctrl Pts',(51.7875421911392,2.48554240511298,-42.382782492684));
#23787=CARTESIAN_POINT('Ctrl Pts',(52.7260106805419,4.46114907550238,-41.2588268883627));
#23788=CARTESIAN_POINT('Ctrl Pts',(54.8102735447582,6.7299823631145,-38.8010166853369));
#23789=CARTESIAN_POINT('Ctrl Pts',(58.2786008454734,8.23949994358309,-34.8767640575889));
#23790=CARTESIAN_POINT('Ctrl Pts',(61.1585225974167,8.11584948190943,-31.8989568195359));
#23791=CARTESIAN_POINT('Ctrl Pts',(62.5904039193511,7.6583127936691,-30.5250624561552));
#23792=CARTESIAN_POINT('Ctrl Pts',(62.5777174765495,-7.9634392868377,-30.3968807187894));
#23793=CARTESIAN_POINT('Ctrl Pts',(61.1076965731432,-8.46164972651616,-31.7860405531774));
#23794=CARTESIAN_POINT('Ctrl Pts',(58.1491913574022,-8.6588051165908,-34.8022816412753));
#23795=CARTESIAN_POINT('Ctrl Pts',(54.770406003722,-7.30098646822153,-38.5745581184182));
#23796=CARTESIAN_POINT('Ctrl Pts',(52.4937591618684,-5.13053317476476,-41.2071453587244));
#23797=CARTESIAN_POINT('Ctrl Pts',(51.3345717216213,-3.11536681555036,-42.5713405178562));
#23798=CARTESIAN_POINT('Ctrl Pts',(50.80489364747,-0.973086475418704,-43.1985149672608));
#23799=CARTESIAN_POINT('Ctrl Pts',(50.8063933838826,0.973031903179425,-43.1967026130617));
#23800=CARTESIAN_POINT('Ctrl Pts',(51.2573520876146,2.80710953729802,-42.6627697753439));
#23801=CARTESIAN_POINT('Ctrl Pts',(52.3130437902742,4.91587606463395,-41.419363544675));
#23802=CARTESIAN_POINT('Ctrl Pts',(54.5468818639601,7.21342605270668,-38.8237752884765));
#23803=CARTESIAN_POINT('Ctrl Pts',(58.1480381345749,8.65729203243944,-34.8037642919162));
#23804=CARTESIAN_POINT('Ctrl Pts',(61.1077265633873,8.46163956240716,-31.7860122125991));
#23805=CARTESIAN_POINT('Ctrl Pts',(62.5777174765495,7.9634392868377,-30.3968807187894));
#23806=CARTESIAN_POINT('Ctrl Pts',(62.5857864376269,-8.11974451941452,-30.3467059609741));
#23807=CARTESIAN_POINT('Ctrl Pts',(61.0995731877722,-8.63911281829804,-31.74623454857));
#23808=CARTESIAN_POINT('Ctrl Pts',(58.1085620998922,-8.87362866313132,-34.7889742482164));
#23809=CARTESIAN_POINT('Ctrl Pts',(54.6792208084628,-7.54849040484405,-38.6195517001502));
#23810=CARTESIAN_POINT('Ctrl Pts',(52.3431513198979,-5.36616124891415,-41.3291120736047));
#23811=CARTESIAN_POINT('Ctrl Pts',(51.1324838939085,-3.29727471161762,-42.7617756824825));
#23812=CARTESIAN_POINT('Ctrl Pts',(50.5654977988392,-1.03845908333126,-43.438457668019));
#23813=CARTESIAN_POINT('Ctrl Pts',(50.5673691958753,1.03851583598142,-43.4361543056794));
#23814=CARTESIAN_POINT('Ctrl Pts',(51.0496315738962,2.97241028941536,-42.8606883506125));
#23815=CARTESIAN_POINT('Ctrl Pts',(52.1564318499909,5.14998354500412,-41.5493290169032));
#23816=CARTESIAN_POINT('Ctrl Pts',(54.4528361352506,7.46272682506624,-38.871938946387));
#23817=CARTESIAN_POINT('Ctrl Pts',(58.1071551393991,8.87236958524201,-34.7908086217603));
#23818=CARTESIAN_POINT('Ctrl Pts',(61.0996035083602,8.63910222254254,-31.7462059964563));
#23819=CARTESIAN_POINT('Ctrl Pts',(62.5857864376269,8.11974451941452,-30.3467059609741));
#23820=CARTESIAN_POINT('',(62.0001023839998,8.30322829225476,-30.9040904042794));
#23821=CARTESIAN_POINT('',(62.0001200040293,-8.30324353871505,-30.9040671432868));
#23822=CARTESIAN_POINT('Ctrl Pts',(62.0001012510352,8.30322731523632,-30.9040918407253));
#23823=CARTESIAN_POINT('Ctrl Pts',(61.5941099144469,8.41601233957157,-31.294418998263));
#23824=CARTESIAN_POINT('Ctrl Pts',(61.1881353144704,8.49983265749143,-31.6926113194296));
#23825=CARTESIAN_POINT('Ctrl Pts',(60.7837478174969,8.55624046373246,-32.0961848387561));
#23826=CARTESIAN_POINT('Ctrl Pts',(60.3590806981778,8.61547706417824,-32.5199971602756));
#23827=CARTESIAN_POINT('Ctrl Pts',(59.9361642491327,8.64448288128927,-32.9497439708323));
#23828=CARTESIAN_POINT('Ctrl Pts',(59.5168590726499,8.64506377982343,-33.3825098937528));
#23829=CARTESIAN_POINT('Ctrl Pts',(59.2963181027409,8.6453693136764,-33.6101307812053));
#23830=CARTESIAN_POINT('Ctrl Pts',(59.0767768036617,8.63781144485083,-33.8385862524986));
#23831=CARTESIAN_POINT('Ctrl Pts',(58.858509746758,8.62265371547609,-34.0674479590845));
#23832=CARTESIAN_POINT('Ctrl Pts',(58.6277262935084,8.60662677500166,-34.3094336059876));
#23833=CARTESIAN_POINT('Ctrl Pts',(58.39818772758,8.58201871678512,-34.5520800845962));
#23834=CARTESIAN_POINT('Ctrl Pts',(58.1701981943553,8.5491694637154,-34.7948922255947));
#23835=CARTESIAN_POINT('Ctrl Pts',(57.8329926670629,8.50058412058207,-35.1540209754116));
#23836=CARTESIAN_POINT('Ctrl Pts',(57.4991770870744,8.43396948207508,-35.5135109022731));
#23837=CARTESIAN_POINT('Ctrl Pts',(57.1696794849973,8.34871184595084,-35.8717709918078));
#23838=CARTESIAN_POINT('Ctrl Pts',(56.8493772762383,8.26583352151987,-36.2200330042316));
#23839=CARTESIAN_POINT('Ctrl Pts',(56.5331556928524,8.16533894646567,-36.5671321395276));
#23840=CARTESIAN_POINT('Ctrl Pts',(56.2218388148571,8.04669241324987,-36.9116334654208));
#23841=CARTESIAN_POINT('Ctrl Pts',(55.9343240716864,7.93711715428765,-37.2297954965771));
#23842=CARTESIAN_POINT('Ctrl Pts',(55.6509928326656,7.81206045781843,-37.5457413038118));
#23843=CARTESIAN_POINT('Ctrl Pts',(55.3724670951342,7.67111227501838,-37.858371532471));
#23844=CARTESIAN_POINT('Ctrl Pts',(55.1989249042423,7.58329110394045,-38.0531633506399));
#23845=CARTESIAN_POINT('Ctrl Pts',(55.0272477780776,7.48930072219156,-38.2466686113815));
#23846=CARTESIAN_POINT('Ctrl Pts',(54.8575797184335,7.38904192488208,-38.4386296303125));
#23847=CARTESIAN_POINT('Ctrl Pts',(54.6442441141775,7.26297947593995,-38.679995742786));
#23848=CARTESIAN_POINT('Ctrl Pts',(54.4345041567674,7.12692432952911,-38.9185103314235));
#23849=CARTESIAN_POINT('Ctrl Pts',(54.2285146699767,6.98061592018927,-39.1538065157717));
#23850=CARTESIAN_POINT('Ctrl Pts',(54.1954395384656,6.9571236053363,-39.1915873382915));
#23851=CARTESIAN_POINT('Ctrl Pts',(54.1624611267774,6.93336683779831,-39.2292851714087));
#23852=CARTESIAN_POINT('Ctrl Pts',(54.1295801071056,6.90934441644494,-39.2668984787726));
#23853=CARTESIAN_POINT('Ctrl Pts',(53.9349114980075,6.76712220440003,-39.4895840980498));
#23854=CARTESIAN_POINT('Ctrl Pts',(53.7436555827443,6.61559218141993,-39.7093077515375));
#23855=CARTESIAN_POINT('Ctrl Pts',(53.5567634172599,6.45410520199659,-39.9248076943406));
#23856=CARTESIAN_POINT('Ctrl Pts',(53.3801976129847,6.30154086989652,-40.1284006091302));
#23857=CARTESIAN_POINT('Ctrl Pts',(53.2075261217369,6.1400895378134,-40.3282244049943));
#23858=CARTESIAN_POINT('Ctrl Pts',(53.0395671024636,5.96916334439465,-40.5231997797519));
#23859=CARTESIAN_POINT('Ctrl Pts',(52.8822480606121,5.80906509487933,-40.7058237273925));
#23860=CARTESIAN_POINT('Ctrl Pts',(52.7290630593257,5.64065439307646,-40.8841944917208));
#23861=CARTESIAN_POINT('Ctrl Pts',(52.580704568405,5.46341141043919,-41.0574035177952));
#23862=CARTESIAN_POINT('Ctrl Pts',(52.5706706209874,5.45142391476649,-41.0691181844051));
#23863=CARTESIAN_POINT('Ctrl Pts',(52.5606587602156,5.43939600328583,-41.0808092299468));
#23864=CARTESIAN_POINT('Ctrl Pts',(52.5506692043932,5.42732750858862,-41.0924763687869));
#23865=CARTESIAN_POINT('Ctrl Pts',(52.326146367373,5.15607894497275,-41.3547041553726));
#23866=CARTESIAN_POINT('Ctrl Pts',(52.1134246130853,4.86497441262733,-41.604231853927));
#23867=CARTESIAN_POINT('Ctrl Pts',(51.9150764404737,4.55261153092244,-41.8377049019999));
#23868=CARTESIAN_POINT('Ctrl Pts',(51.6817907972624,4.18522838433518,-42.1123023912283));
#23869=CARTESIAN_POINT('Ctrl Pts',(51.4683897034793,3.78844091406138,-42.3646895021457));
#23870=CARTESIAN_POINT('Ctrl Pts',(51.2842097158458,3.36345268041168,-42.5830775379464));
#23871=CARTESIAN_POINT('Ctrl Pts',(51.2218736018392,3.21961449622777,-42.6569914396263));
#23872=CARTESIAN_POINT('Ctrl Pts',(51.1628846200672,3.07254551732303,-42.7270109645469));
#23873=CARTESIAN_POINT('Ctrl Pts',(51.1076045454045,2.92229120412496,-42.79267942641));
#23874=CARTESIAN_POINT('Ctrl Pts',(51.0777650817789,2.84118588470146,-42.8281264060148));
#23875=CARTESIAN_POINT('Ctrl Pts',(51.0490066311153,2.7591539419897,-42.8623052012408));
#23876=CARTESIAN_POINT('Ctrl Pts',(51.0213793428822,2.67624432063873,-42.8951530087209));
#23877=CARTESIAN_POINT('Ctrl Pts',(50.93401383815,2.41406003185287,-42.9990273106656));
#23878=CARTESIAN_POINT('Ctrl Pts',(50.8579717898991,2.14313439968825,-43.0895777141708));
#23879=CARTESIAN_POINT('Ctrl Pts',(50.7950448077893,1.86551417994214,-43.1645736822976));
#23880=CARTESIAN_POINT('Ctrl Pts',(50.7635813167345,1.72670407006909,-43.202071666361));
#23881=CARTESIAN_POINT('Ctrl Pts',(50.7353969825947,1.58622028876809,-43.2356805725728));
#23882=CARTESIAN_POINT('Ctrl Pts',(50.7107183655813,1.44431884754542,-43.2651184376449));
#23883=CARTESIAN_POINT('Ctrl Pts',(50.6978982060417,1.37060324531452,-43.2804109528828));
#23884=CARTESIAN_POINT('Ctrl Pts',(50.6860241446869,1.29650507187844,-43.2945778164074));
#23885=CARTESIAN_POINT('Ctrl Pts',(50.6751281526797,1.22206025810523,-43.3075792459665));
#23886=CARTESIAN_POINT('Ctrl Pts',(50.6688327119529,1.1790478447136,-43.3150911576032));
#23887=CARTESIAN_POINT('Ctrl Pts',(50.6628638943807,1.13592001508024,-43.3222138760624));
#23888=CARTESIAN_POINT('Ctrl Pts',(50.657229426006,1.09269727206875,-43.3289378665353));
#23889=CARTESIAN_POINT('Ctrl Pts',(50.6538434412765,1.06672294085045,-43.332978590087));
#23890=CARTESIAN_POINT('Ctrl Pts',(50.6505780086374,1.04071306381805,-43.3368755494295));
#23891=CARTESIAN_POINT('Ctrl Pts',(50.6474343593728,1.01466909166829,-43.3406272068915));
#23892=CARTESIAN_POINT('Ctrl Pts',(50.6186694791588,0.776362691650125,-43.3749554567736));
#23893=CARTESIAN_POINT('Ctrl Pts',(50.600098342512,0.535203459559028,-43.3971213719785));
#23894=CARTESIAN_POINT('Ctrl Pts',(50.5917367840456,0.293243554386321,-43.4071042335405));
#23895=CARTESIAN_POINT('Ctrl Pts',(50.5883618175051,0.195581547070637,-43.4111336048456));
#23896=CARTESIAN_POINT('Ctrl Pts',(50.5866505170883,0.0977888671166625,
-43.4131777294003));
#23897=CARTESIAN_POINT('Ctrl Pts',(50.5866053901866,-2.17691642161351E-7,
-43.4132334956971));
#23898=CARTESIAN_POINT('Ctrl Pts',(50.586485167316,-0.260520750748842,-43.413382063049));
#23899=CARTESIAN_POINT('Ctrl Pts',(50.5982467100744,-0.521104937388154,
-43.3993625324755));
#23900=CARTESIAN_POINT('Ctrl Pts',(50.6219681403998,-0.77917008619531,-43.3710763758922));
#23901=CARTESIAN_POINT('Ctrl Pts',(50.6292153817941,-0.858012736203985,
-43.3624345443474));
#23902=CARTESIAN_POINT('Ctrl Pts',(50.6375791839474,-0.936620275249521,
-43.3524608025752));
#23903=CARTESIAN_POINT('Ctrl Pts',(50.6470624139535,-1.01491901366598,-43.3411515885966));
#23904=CARTESIAN_POINT('Ctrl Pts',(50.6472813846526,-1.01672695563096,-43.3408904553657));
#23905=CARTESIAN_POINT('Ctrl Pts',(50.6475009522024,-1.01853473295156,-43.3406286100948));
#23906=CARTESIAN_POINT('Ctrl Pts',(50.6477211161207,-1.02034234510595,-43.3403660533829));
#23907=CARTESIAN_POINT('Ctrl Pts',(50.673528927452,-1.23223225784476,-43.3095889208865));
#23908=CARTESIAN_POINT('Ctrl Pts',(50.7073631779969,-1.44168968568162,-43.2692082735287));
#23909=CARTESIAN_POINT('Ctrl Pts',(50.7484990707422,-1.64787039720256,-43.220143263679));
#23910=CARTESIAN_POINT('Ctrl Pts',(50.7921321138407,-1.86656728868811,-43.1680997671963));
#23911=CARTESIAN_POINT('Ctrl Pts',(50.84398110902,-2.08157734702968,-43.1062843533602));
#23912=CARTESIAN_POINT('Ctrl Pts',(50.9031825382286,-2.29183416733726,-43.0357934194958));
#23913=CARTESIAN_POINT('Ctrl Pts',(50.9292756216388,-2.3845050508477,-43.0047244767089));
#23914=CARTESIAN_POINT('Ctrl Pts',(50.9567969317084,-2.47625184720333,-42.9719703202599));
#23915=CARTESIAN_POINT('Ctrl Pts',(50.9856720258372,-2.56698024296232,-42.9376255742626));
#23916=CARTESIAN_POINT('Ctrl Pts',(51.0240408230126,-2.68753879073323,-42.8919887847397));
#23917=CARTESIAN_POINT('Ctrl Pts',(51.0648054205121,-2.8063940980028,-42.8435323454503));
#23918=CARTESIAN_POINT('Ctrl Pts',(51.1077731615943,-2.92331062745625,-42.7924952486978));
#23919=CARTESIAN_POINT('Ctrl Pts',(51.186049359457,-3.13630254098097,-42.6995187555632));
#23920=CARTESIAN_POINT('Ctrl Pts',(51.2716388252896,-3.34285777520948,-42.5979758659837));
#23921=CARTESIAN_POINT('Ctrl Pts',(51.3636626458657,-3.54285994422824,-42.4889780171507));
#23922=CARTESIAN_POINT('Ctrl Pts',(51.4604494463671,-3.75321384946142,-42.3743386446051));
#23923=CARTESIAN_POINT('Ctrl Pts',(51.5643534413362,-3.95631874229753,-42.2514532460909));
#23924=CARTESIAN_POINT('Ctrl Pts',(51.6743212746164,-4.15207844084002,-42.1216502585922));
#23925=CARTESIAN_POINT('Ctrl Pts',(51.793622211243,-4.36445250235611,-41.9808307341585));
#23926=CARTESIAN_POINT('Ctrl Pts',(51.9200593333631,-4.56818133269484,-41.8318704331003));
#23927=CARTESIAN_POINT('Ctrl Pts',(52.0522607572722,-4.76319042120215,-41.6764946462579));
#23928=CARTESIAN_POINT('Ctrl Pts',(52.1216221833531,-4.865504814479,-41.5949744490078));
#23929=CARTESIAN_POINT('Ctrl Pts',(52.1925699964374,-4.96541970222067,-41.5116886236485));
#23930=CARTESIAN_POINT('Ctrl Pts',(52.264904452046,-5.06292947504769,-41.4268878241172));
#23931=CARTESIAN_POINT('Ctrl Pts',(52.312104038938,-5.12655642788292,-41.3715537143584));
#23932=CARTESIAN_POINT('Ctrl Pts',(52.3599223500288,-5.18918440397153,-41.3155429681556));
#23933=CARTESIAN_POINT('Ctrl Pts',(52.4083099354638,-5.25081325409878,-41.25891856032));
#23934=CARTESIAN_POINT('Ctrl Pts',(52.7176297514124,-5.64477845006965,-40.8969444867553));
#23935=CARTESIAN_POINT('Ctrl Pts',(53.0502141797102,-5.99791651902043,-40.5098908689843));
#23936=CARTESIAN_POINT('Ctrl Pts',(53.3996025180074,-6.31470393262302,-40.1062255542024));
#23937=CARTESIAN_POINT('Ctrl Pts',(53.6358531256194,-6.52891033490946,-39.8332737540538));
#23938=CARTESIAN_POINT('Ctrl Pts',(53.8797866873093,-6.7264958123545,-39.5527271279448));
#23939=CARTESIAN_POINT('Ctrl Pts',(54.1293982844213,-6.90884160725303,-39.2672150609152));
#23940=CARTESIAN_POINT('Ctrl Pts',(54.2994416340632,-7.03306135551964,-39.0727151706752));
#23941=CARTESIAN_POINT('Ctrl Pts',(54.4721197328197,-7.15020875091379,-38.8759113199701));
#23942=CARTESIAN_POINT('Ctrl Pts',(54.6472513236306,-7.26040146543055,-38.6771162244914));
#23943=CARTESIAN_POINT('Ctrl Pts',(54.9699633495794,-7.46345172028084,-38.3107998579607));
#23944=CARTESIAN_POINT('Ctrl Pts',(55.3004435195228,-7.64300727204081,-37.9382715990561));
#23945=CARTESIAN_POINT('Ctrl Pts',(55.6375976843359,-7.79988175928238,-37.5614333033218));
#23946=CARTESIAN_POINT('Ctrl Pts',(56.0076859609607,-7.97208016193834,-37.1477844447593));
#23947=CARTESIAN_POINT('Ctrl Pts',(56.3858156688506,-8.1169486357207,-36.7289427228566));
#23948=CARTESIAN_POINT('Ctrl Pts',(56.7705126358147,-8.23551698557478,-36.3074625031452));
#23949=CARTESIAN_POINT('Ctrl Pts',(57.1943033398964,-8.36613450736868,-35.8431505526829));
#23950=CARTESIAN_POINT('Ctrl Pts',(57.6260640850358,-8.46483346777168,-35.3756366645352));
#23951=CARTESIAN_POINT('Ctrl Pts',(58.0637925846012,-8.53296150481107,-34.9083769250887));
#23952=CARTESIAN_POINT('Ctrl Pts',(58.0993721404169,-8.53849910471345,-34.8703970037525));
#23953=CARTESIAN_POINT('Ctrl Pts',(58.1349911067779,-8.54383472057116,-34.8324187822653));
#23954=CARTESIAN_POINT('Ctrl Pts',(58.1706483991881,-8.54896907247115,-34.7944441274998));
#23955=CARTESIAN_POINT('Ctrl Pts',(58.5551727492141,-8.60433736304228,-34.3849295947302));
#23956=CARTESIAN_POINT('Ctrl Pts',(58.944155818618,-8.63630043942602,-33.9758280479163));
#23957=CARTESIAN_POINT('Ctrl Pts',(59.3362796214209,-8.64327347910499,-33.5693510645206));
#23958=CARTESIAN_POINT('Ctrl Pts',(59.6583329109191,-8.64900047234121,-33.2355094342187));
#23959=CARTESIAN_POINT('Ctrl Pts',(59.9827515460476,-8.6381484172323,-32.9031110658833));
#23960=CARTESIAN_POINT('Ctrl Pts',(60.3086572343028,-8.60978376402087,-32.5735422953563));
#23961=CARTESIAN_POINT('Ctrl Pts',(60.6228690745861,-8.58243686519172,-32.255798808148));
#23962=CARTESIAN_POINT('Ctrl Pts',(60.938462675709,-8.53881140084064,-31.9406862056459));
#23963=CARTESIAN_POINT('Ctrl Pts',(61.254642507309,-8.47811729861641,-31.6294480076406));
#23964=CARTESIAN_POINT('Ctrl Pts',(61.5028961274628,-8.43046235958092,-31.3850743896462));
#23965=CARTESIAN_POINT('Ctrl Pts',(61.7515109191481,-8.37228568684251,-31.1430894138287));
#23966=CARTESIAN_POINT('Ctrl Pts',(62.0001008132074,-8.30322720641197,-30.9040914170777));
#23967=CARTESIAN_POINT('',(62.0088202634227,-8.3010477799695,-30.8955608315711));
#23968=CARTESIAN_POINT('Ctrl Pts',(62.0005099868911,-8.30357543269804,-30.9035738677768));
#23969=CARTESIAN_POINT('Ctrl Pts',(62.0033470639992,-8.30278347640663,-30.9008472871189));
#23970=CARTESIAN_POINT('Ctrl Pts',(62.0061841412741,-8.30199009465469,-30.8981210941654));
#23971=CARTESIAN_POINT('Ctrl Pts',(62.0090212182218,-8.30119528689782,-30.8953952897239));
#23972=CARTESIAN_POINT('',(63.3333333333333,-6.59966329107444,-31.7128621774316));
#23973=CARTESIAN_POINT('Ctrl Pts',(62.0085237301998,-8.30083011557419,-30.8958051086804));
#23974=CARTESIAN_POINT('Ctrl Pts',(62.0311590677664,-8.05644177174264,-30.9380272890384));
#23975=CARTESIAN_POINT('Ctrl Pts',(62.0981396788048,-7.82229842288598,-30.9982213762078));
#23976=CARTESIAN_POINT('Ctrl Pts',(62.315933348572,-7.37581872570051,-31.1536217805517));
#23977=CARTESIAN_POINT('Ctrl Pts',(62.4713648465707,-7.17154726294401,-31.249902943982));
#23978=CARTESIAN_POINT('Ctrl Pts',(62.8535438668198,-6.82510864454588,-31.4671224701204));
#23979=CARTESIAN_POINT('Ctrl Pts',(63.0820808101837,-6.68927586422443,-31.5880758676676));
#23980=CARTESIAN_POINT('Ctrl Pts',(63.3298258043247,-6.60090614371293,-31.7111212674739));
#23981=CARTESIAN_POINT('Ctrl Pts',(63.331579144709,-6.60028349041031,-31.7119917027094));
#23982=CARTESIAN_POINT('Ctrl Pts',(63.3333333333333,-6.59966329107444,-31.7128621774316));
#23983=CARTESIAN_POINT('',(54.0006369628663,-9.87019395503469E-7,-44.8274429326583));
#23984=CARTESIAN_POINT('Ctrl Pts',(63.3333333333333,-6.59966329107444,-31.7128621774316));
#23985=CARTESIAN_POINT('Ctrl Pts',(62.1773896945574,-7.00835108389839,-33.1107619749047));
#23986=CARTESIAN_POINT('Ctrl Pts',(59.8510477373174,-7.17140712600759,-36.1605129538655));
#23987=CARTESIAN_POINT('Ctrl Pts',(57.183782288428,-6.08047773499016,-40.0089544705698));
#23988=CARTESIAN_POINT('Ctrl Pts',(55.3668393528774,-4.31463467556344,-42.7323184706779));
#23989=CARTESIAN_POINT('Ctrl Pts',(54.4252091326635,-2.64874627344738,-44.1725365377487));
#23990=CARTESIAN_POINT('Ctrl Pts',(54.0472129322659,-1.09312894171435,-44.7556283321497));
#23991=CARTESIAN_POINT('Ctrl Pts',(54.0005126820376,-0.273223819838185,
-44.8276413098042));
#23992=CARTESIAN_POINT('Ctrl Pts',(54.0006369887046,5.63225172177384E-5,
-44.8274428914028));
#23993=CARTESIAN_POINT('',(63.3333333333333,6.59966329107444,-31.7128621774316));
#23994=CARTESIAN_POINT('Ctrl Pts',(54.0006369628663,-9.87019395576327E-7,
-44.8274429326583));
#23995=CARTESIAN_POINT('Ctrl Pts',(54.000759063025,0.273250808313191,-44.827247918389));
#23996=CARTESIAN_POINT('Ctrl Pts',(54.0481920300815,1.09290429704828,-44.7540646741929));
#23997=CARTESIAN_POINT('Ctrl Pts',(54.3607684393205,2.38775013614543,-44.2719711995386));
#23998=CARTESIAN_POINT('Ctrl Pts',(55.2216130985053,4.14017606552555,-42.9536995244691));
#23999=CARTESIAN_POINT('Ctrl Pts',(57.007705320374,6.00979472992292,-40.2625095891802));
#24000=CARTESIAN_POINT('Ctrl Pts',(59.8499534347117,7.17041001211291,-36.1623598714334));
#24001=CARTESIAN_POINT('Ctrl Pts',(62.177413277237,7.00834274616208,-33.1107334560203));
#24002=CARTESIAN_POINT('Ctrl Pts',(63.3333333333333,6.59966329107444,-31.7128621774316));
#24003=CARTESIAN_POINT('',(62.0088028665926,8.30103473250453,-30.8955848315571));
#24004=CARTESIAN_POINT('Ctrl Pts',(63.3333333333333,6.59966329107444,-31.7128621774316));
#24005=CARTESIAN_POINT('Ctrl Pts',(63.3315791446631,6.60028349042654,-31.7119917026866));
#24006=CARTESIAN_POINT('Ctrl Pts',(63.3298258160868,6.60090617043969,-31.7111212664723));
#24007=CARTESIAN_POINT('Ctrl Pts',(63.3280733522143,6.60153132813992,-31.7102508716682));
#24008=CARTESIAN_POINT('Ctrl Pts',(63.2635232041076,6.62455834899427,-31.6781908021871));
#24009=CARTESIAN_POINT('Ctrl Pts',(63.2001937780771,6.65092550213733,-31.6462071962042));
#24010=CARTESIAN_POINT('Ctrl Pts',(63.1383080680394,6.6804983322719,-31.6144426934177));
#24011=CARTESIAN_POINT('Ctrl Pts',(63.0761479782219,6.71020227808104,-31.58253735784));
#24012=CARTESIAN_POINT('Ctrl Pts',(63.015444088525,6.74314079497629,-31.5508526061538));
#24013=CARTESIAN_POINT('Ctrl Pts',(62.9564567516355,6.77921725541551,-31.5195350800571));
#24014=CARTESIAN_POINT('Ctrl Pts',(62.8977369868048,6.81513006966725,-31.4883596131781));
#24015=CARTESIAN_POINT('Ctrl Pts',(62.8407179621036,6.85415287127117,-31.4575476304171));
#24016=CARTESIAN_POINT('Ctrl Pts',(62.7856950660349,6.89622306178314,-31.4272524681983));
#24017=CARTESIAN_POINT('Ctrl Pts',(62.7691692946379,6.90885857173816,-31.4181535119268));
#24018=CARTESIAN_POINT('Ctrl Pts',(62.7528238671385,6.92176917986149,-31.4091012602555));
#24019=CARTESIAN_POINT('Ctrl Pts',(62.7366655328393,6.93495040659354,-31.4000991129422));
#24020=CARTESIAN_POINT('Ctrl Pts',(62.6833910901369,6.97840924927402,-31.3704188023133));
#24021=CARTESIAN_POINT('Ctrl Pts',(62.63226160359,7.02471404691096,-31.3413468098537));
#24022=CARTESIAN_POINT('Ctrl Pts',(62.5834883508633,7.07370394238452,-31.3130025833967));
#24023=CARTESIAN_POINT('Ctrl Pts',(62.5353508777631,7.12205523420339,-31.2850278357156));
#24024=CARTESIAN_POINT('Ctrl Pts',(62.4895084719016,7.17302268219252,-31.257761588209));
#24025=CARTESIAN_POINT('Ctrl Pts',(62.4462067271139,7.22647307749946,-31.2313344330245));
#24026=CARTESIAN_POINT('Ctrl Pts',(62.4102568378579,7.27084855939736,-31.2093941323071));
#24027=CARTESIAN_POINT('Ctrl Pts',(62.3760588170702,7.31693597573896,-31.1880323491785));
#24028=CARTESIAN_POINT('Ctrl Pts',(62.3437770329297,7.36466613151546,-31.1673352748822));
#24029=CARTESIAN_POINT('Ctrl Pts',(62.3208256261186,7.39860087990527,-31.1526202588253));
#24030=CARTESIAN_POINT('Ctrl Pts',(62.2988433325185,7.43336620520493,-31.1382414985304));
#24031=CARTESIAN_POINT('Ctrl Pts',(62.2778800856691,7.46892117258342,-31.1242222112547));
#24032=CARTESIAN_POINT('Ctrl Pts',(62.2423237652168,7.52922689825947,-31.1004437252946));
#24033=CARTESIAN_POINT('Ctrl Pts',(62.2098522421806,7.59153865793464,-31.077803087974));
#24034=CARTESIAN_POINT('Ctrl Pts',(62.180645578126,7.65563148244981,-31.0563991987818));
#24035=CARTESIAN_POINT('Ctrl Pts',(62.1580094653665,7.7053055020534,-31.0398104898372));
#24036=CARTESIAN_POINT('Ctrl Pts',(62.1373353088525,7.75604981429739,-31.0239650024763));
#24037=CARTESIAN_POINT('Ctrl Pts',(62.118725318096,7.80776250967515,-31.0089197705683));
#24038=CARTESIAN_POINT('Ctrl Pts',(62.0952037529992,7.87312329069713,-30.9899037803751));
#24039=CARTESIAN_POINT('Ctrl Pts',(62.0749785877622,7.94003185523155,-30.9721652566799));
#24040=CARTESIAN_POINT('Ctrl Pts',(62.0582301482953,8.00824501492773,-30.9557896333494));
#24041=CARTESIAN_POINT('Ctrl Pts',(62.0467738079755,8.0549044767425,-30.9445883083428));
#24042=CARTESIAN_POINT('Ctrl Pts',(62.0369450076869,8.10217425231307,-30.9340252251599));
#24043=CARTESIAN_POINT('Ctrl Pts',(62.0288121054035,8.14997249472371,-30.924136146721));
#24044=CARTESIAN_POINT('Ctrl Pts',(62.020307426509,8.19995572202247,-30.9137950121843));
#24045=CARTESIAN_POINT('Ctrl Pts',(62.013678947783,8.25038775318331,-30.9042177588782));
#24046=CARTESIAN_POINT('Ctrl Pts',(62.0089847266465,8.30116803958258,-30.8954413183826));
#24047=CARTESIAN_POINT('Ctrl Pts',(62.0089847242203,8.30116804026198,-30.8954413207137));
#24048=CARTESIAN_POINT('Ctrl Pts',(62.0061473048757,8.30196259736025,-30.8981675557624));
#24049=CARTESIAN_POINT('Ctrl Pts',(62.0033098833227,8.30275572690749,-30.900894181743));
#24050=CARTESIAN_POINT('Ctrl Pts',(62.0004724600677,8.30354742945956,-30.9036211978314));
#24051=CARTESIAN_POINT('Origin',(64.,-8.48528137423857,13.));
#24052=CARTESIAN_POINT('',(63.3333333333333,-6.59966329107444,31.7128621774316));
#24053=CARTESIAN_POINT('',(63.3333333333333,-6.59966329107444,13.));
#24054=CARTESIAN_POINT('',(62.,-8.48528137423857,-30.854497241083));
#24055=CARTESIAN_POINT('Ctrl Pts',(62.0085237301807,-8.30083011578128,-30.8958051086446));
#24056=CARTESIAN_POINT('Ctrl Pts',(62.0029032474376,-8.36151312820127,-30.885321101655));
#24057=CARTESIAN_POINT('Ctrl Pts',(62.,-8.42346268655744,-30.8714979705087));
#24058=CARTESIAN_POINT('Ctrl Pts',(62.,-8.48528137423856,-30.854497241083));
#24059=CARTESIAN_POINT('',(62.,-8.48528137423857,30.854497241083));
#24060=CARTESIAN_POINT('',(62.,-8.48528137423857,13.));
#24061=CARTESIAN_POINT('',(62.008849633308,-8.30100100727199,30.895526211557));
#24062=CARTESIAN_POINT('Ctrl Pts',(62.,-8.48528137423857,30.854497241083));
#24063=CARTESIAN_POINT('Ctrl Pts',(62.,-8.42347251099396,30.8714952686948));
#24064=CARTESIAN_POINT('Ctrl Pts',(62.0029020528202,-8.36152602610337,30.8853188733362));
#24065=CARTESIAN_POINT('Ctrl Pts',(62.0085237302078,-8.30083011548887,30.8958051086952));
#24066=CARTESIAN_POINT('Ctrl Pts',(63.3333333333333,-6.59966329107444,31.7128621774316));
#24067=CARTESIAN_POINT('Ctrl Pts',(63.3315791446588,-6.60028349042807,31.7119917026845));
#24068=CARTESIAN_POINT('Ctrl Pts',(63.3298258164317,-6.60090617028985,31.7111212659654));
#24069=CARTESIAN_POINT('Ctrl Pts',(63.3280733532319,-6.60153132770387,31.7102508701461));
#24070=CARTESIAN_POINT('Ctrl Pts',(63.2635050836892,-6.62456481132822,31.6781817505937));
#24071=CARTESIAN_POINT('Ctrl Pts',(63.2001586660833,-6.65094012635296,31.6461884495608));
#24072=CARTESIAN_POINT('Ctrl Pts',(63.1382571476502,-6.68052308701512,31.6144138631241));
#24073=CARTESIAN_POINT('Ctrl Pts',(63.0760620233079,-6.71024636300848,31.5824885662271));
#24074=CARTESIAN_POINT('Ctrl Pts',(63.0153251922965,-6.74320819450885,31.5507835985174));
#24075=CARTESIAN_POINT('Ctrl Pts',(62.956307457809,-6.77931199071329,31.5194460012486));
#24076=CARTESIAN_POINT('Ctrl Pts',(62.8976433010526,-6.81519948755522,31.4882961488439));
#24077=CARTESIAN_POINT('Ctrl Pts',(62.8406774425965,-6.85419187098811,31.4575088655831));
#24078=CARTESIAN_POINT('Ctrl Pts',(62.7857045379272,-6.89622665807325,31.4272371911452));
#24079=CARTESIAN_POINT('Ctrl Pts',(62.7691793523232,-6.90886256775612,31.4181373438361));
#24080=CARTESIAN_POINT('Ctrl Pts',(62.7528345382147,-6.92177360354981,31.4090841726496));
#24081=CARTESIAN_POINT('Ctrl Pts',(62.7366768459354,-6.93495528086646,31.4000810795403));
#24082=CARTESIAN_POINT('Ctrl Pts',(62.6833852217834,-6.97843135288908,31.3703868976057));
#24083=CARTESIAN_POINT('Ctrl Pts',(62.6322404130614,-7.02475569639747,31.3413011968834));
#24084=CARTESIAN_POINT('Ctrl Pts',(62.5834539692209,-7.07376700776111,31.3129436174977));
#24085=CARTESIAN_POINT('Ctrl Pts',(62.5353085615151,-7.12213432831251,31.2849586463951));
#24086=CARTESIAN_POINT('Ctrl Pts',(62.4894598137834,-7.17311907144123,31.2576823710423));
#24087=CARTESIAN_POINT('Ctrl Pts',(62.4461535426247,-7.22658757348273,31.231245525692));
#24088=CARTESIAN_POINT('Ctrl Pts',(62.4102361210531,-7.27093336168479,31.2093192943619));
#24089=CARTESIAN_POINT('Ctrl Pts',(62.3760682926572,-7.31698819323151,31.1879706493171));
#24090=CARTESIAN_POINT('Ctrl Pts',(62.3438140501227,-7.36468280083248,31.1672856002691));
#24091=CARTESIAN_POINT('Ctrl Pts',(62.3208649852281,-7.39861776748955,31.1525680779945));
#24092=CARTESIAN_POINT('Ctrl Pts',(62.2988851467792,-7.43338305818485,31.1381867524407));
#24093=CARTESIAN_POINT('Ctrl Pts',(62.2779244539186,-7.46893767670066,31.124164845081));
#24094=CARTESIAN_POINT('Ctrl Pts',(62.2423689479923,-7.52924877699471,31.1003795621449));
#24095=CARTESIAN_POINT('Ctrl Pts',(62.2098991175825,-7.5915653981267,31.0777322138085));
#24096=CARTESIAN_POINT('Ctrl Pts',(62.1806949586429,-7.65566232615891,31.0563217546863));
#24097=CARTESIAN_POINT('Ctrl Pts',(62.1580659155852,-7.70532827090699,31.0397317134404));
#24098=CARTESIAN_POINT('Ctrl Pts',(62.1373984273643,-7.75606357093779,31.0238846422908));
#24099=CARTESIAN_POINT('Ctrl Pts',(62.1187945868658,-7.80776633320906,31.0088375691922));
#24100=CARTESIAN_POINT('Ctrl Pts',(62.0952718368554,-7.87313945613236,30.9898120062223));
#24101=CARTESIAN_POINT('Ctrl Pts',(62.075047167823,-7.94006006372112,30.9720644712138));
#24102=CARTESIAN_POINT('Ctrl Pts',(62.0583009018868,-8.00828491614149,30.9556804706479));
#24103=CARTESIAN_POINT('Ctrl Pts',(62.0468531893068,-8.05492328342251,30.944480401922));
#24104=CARTESIAN_POINT('Ctrl Pts',(62.0370317732946,-8.10217104304868,30.9339180770259));
#24105=CARTESIAN_POINT('Ctrl Pts',(62.0289048874703,-8.1499465245071,30.9240292222972));
#24106=CARTESIAN_POINT('Ctrl Pts',(62.0204033521119,-8.19992445623345,30.9136844912469));
#24107=CARTESIAN_POINT('Ctrl Pts',(62.0137778853462,-8.25035081906717,30.9041036111461));
#24108=CARTESIAN_POINT('Ctrl Pts',(62.0090864889818,-8.30112520359226,30.8953235179838));
#24109=CARTESIAN_POINT('Origin',(64.,8.48528137423857,13.));
#24110=CARTESIAN_POINT('',(62.,8.48528137423857,30.854497241083));
#24111=CARTESIAN_POINT('',(62.,8.48528137423857,-30.854497241083));
#24112=CARTESIAN_POINT('',(62.,8.48528137423857,13.));
#24113=CARTESIAN_POINT('Ctrl Pts',(62.,8.48528137423857,-30.854497241083));
#24114=CARTESIAN_POINT('Ctrl Pts',(62.,8.42347251099396,-30.8714952686948));
#24115=CARTESIAN_POINT('Ctrl Pts',(62.0029020528202,8.36152602610337,-30.8853188733362));
#24116=CARTESIAN_POINT('Ctrl Pts',(62.0085237302078,8.30083011548887,-30.8958051086952));
#24117=CARTESIAN_POINT('',(63.3333333333334,6.59966329107444,31.7128621774316));
#24118=CARTESIAN_POINT('',(63.3333333333333,6.59966329107444,13.));
#24119=CARTESIAN_POINT('',(62.0088203985241,8.30104700095525,30.8955604966231));
#24120=CARTESIAN_POINT('Ctrl Pts',(63.3333333333334,6.59966329107444,31.7128621774316));
#24121=CARTESIAN_POINT('Ctrl Pts',(63.3315791447087,6.60028349041044,31.7119917027092));
#24122=CARTESIAN_POINT('Ctrl Pts',(63.3298258043253,6.60090614371271,31.7111212674742));
#24123=CARTESIAN_POINT('Ctrl Pts',(63.0820808102159,6.68927586421289,31.5880758676829));
#24124=CARTESIAN_POINT('Ctrl Pts',(62.8535438668757,6.82510864451255,31.46712247015));
#24125=CARTESIAN_POINT('Ctrl Pts',(62.4713648466326,7.17154726287157,31.2499029440192));
#24126=CARTESIAN_POINT('Ctrl Pts',(62.3159333486232,7.37581872562244,31.1536217805848));
#24127=CARTESIAN_POINT('Ctrl Pts',(62.0981396750928,7.82229843047092,30.9982213735624));
#24128=CARTESIAN_POINT('Ctrl Pts',(62.0311590674915,8.05644177565425,30.9380272884007));
#24129=CARTESIAN_POINT('Ctrl Pts',(62.0085237302653,8.30083011486769,30.8958051088025));
#24130=CARTESIAN_POINT('Ctrl Pts',(62.0085237301807,8.30083011578128,30.8958051086446));
#24131=CARTESIAN_POINT('Ctrl Pts',(62.0029032474376,8.36151312820127,30.885321101655));
#24132=CARTESIAN_POINT('Ctrl Pts',(62.,8.42346268655744,30.8714979705087));
#24133=CARTESIAN_POINT('Ctrl Pts',(62.,8.48528137423857,30.854497241083));
#24134=CARTESIAN_POINT('Ctrl Pts',(63.3333333333334,6.59966329107444,31.7128621774316));
#24135=CARTESIAN_POINT('Ctrl Pts',(62.1773896945574,7.00835108389839,33.1107619749047));
#24136=CARTESIAN_POINT('Ctrl Pts',(59.8510643212503,7.17136627556463,36.1604788683916));
#24137=CARTESIAN_POINT('Ctrl Pts',(57.1837550511065,6.08049991760512,40.0089963598732));
#24138=CARTESIAN_POINT('Ctrl Pts',(55.3668248198271,4.31461669518687,42.7323293863949));
#24139=CARTESIAN_POINT('Ctrl Pts',(54.4251147577635,2.64876740625127,44.1726835846802));
#24140=CARTESIAN_POINT('Ctrl Pts',(53.9842189222391,0.833747439766708,44.852770613662));
#24141=CARTESIAN_POINT('Ctrl Pts',(53.985357986249,-0.833764372921021,44.8510072059771));
#24142=CARTESIAN_POINT('Ctrl Pts',(54.3610359933426,-2.38837584180055,44.2714261991957));
#24143=CARTESIAN_POINT('Ctrl Pts',(55.0050244523723,-3.70114923515179,43.2855805513825));
#24144=CARTESIAN_POINT('Ctrl Pts',(55.8180315346338,-4.7647811160322,42.0547184493501));
#24145=CARTESIAN_POINT('Ctrl Pts',(57.3603596238608,-6.15480540711906,39.7540563319785));
#24146=CARTESIAN_POINT('Ctrl Pts',(59.8534489927889,-7.16888802237617,36.1571505333425));
#24147=CARTESIAN_POINT('Ctrl Pts',(62.177413277237,-7.00834274616208,33.1107334560203));
#24148=CARTESIAN_POINT('Ctrl Pts',(63.3333333333333,-6.59966329107444,31.7128621774316));
#24149=CARTESIAN_POINT('Ctrl Pts',(63.1962492273341,6.6481298415469,31.5488996087769));
#24150=CARTESIAN_POINT('Ctrl Pts',(62.0093421297043,7.04072991080625,32.9391773083993));
#24151=CARTESIAN_POINT('Ctrl Pts',(59.6306254735857,7.14629729109621,35.9670702941392));
#24152=CARTESIAN_POINT('Ctrl Pts',(56.9648615533032,5.94454544765156,39.7623544055489));
#24153=CARTESIAN_POINT('Ctrl Pts',(55.2199565629048,4.1186832182827,42.4090274642781));
#24154=CARTESIAN_POINT('Ctrl Pts',(54.3627119956756,2.46990066692426,43.7769112833253));
#24155=CARTESIAN_POINT('Ctrl Pts',(53.9868660380235,0.765082134508059,44.4022644152194));
#24156=CARTESIAN_POINT('Ctrl Pts',(53.9874577061127,-0.764888305104543,
44.40097010027));
#24157=CARTESIAN_POINT('Ctrl Pts',(54.308342330058,-2.22529296405365,43.86757204928));
#24158=CARTESIAN_POINT('Ctrl Pts',(54.8892188306448,-3.5093071402967,42.9356756235718));
#24159=CARTESIAN_POINT('Ctrl Pts',(55.6523321195903,-4.58361797221118,41.7510674504422));
#24160=CARTESIAN_POINT('Ctrl Pts',(57.1409463863557,-6.02588925105485,39.5112017421951));
#24161=CARTESIAN_POINT('Ctrl Pts',(59.6331015208575,-7.14454194899524,35.9635238647728));
#24162=CARTESIAN_POINT('Ctrl Pts',(62.0093663440767,-7.04072190127939,32.9391489450152));
#24163=CARTESIAN_POINT('Ctrl Pts',(63.1962492273341,-6.64812984154691,31.5488996087769));
#24164=CARTESIAN_POINT('Ctrl Pts',(62.9463311105499,6.81360008562125,31.2209941996293));
#24165=CARTESIAN_POINT('Ctrl Pts',(61.6902590726639,7.19193133539315,32.5959957954705));
#24166=CARTESIAN_POINT('Ctrl Pts',(59.1806910892167,7.22376058361478,35.5805693674503));
#24167=CARTESIAN_POINT('Ctrl Pts',(56.4330414247942,5.8407858655779,39.2697861596156));
#24168=CARTESIAN_POINT('Ctrl Pts',(54.7292159564143,3.88448268514588,41.7632982027126));
#24169=CARTESIAN_POINT('Ctrl Pts',(53.9652037659389,2.22577079086734,42.9859075220035));
#24170=CARTESIAN_POINT('Ctrl Pts',(53.6754715503903,0.666318585301244,43.5014342636392));
#24171=CARTESIAN_POINT('Ctrl Pts',(53.6751795362821,-0.665698958814348,
43.501067912247));
#24172=CARTESIAN_POINT('Ctrl Pts',(53.9236778818116,-2.0018479285686,43.0602414260277));
#24173=CARTESIAN_POINT('Ctrl Pts',(54.4317973968295,-3.26780308655164,42.2363800092985));
#24174=CARTESIAN_POINT('Ctrl Pts',(55.1499982747057,-4.38195964414384,41.1445144943703));
#24175=CARTESIAN_POINT('Ctrl Pts',(56.6140690268316,-5.93366160544652,39.0263796051091));
#24176=CARTESIAN_POINT('Ctrl Pts',(59.1836503932084,-7.22318373229117,35.576683205603));
#24177=CARTESIAN_POINT('Ctrl Pts',(61.6902846980866,-7.19192361696785,32.5959677437378));
#24178=CARTESIAN_POINT('Ctrl Pts',(62.9463311105498,-6.81360008562125,31.2209941996293));
#24179=CARTESIAN_POINT('Ctrl Pts',(62.7061595886978,7.20521258113835,30.8184466564059));
#24180=CARTESIAN_POINT('Ctrl Pts',(61.3525918084502,7.61031511383114,32.1841418341021));
#24181=CARTESIAN_POINT('Ctrl Pts',(58.639719444944,7.65453953624728,35.1410478713317));
#24182=CARTESIAN_POINT('Ctrl Pts',(55.6374343951349,6.19012486821752,38.7683214990875));
#24183=CARTESIAN_POINT('Ctrl Pts',(53.7520469534746,4.10519226863261,41.1835161043104));
#24184=CARTESIAN_POINT('Ctrl Pts',(52.8964738416428,2.33969535740793,42.3385222833608));
#24185=CARTESIAN_POINT('Ctrl Pts',(52.5689543596521,0.696894842639347,42.8062051339743));
#24186=CARTESIAN_POINT('Ctrl Pts',(52.5686719868954,-0.69616267180925,42.8062135338103));
#24187=CARTESIAN_POINT('Ctrl Pts',(52.8494705009145,-2.10371014619857,42.405795394335));
#24188=CARTESIAN_POINT('Ctrl Pts',(53.4191785279361,-3.44852229436623,41.6315854149983));
#24189=CARTESIAN_POINT('Ctrl Pts',(54.2179795314303,-4.6354735302374,40.5847140055125));
#24190=CARTESIAN_POINT('Ctrl Pts',(55.8351784344025,-6.28842573724461,38.5292245334429));
#24191=CARTESIAN_POINT('Ctrl Pts',(58.6430771173405,-7.65402260661205,35.1370333846699));
#24192=CARTESIAN_POINT('Ctrl Pts',(61.3526194229065,-7.61030684923857,32.1841139722319));
#24193=CARTESIAN_POINT('Ctrl Pts',(62.7061595886978,-7.20521258113835,30.8184466564059));
#24194=CARTESIAN_POINT('Ctrl Pts',(62.5904039193512,7.6583127936691,30.5250624561551));
#24195=CARTESIAN_POINT('Ctrl Pts',(61.1584933846713,8.11585881641404,31.8989848492516));
#24196=CARTESIAN_POINT('Ctrl Pts',(58.2792017179309,8.24146500383239,34.8758878324567));
#24197=CARTESIAN_POINT('Ctrl Pts',(55.0264864356743,6.82106261533207,38.5566816547643));
#24198=CARTESIAN_POINT('Ctrl Pts',(52.8924820285019,4.67292890435344,41.0602180277437));
#24199=CARTESIAN_POINT('Ctrl Pts',(51.8520940544338,2.76163585714774,42.3048969763665));
#24200=CARTESIAN_POINT('Ctrl Pts',(51.4059275777634,0.845595187901781,42.8430538858222));
#24201=CARTESIAN_POINT('Ctrl Pts',(51.4064422995083,-0.845159328481016,
42.8424354934688));
#24202=CARTESIAN_POINT('Ctrl Pts',(51.7875642574907,-2.48653462782744,42.3826354495856));
#24203=CARTESIAN_POINT('Ctrl Pts',(52.4904256291742,-3.96523549111311,41.5411529134917));
#24204=CARTESIAN_POINT('Ctrl Pts',(53.4212386216903,-5.21989656328882,40.4387210123535));
#24205=CARTESIAN_POINT('Ctrl Pts',(55.2412605277983,-6.91695086253193,38.3135879661086));
#24206=CARTESIAN_POINT('Ctrl Pts',(58.2825427953835,-8.23988638622876,34.872150343801));
#24207=CARTESIAN_POINT('Ctrl Pts',(61.1585225974167,-8.11584948190943,31.898956819536));
#24208=CARTESIAN_POINT('Ctrl Pts',(62.5904039193511,-7.6583127936691,30.5250624561552));
#24209=CARTESIAN_POINT('Ctrl Pts',(62.5777174765496,7.9634392868377,30.3968807187894));
#24210=CARTESIAN_POINT('Ctrl Pts',(61.1076965731432,8.46164972651616,31.7860405531774));
#24211=CARTESIAN_POINT('Ctrl Pts',(58.1492105273372,8.65876024618515,34.8022481083434));
#24212=CARTESIAN_POINT('Ctrl Pts',(54.7703733975909,7.30102209714431,38.5745952960703));
#24213=CARTESIAN_POINT('Ctrl Pts',(52.4937350175267,5.13051425931518,41.2071640355381));
#24214=CARTESIAN_POINT('Ctrl Pts',(51.3344612102292,3.11541106986722,42.5714726656167));
#24215=CARTESIAN_POINT('Ctrl Pts',(50.8048762661169,0.972902268736063,43.1985090979019));
#24216=CARTESIAN_POINT('Ctrl Pts',(50.8060383404805,-0.972769282655253,
43.1971473210877));
#24217=CARTESIAN_POINT('Ctrl Pts',(51.2576003506582,-2.80797998191018,42.6623597404875));
#24218=CARTESIAN_POINT('Ctrl Pts',(52.0476061174834,-4.38726349542764,41.7321453947841));
#24219=CARTESIAN_POINT('Ctrl Pts',(53.0587432961293,-5.68374075190955,40.5526413291701));
#24220=CARTESIAN_POINT('Ctrl Pts',(54.9939048068932,-7.39328817802591,38.3250004905781));
#24221=CARTESIAN_POINT('Ctrl Pts',(58.1523706727149,-8.65618956969658,34.7988022375372));
#24222=CARTESIAN_POINT('Ctrl Pts',(61.1077265633873,-8.46163956240716,31.7860122125991));
#24223=CARTESIAN_POINT('Ctrl Pts',(62.5777174765495,-7.9634392868377,30.3968807187894));
#24224=CARTESIAN_POINT('Ctrl Pts',(62.5857864376269,8.11974451941452,30.3467059609741));
#24225=CARTESIAN_POINT('Ctrl Pts',(61.0995731877722,8.63911281829803,31.7462345485699));
#24226=CARTESIAN_POINT('Ctrl Pts',(58.1085834220916,8.87357929861398,34.7889401279806));
#24227=CARTESIAN_POINT('Ctrl Pts',(54.6791857890496,7.54851825740161,38.6195934717837));
#24228=CARTESIAN_POINT('Ctrl Pts',(52.3431326345475,5.36613894866642,41.3291233333569));
#24229=CARTESIAN_POINT('Ctrl Pts',(51.1323625547514,3.29730168453684,42.7619221061187));
#24230=CARTESIAN_POINT('Ctrl Pts',(50.5654964805058,1.03828559051394,43.4384291646527));
#24231=CARTESIAN_POINT('Ctrl Pts',(50.5669609913757,-1.03830665890786,43.4366729518529));
#24232=CARTESIAN_POINT('Ctrl Pts',(51.0499755719245,-2.97319690488059,42.8601506219393));
#24233=CARTESIAN_POINT('Ctrl Pts',(51.8779607335342,-4.60442848107814,41.8794658901552));
#24234=CARTESIAN_POINT('Ctrl Pts',(52.9232555535846,-5.92265909195242,40.6549664913959));
#24235=CARTESIAN_POINT('Ctrl Pts',(54.9062488111622,-7.63883014775581,38.3658488848707));
#24236=CARTESIAN_POINT('Ctrl Pts',(58.1116494283555,-8.87050844544732,34.7856031628019));
#24237=CARTESIAN_POINT('Ctrl Pts',(61.0996035083602,-8.63910222254255,31.7462059964563));
#24238=CARTESIAN_POINT('Ctrl Pts',(62.5857864376269,-8.11974451941452,30.3467059609741));
#24239=CARTESIAN_POINT('',(62.000165884661,-8.3032680262804,30.9039893606587));
#24240=CARTESIAN_POINT('',(62.0001575703546,8.3032754367448,30.9040190526451));
#24241=CARTESIAN_POINT('Ctrl Pts',(62.0000893809181,-8.30322423863785,30.904080390366));
#24242=CARTESIAN_POINT('Ctrl Pts',(61.6561655749137,-8.39875971217444,31.2347093086726));
#24243=CARTESIAN_POINT('Ctrl Pts',(61.312246656489,-8.47352712664702,31.570965086887));
#24244=CARTESIAN_POINT('Ctrl Pts',(60.9692904429481,-8.52842461676202,31.9113599823671));
#24245=CARTESIAN_POINT('Ctrl Pts',(60.6092687475215,-8.58605380289575,32.2686929086903));
#24246=CARTESIAN_POINT('Ctrl Pts',(60.2503082421953,-8.62178639813802,32.6305870777806));
#24247=CARTESIAN_POINT('Ctrl Pts',(59.8935507198074,-8.63669078438552,32.9952825246954));
#24248=CARTESIAN_POINT('Ctrl Pts',(59.5460504659188,-8.6512084264254,33.3505147270794));
#24249=CARTESIAN_POINT('Ctrl Pts',(59.200640836074,-8.64596508009651,33.7084043749006));
#24250=CARTESIAN_POINT('Ctrl Pts',(58.8584017653847,-8.62197236638857,34.0672926119468));
#24251=CARTESIAN_POINT('Ctrl Pts',(58.6281835464303,-8.6058328887813,34.3087104330332));
#24252=CARTESIAN_POINT('Ctrl Pts',(58.3992449606898,-8.5811865819245,34.5507455964031));
#24253=CARTESIAN_POINT('Ctrl Pts',(58.1718343339284,-8.5483883566638,34.7929625798458));
#24254=CARTESIAN_POINT('Ctrl Pts',(57.7947286563834,-8.49400041035123,35.1946210289467));
#24255=CARTESIAN_POINT('Ctrl Pts',(57.421826114243,-8.41719678346568,35.5967774882034));
#24256=CARTESIAN_POINT('Ctrl Pts',(57.0544150878352,-8.31710533598519,35.9971993560921));
#24257=CARTESIAN_POINT('Ctrl Pts',(56.7092101840014,-8.22306336114325,36.3734199441049));
#24258=CARTESIAN_POINT('Ctrl Pts',(56.368852907092,-8.10846458855582,36.7481092284094));
#24259=CARTESIAN_POINT('Ctrl Pts',(56.0343874284652,-7.97256756446671,37.1194477581821));
#24260=CARTESIAN_POINT('Ctrl Pts',(55.7387207793211,-7.85243493401995,37.4477100925992));
#24261=CARTESIAN_POINT('Ctrl Pts',(55.4476581679515,-7.71565946307753,37.7733539993108));
#24262=CARTESIAN_POINT('Ctrl Pts',(55.1619029604268,-7.56170256232362,38.0951486520963));
#24263=CARTESIAN_POINT('Ctrl Pts',(55.0596996615354,-7.50663828797344,38.2102418305029));
#24264=CARTESIAN_POINT('Ctrl Pts',(54.9581751145601,-7.44937583169452,38.3248428739989));
#24265=CARTESIAN_POINT('Ctrl Pts',(54.857360866142,-7.38988930267797,38.4388964431299));
#24266=CARTESIAN_POINT('Ctrl Pts',(54.6095274878066,-7.24365255853758,38.7192762683279));
#24267=CARTESIAN_POINT('Ctrl Pts',(54.3664530066397,-7.08381787166391,38.9959034963516));
#24268=CARTESIAN_POINT('Ctrl Pts',(54.1286075746492,-6.9100316967836,39.2679453077468));
#24269=CARTESIAN_POINT('Ctrl Pts',(53.8559340081726,-6.71079769967733,39.579822690983));
#24270=CARTESIAN_POINT('Ctrl Pts',(53.5901332063915,-6.4932284863201,39.8856731212024));
#24271=CARTESIAN_POINT('Ctrl Pts',(53.3336133764994,-6.25552348746623,40.1823161614254));
#24272=CARTESIAN_POINT('Ctrl Pts',(53.2023314977896,-6.13387067473281,40.3341323217708));
#24273=CARTESIAN_POINT('Ctrl Pts',(53.073480450123,-6.00694321737372,40.4835370465735));
#24274=CARTESIAN_POINT('Ctrl Pts',(52.9473834727163,-5.87449429652602,40.6301042204462));
#24275=CARTESIAN_POINT('Ctrl Pts',(52.8117095535923,-5.73198601008858,40.787803027374));
#24276=CARTESIAN_POINT('Ctrl Pts',(52.6792238533422,-5.58308587547121,40.9422169831774));
#24277=CARTESIAN_POINT('Ctrl Pts',(52.5504935599745,-5.42758583527421,41.0926023952026));
#24278=CARTESIAN_POINT('Ctrl Pts',(52.3454270557672,-5.17987530177754,41.3321653599177));
#24279=CARTESIAN_POINT('Ctrl Pts',(52.1499225997406,-4.91535186897423,41.561480678128));
#24280=CARTESIAN_POINT('Ctrl Pts',(51.9663979586597,-4.63330475841997,41.7773970455567));
#24281=CARTESIAN_POINT('Ctrl Pts',(51.9489051159833,-4.60642114375545,41.7979773394314));
#24282=CARTESIAN_POINT('Ctrl Pts',(51.9315210899143,-4.57937834572491,41.8184359269166));
#24283=CARTESIAN_POINT('Ctrl Pts',(51.9142479594617,-4.55217576216835,41.8387700961554));
#24284=CARTESIAN_POINT('Ctrl Pts',(51.7536961254005,-4.29933076147783,42.0277739466369));
#24285=CARTESIAN_POINT('Ctrl Pts',(51.6027273490625,-4.03268011577195,42.2060260038393));
#24286=CARTESIAN_POINT('Ctrl Pts',(51.464240637923,-3.75251435206581,42.36988034755));
#24287=CARTESIAN_POINT('Ctrl Pts',(51.3334041833375,-3.4878254521854,42.5246830807737));
#24288=CARTESIAN_POINT('Ctrl Pts',(51.2137091021908,-3.21107414891051,42.6666345143635));
#24289=CARTESIAN_POINT('Ctrl Pts',(51.1075727371426,-2.92250941342542,42.7926932040937));
#24290=CARTESIAN_POINT('Ctrl Pts',(51.0958316745257,-2.89058768116312,42.806638122679));
#24291=CARTESIAN_POINT('Ctrl Pts',(51.0842565032326,-2.85852138158929,42.8203885943635));
#24292=CARTESIAN_POINT('Ctrl Pts',(51.0728507020669,-2.82631478942691,42.8339402661012));
#24293=CARTESIAN_POINT('Ctrl Pts',(50.9905591164766,-2.59394781257042,42.9317140689659));
#24294=CARTESIAN_POINT('Ctrl Pts',(50.9171137635618,-2.35422681405925,43.019113509796));
#24295=CARTESIAN_POINT('Ctrl Pts',(50.8538042492007,-2.10863256818959,43.0945234256458));
#24296=CARTESIAN_POINT('Ctrl Pts',(50.794402771643,-1.87819862423098,43.1652783582842));
#24297=CARTESIAN_POINT('Ctrl Pts',(50.7439241014323,-1.6425934332917,43.2254786846976));
#24298=CARTESIAN_POINT('Ctrl Pts',(50.7034615123714,-1.40302481611627,43.2737571692822));
#24299=CARTESIAN_POINT('Ctrl Pts',(50.691004801656,-1.32927182526984,43.2886200618999));
#24300=CARTESIAN_POINT('Ctrl Pts',(50.6794976055421,-1.25514312052498,43.3023527755394));
#24301=CARTESIAN_POINT('Ctrl Pts',(50.6689724743387,-1.18067377945559,43.3149146392693));
#24302=CARTESIAN_POINT('Ctrl Pts',(50.661175987002,-1.12551064054602,43.3242198355278));
#24303=CARTESIAN_POINT('Ctrl Pts',(50.6539207978311,-1.07017769902012,43.3328796750757));
#24304=CARTESIAN_POINT('Ctrl Pts',(50.6472193363222,-1.01468965833302,43.3408785990006));
#24305=CARTESIAN_POINT('Ctrl Pts',(50.616356722979,-0.759147498968588,43.3777164881572));
#24306=CARTESIAN_POINT('Ctrl Pts',(50.5972357485005,-0.500317544405125,
43.4005398504856));
#24307=CARTESIAN_POINT('Ctrl Pts',(50.5898714711672,-0.240738864968742,
43.4093313537544));
#24308=CARTESIAN_POINT('Ctrl Pts',(50.5875961987457,-0.160539249469542,
43.4120475829275));
#24309=CARTESIAN_POINT('Ctrl Pts',(50.586443408801,-0.0802680232746275,
43.413424106223));
#24310=CARTESIAN_POINT('Ctrl Pts',(50.5864141549312,2.20702370434811E-7,
43.413459684969));
#24311=CARTESIAN_POINT('Ctrl Pts',(50.5863344035338,0.218826128786446,43.4135566791352));
#24312=CARTESIAN_POINT('Ctrl Pts',(50.5946901354538,0.437687451886798,43.4036025250393));
#24313=CARTESIAN_POINT('Ctrl Pts',(50.6114484592242,0.65505550810239,43.3836221739438));
#24314=CARTESIAN_POINT('Ctrl Pts',(50.6207357926489,0.775519203732342,43.3725492178948));
#24315=CARTESIAN_POINT('Ctrl Pts',(50.6326040296411,0.895525157135156,43.3583966672893));
#24316=CARTESIAN_POINT('Ctrl Pts',(50.6470500171268,1.0148189366432,43.3411658012909));
#24317=CARTESIAN_POINT('Ctrl Pts',(50.6472729914877,1.01666024062296,43.3408998422252));
#24318=CARTESIAN_POINT('Ctrl Pts',(50.6474965800171,1.01850137500363,43.3406331497258));
#24319=CARTESIAN_POINT('Ctrl Pts',(50.647720782167,1.02034233925431,43.3403657244623));
#24320=CARTESIAN_POINT('Ctrl Pts',(50.6735956285347,1.23280536498562,43.3095025609724));
#24321=CARTESIAN_POINT('Ctrl Pts',(50.7075375601688,1.44282541763031,43.2689898459162));
#24322=CARTESIAN_POINT('Ctrl Pts',(50.7488174201003,1.6495499391546,43.2197515368914));
#24323=CARTESIAN_POINT('Ctrl Pts',(50.7926945580034,1.86928131309695,43.1674152140748));
#24324=CARTESIAN_POINT('Ctrl Pts',(50.8448629741679,2.08528923107664,43.1052195558173));
#24325=CARTESIAN_POINT('Ctrl Pts',(50.9044498982716,2.29649084950969,43.0342719592216));
#24326=CARTESIAN_POINT('Ctrl Pts',(50.9301517198461,2.38758912979296,43.0036699018697));
#24327=CARTESIAN_POINT('Ctrl Pts',(50.9572336936552,2.4777925102904,42.9714396437231));
#24328=CARTESIAN_POINT('Ctrl Pts',(50.985625379792,2.56701126801593,42.9376706686577));
#24329=CARTESIAN_POINT('Ctrl Pts',(51.0239835929914,2.6875490942565,42.8920475401528));
#24330=CARTESIAN_POINT('Ctrl Pts',(51.0647374564426,2.80638398422016,42.8436050676676));
#24331=CARTESIAN_POINT('Ctrl Pts',(51.1076949778189,2.92327958149374,42.7925812475125));
#24332=CARTESIAN_POINT('Ctrl Pts',(51.1859073117987,3.13611023842693,42.6996826831855));
#24333=CARTESIAN_POINT('Ctrl Pts',(51.2714261489779,3.34250990315628,42.5982253582903));
#24334=CARTESIAN_POINT('Ctrl Pts',(51.3633720424189,3.54236397232683,42.4893210803475));
#24335=CARTESIAN_POINT('Ctrl Pts',(51.4601407745289,3.75270098855345,42.3747044454606));
#24336=CARTESIAN_POINT('Ctrl Pts',(51.5640280213028,3.95578770363038,42.2518397579902));
#24337=CARTESIAN_POINT('Ctrl Pts',(51.6739780854953,4.1515305695143,42.1220580223104));
#24338=CARTESIAN_POINT('Ctrl Pts',(51.7933202450361,4.36399407738818,41.9811901408886));
#24339=CARTESIAN_POINT('Ctrl Pts',(51.919804621899,4.56780518704684,41.832173867876));
#24340=CARTESIAN_POINT('Ctrl Pts',(52.0520547200304,4.76289322778432,41.6767397588155));
#24341=CARTESIAN_POINT('Ctrl Pts',(52.1214830965618,4.86531013439127,41.5951402893094));
#24342=CARTESIAN_POINT('Ctrl Pts',(52.1925001533719,4.9653237612545,41.5117724248637));
#24343=CARTESIAN_POINT('Ctrl Pts',(52.2649051712575,5.06292908031616,41.4268879616273));
#24344=CARTESIAN_POINT('Ctrl Pts',(52.3120967308617,5.12654548932615,41.3715626496079));
#24345=CARTESIAN_POINT('Ctrl Pts',(52.3599068618714,5.18916334778516,41.3155609124478));
#24346=CARTESIAN_POINT('Ctrl Pts',(52.4082860638065,5.25078255038662,41.2589457946924));
#24347=CARTESIAN_POINT('Ctrl Pts',(52.7202424682068,5.64811247970936,40.8938829605977));
#24348=CARTESIAN_POINT('Ctrl Pts',(53.0558615152328,6.00392110101613,40.5033140822927));
#24349=CARTESIAN_POINT('Ctrl Pts',(53.4085173529738,6.32279271823725,40.0959222298945));
#24350=CARTESIAN_POINT('Ctrl Pts',(53.641979521913,6.53388934957749,39.826224197733));
#24351=CARTESIAN_POINT('Ctrl Pts',(53.8829080025842,6.72879759239876,39.5491538062669));
#24352=CARTESIAN_POINT('Ctrl Pts',(54.1293733297254,6.90884566929533,39.2672410660208));
#24353=CARTESIAN_POINT('Ctrl Pts',(54.2994228263867,7.03307038360392,39.0727345196546));
#24354=CARTESIAN_POINT('Ctrl Pts',(54.4721077718443,7.15022117656695,38.875923214831));
#24355=CARTESIAN_POINT('Ctrl Pts',(54.6472464829213,7.26041604117073,38.6771203410467));
#24356=CARTESIAN_POINT('Ctrl Pts',(54.9696401158298,7.46326167426362,38.3111659479952));
#24357=CARTESIAN_POINT('Ctrl Pts',(55.2997861374957,7.6426576925173,37.9390118616385));
#24358=CARTESIAN_POINT('Ctrl Pts',(55.6365936394474,7.79941676002793,37.5625544660927));
#24359=CARTESIAN_POINT('Ctrl Pts',(56.0062120435004,7.97144688411473,37.1494235799654));
#24360=CARTESIAN_POINT('Ctrl Pts',(56.3838529220466,8.11621342061613,36.7311104385792));
#24361=CARTESIAN_POINT('Ctrl Pts',(56.7680476094898,8.23474387868071,36.3101601802102));
#24362=CARTESIAN_POINT('Ctrl Pts',(57.1913088001799,8.36532700346917,35.8464059602747));
#24363=CARTESIAN_POINT('Ctrl Pts',(57.6225246054172,8.46406571536722,35.3794511113515));
#24364=CARTESIAN_POINT('Ctrl Pts',(58.0596999375003,8.53230441069762,34.9127398648411));
#24365=CARTESIAN_POINT('Ctrl Pts',(58.0966419874149,8.53807069507829,34.8733019805439));
#24366=CARTESIAN_POINT('Ctrl Pts',(58.1336265730028,8.54361918421598,34.8338658580828));
#24367=CARTESIAN_POINT('Ctrl Pts',(58.170652480092,8.54895068510073,34.7944335879392));
#24368=CARTESIAN_POINT('Ctrl Pts',(58.5551743043278,8.60431944193314,34.3849211778079));
#24369=CARTESIAN_POINT('Ctrl Pts',(58.9441544561351,8.63628571489729,33.9758224439262));
#24370=CARTESIAN_POINT('Ctrl Pts',(59.336276225615,8.64326314471869,33.5693475219187));
#24371=CARTESIAN_POINT('Ctrl Pts',(59.658536886301,8.64899746328794,33.235290891775));
#24372=CARTESIAN_POINT('Ctrl Pts',(59.9831665395922,8.63812999453601,32.9026794425133));
#24373=CARTESIAN_POINT('Ctrl Pts',(60.3092847224631,8.60972594452936,32.5729022773846));
#24374=CARTESIAN_POINT('Ctrl Pts',(60.6235699359896,8.58235251553876,32.255090845203));
#24375=CARTESIAN_POINT('Ctrl Pts',(60.9392371253881,8.53869186336392,31.9399124481438));
#24376=CARTESIAN_POINT('Ctrl Pts',(61.2554899897929,8.47795384680794,31.6286113065427));
#24377=CARTESIAN_POINT('Ctrl Pts',(61.5034619132754,8.43032954205346,31.3845219984178));
#24378=CARTESIAN_POINT('Ctrl Pts',(61.751793684675,8.37220685580352,31.1428165614412));
#24379=CARTESIAN_POINT('Ctrl Pts',(62.0001005262926,8.30322713190806,30.9040911403702));
#24380=CARTESIAN_POINT('Ctrl Pts',(62.0090216939304,8.30119416254679,30.8953945223182));
#24381=CARTESIAN_POINT('Ctrl Pts',(62.0061846213717,8.30198895980305,30.8981203196454));
#24382=CARTESIAN_POINT('Ctrl Pts',(62.0033475485117,8.30278233098926,30.9008465054417));
#24383=CARTESIAN_POINT('Ctrl Pts',(62.0005104758444,8.30357427665019,30.9035730788998));
#24384=CARTESIAN_POINT('',(54.0004882446407,-5.63129358982506E-5,44.8276698544958));
#24385=CARTESIAN_POINT('Ctrl Pts',(63.3333333333334,6.59966329107444,31.7128621774316));
#24386=CARTESIAN_POINT('Ctrl Pts',(62.1773896945574,7.00835108389839,33.1107619749047));
#24387=CARTESIAN_POINT('Ctrl Pts',(59.8510643212503,7.17136627556463,36.1604788683916));
#24388=CARTESIAN_POINT('Ctrl Pts',(57.1837550511065,6.08049991760512,40.0089963598732));
#24389=CARTESIAN_POINT('Ctrl Pts',(55.3668248198271,4.31461669518687,42.7323293863949));
#24390=CARTESIAN_POINT('Ctrl Pts',(54.4251147577635,2.64876740625127,44.1726835846802));
#24391=CARTESIAN_POINT('Ctrl Pts',(54.0471985724064,1.0930134915766,44.7556237601027));
#24392=CARTESIAN_POINT('Ctrl Pts',(54.0003896413325,0.273205195412317,44.8278246929999));
#24393=CARTESIAN_POINT('Ctrl Pts',(54.0004882446406,-5.63129358982679E-5,
44.8276698544958));
#24394=CARTESIAN_POINT('Ctrl Pts',(54.0004882243341,5.92031391855041E-7,
44.8276698863898));
#24395=CARTESIAN_POINT('Ctrl Pts',(54.0005846376296,-0.273232435743518,
44.8275184265616));
#24396=CARTESIAN_POINT('Ctrl Pts',(54.0479720776823,-1.09287079602173,44.7544086895179));
#24397=CARTESIAN_POINT('Ctrl Pts',(54.3610359933426,-2.38837584180055,44.2714261991957));
#24398=CARTESIAN_POINT('Ctrl Pts',(55.0050244523723,-3.70114923515179,43.2855805513825));
#24399=CARTESIAN_POINT('Ctrl Pts',(55.8180315346338,-4.7647811160322,42.0547184493501));
#24400=CARTESIAN_POINT('Ctrl Pts',(57.3603596238608,-6.15480540711906,39.7540563319785));
#24401=CARTESIAN_POINT('Ctrl Pts',(59.8534489927889,-7.16888802237617,36.1571505333425));
#24402=CARTESIAN_POINT('Ctrl Pts',(62.177413277237,-7.00834274616208,33.1107334560203));
#24403=CARTESIAN_POINT('Ctrl Pts',(63.3333333333333,-6.59966329107444,31.7128621774316));
#24404=CARTESIAN_POINT('Ctrl Pts',(62.0090864865565,-8.30112520427131,30.8953235203139));
#24405=CARTESIAN_POINT('Ctrl Pts',(62.0062500143164,-8.30191935890931,30.8980486593436));
#24406=CARTESIAN_POINT('Ctrl Pts',(62.0034135456646,-8.30271208344451,30.9007741826053));
#24407=CARTESIAN_POINT('Ctrl Pts',(62.0005770810725,-8.3035033784451,30.9035000893158));
#24408=CARTESIAN_POINT('Origin',(62.,0.,0.));
#24409=CARTESIAN_POINT('',(62.,-32.,-3.91886975727153E-15));
#24410=CARTESIAN_POINT('Origin',(62.,0.,0.));
#24411=CARTESIAN_POINT('Origin',(62.,0.,0.));
#24412=CARTESIAN_POINT('Origin',(61.,0.,13.));
#24413=CARTESIAN_POINT('',(54.,-8.57252759403147E-16,-50.));
#24414=CARTESIAN_POINT('Origin',(61.,0.,-50.));
#24415=CARTESIAN_POINT('',(54.,-8.57252759403147E-16,13.));
#24416=CARTESIAN_POINT('',(54.,-8.57252759403147E-16,76.));
#24417=CARTESIAN_POINT('',(54.,-8.57252759403147E-16,13.));
#24418=CARTESIAN_POINT('Origin',(61.,0.,76.));
#24419=CARTESIAN_POINT('Origin',(53.,-25.,-65.));
#24420=CARTESIAN_POINT('',(53.,-33.,-65.));
#24421=CARTESIAN_POINT('Origin',(53.,-25.,-65.));
#24422=CARTESIAN_POINT('',(53.,-31.,-63.));
#24423=CARTESIAN_POINT('Origin',(53.,-31.,-65.));
#24424=CARTESIAN_POINT('Origin',(53.,-25.,-63.));
#24425=CARTESIAN_POINT('Origin',(57.,-31.,-65.));
#24426=CARTESIAN_POINT('',(61.776208734813,-31.,-63.));
#24427=CARTESIAN_POINT('',(60.2237912651869,-31.,-63.));
#24428=CARTESIAN_POINT('Ctrl Pts',(61.7762087348131,-31.,-63.));
#24429=CARTESIAN_POINT('Ctrl Pts',(61.7599416865592,-31.0010478526925,-63.));
#24430=CARTESIAN_POINT('Ctrl Pts',(61.7436725835362,-31.0020628978659,-63.0000008227015));
#24431=CARTESIAN_POINT('Ctrl Pts',(61.4851779611869,-31.0176669941819,-63.0000245808219));
#24432=CARTESIAN_POINT('Ctrl Pts',(61.2426971526137,-31.0249999999999,-63.000156256104));
#24433=CARTESIAN_POINT('Ctrl Pts',(60.7573028473861,-31.0249999999999,-63.000156256104));
#24434=CARTESIAN_POINT('Ctrl Pts',(60.5148220388123,-31.0176669941818,-63.0000245808219));
#24435=CARTESIAN_POINT('Ctrl Pts',(60.256327416464,-31.002062897866,-63.0000008227015));
#24436=CARTESIAN_POINT('Ctrl Pts',(60.2400583134407,-31.0010478526925,-63.));
#24437=CARTESIAN_POINT('Ctrl Pts',(60.2237912651869,-31.,-63.));
#24438=CARTESIAN_POINT('',(57.,-31.,-63.));
#24439=CARTESIAN_POINT('',(69.,-33.,-65.));
#24440=CARTESIAN_POINT('',(57.,-33.,-65.));
#24441=CARTESIAN_POINT('',(69.,-31.,-63.));
#24442=CARTESIAN_POINT('Origin',(69.,-31.,-65.));
#24443=CARTESIAN_POINT('',(57.,-31.,-63.));
#24444=CARTESIAN_POINT('Origin',(69.,-25.,-65.));
#24445=CARTESIAN_POINT('',(77.,-25.,-65.));
#24446=CARTESIAN_POINT('',(75.,-25.,-63.));
#24447=CARTESIAN_POINT('Origin',(75.,-25.,-65.));
#24448=CARTESIAN_POINT('Origin',(69.,-25.,-63.));
#24449=CARTESIAN_POINT('Origin',(69.,-25.,-65.));
#24450=CARTESIAN_POINT('Origin',(75.,-7.,-65.));
#24451=CARTESIAN_POINT('',(77.,-14.,-65.));
#24452=CARTESIAN_POINT('',(75.,-19.2915026221292,-63.));
#24453=CARTESIAN_POINT('Ctrl Pts',(75.,-19.2915026221292,-63.));
#24454=CARTESIAN_POINT('Ctrl Pts',(75.6598443730912,-18.5433094298986,-63.));
#24455=CARTESIAN_POINT('Ctrl Pts',(76.1700160324087,-17.6794947918718,-63.2991643782353));
#24456=CARTESIAN_POINT('Ctrl Pts',(76.8431824332822,-15.8525818385792,-64.0701256324549));
#24457=CARTESIAN_POINT('Ctrl Pts',(77.,-14.8922724470027,-64.5538637764986));
#24458=CARTESIAN_POINT('Ctrl Pts',(77.,-14.,-65.));
#24459=CARTESIAN_POINT('',(75.,-7.,-63.));
#24460=CARTESIAN_POINT('',(77.,-7.,-65.));
#24461=CARTESIAN_POINT('Origin',(53.,-33.,-77.));
#24462=CARTESIAN_POINT('',(53.,-33.,-75.));
#24463=CARTESIAN_POINT('',(53.,-33.,-77.));
#24464=CARTESIAN_POINT('',(69.,-33.,-75.));
#24465=CARTESIAN_POINT('',(57.,-33.,-75.));
#24466=CARTESIAN_POINT('',(69.,-33.,-77.));
#24467=CARTESIAN_POINT('Origin',(53.,-25.,-77.));
#24468=CARTESIAN_POINT('',(45.,-25.,-75.));
#24469=CARTESIAN_POINT('',(45.,-25.,-77.));
#24470=CARTESIAN_POINT('Origin',(53.,-25.,-75.));
#24471=CARTESIAN_POINT('Origin',(61.,0.,-63.));
#24472=CARTESIAN_POINT('Origin',(61.,-25.,-63.));
#24473=CARTESIAN_POINT('Origin',(53.,-14.,-63.));
#24474=CARTESIAN_POINT('Origin',(61.,-25.,-65.));
#24475=CARTESIAN_POINT('Origin',(61.,-25.,-63.));
#24476=CARTESIAN_POINT('Origin',(69.,25.,-75.));
#24477=CARTESIAN_POINT('',(77.,25.,-75.));
#24478=CARTESIAN_POINT('Origin',(75.,25.,-75.));
#24479=CARTESIAN_POINT('',(69.,33.,-75.));
#24480=CARTESIAN_POINT('Origin',(69.,31.,-75.));
#24481=CARTESIAN_POINT('Origin',(69.,25.,-75.));
#24482=CARTESIAN_POINT('Origin',(65.,31.,-75.));
#24483=CARTESIAN_POINT('',(53.,33.,-75.));
#24484=CARTESIAN_POINT('Origin',(53.,31.,-75.));
#24485=CARTESIAN_POINT('',(65.,33.,-75.));
#24486=CARTESIAN_POINT('Origin',(53.,25.,-75.));
#24487=CARTESIAN_POINT('',(45.,25.,-75.));
#24488=CARTESIAN_POINT('Origin',(47.,25.,-75.));
#24489=CARTESIAN_POINT('Origin',(53.,25.,-75.));
#24490=CARTESIAN_POINT('Origin',(47.,7.,-75.));
#24491=CARTESIAN_POINT('Origin',(47.,-25.,-75.));
#24492=CARTESIAN_POINT('',(45.,7.,-75.));
#24493=CARTESIAN_POINT('Origin',(53.,-25.,-75.));
#24494=CARTESIAN_POINT('Origin',(53.,-31.,-75.));
#24495=CARTESIAN_POINT('Origin',(57.,-31.,-75.));
#24496=CARTESIAN_POINT('Origin',(69.,-31.,-75.));
#24497=CARTESIAN_POINT('Origin',(69.,-25.,-75.));
#24498=CARTESIAN_POINT('',(77.,-25.,-75.));
#24499=CARTESIAN_POINT('Origin',(75.,-25.,-75.));
#24500=CARTESIAN_POINT('Origin',(69.,-25.,-75.));
#24501=CARTESIAN_POINT('Origin',(75.,-7.,-75.));
#24502=CARTESIAN_POINT('',(77.,-7.,-75.));
#24503=CARTESIAN_POINT('Origin',(69.,-25.,-77.));
#24504=CARTESIAN_POINT('',(77.,-25.,-77.));
#24505=CARTESIAN_POINT('Origin',(77.,-14.,-77.));
#24506=CARTESIAN_POINT('',(77.,25.,-65.));
#24507=CARTESIAN_POINT('',(77.,25.,-77.));
#24508=CARTESIAN_POINT('',(77.,14.,-65.));
#24509=CARTESIAN_POINT('',(77.,-7.,-65.));
#24510=CARTESIAN_POINT('',(77.,14.,-77.));
#24511=CARTESIAN_POINT('',(77.,-14.,-77.));
#24512=CARTESIAN_POINT('Origin',(69.,25.,-77.));
#24513=CARTESIAN_POINT('',(69.,33.,-65.));
#24514=CARTESIAN_POINT('',(69.,33.,-77.));
#24515=CARTESIAN_POINT('Origin',(69.,25.,-65.));
#24516=CARTESIAN_POINT('Origin',(75.,-7.,-65.));
#24517=CARTESIAN_POINT('',(75.,25.,-63.));
#24518=CARTESIAN_POINT('Origin',(75.,25.,-65.));
#24519=CARTESIAN_POINT('',(75.,19.2915026221292,-63.));
#24520=CARTESIAN_POINT('',(75.,-7.,-63.));
#24521=CARTESIAN_POINT('Ctrl Pts',(77.,14.,-65.));
#24522=CARTESIAN_POINT('Ctrl Pts',(77.,14.8922724470027,-64.5538637764986));
#24523=CARTESIAN_POINT('Ctrl Pts',(76.8431824332822,15.8525818385793,-64.0701256324549));
#24524=CARTESIAN_POINT('Ctrl Pts',(76.1700160324087,17.6794947918718,-63.2991643782353));
#24525=CARTESIAN_POINT('Ctrl Pts',(75.6598443730912,18.5433094298986,-63.));
#24526=CARTESIAN_POINT('Ctrl Pts',(75.,19.2915026221292,-63.));
#24527=CARTESIAN_POINT('Origin',(69.,25.,-65.));
#24528=CARTESIAN_POINT('',(69.,31.,-63.));
#24529=CARTESIAN_POINT('Origin',(69.,31.,-65.));
#24530=CARTESIAN_POINT('Origin',(69.,25.,-63.));
#24531=CARTESIAN_POINT('Origin',(65.,31.,-65.));
#24532=CARTESIAN_POINT('',(60.2237912651869,31.,-63.));
#24533=CARTESIAN_POINT('',(61.776208734813,31.,-63.));
#24534=CARTESIAN_POINT('Ctrl Pts',(60.2237912651869,31.,-63.));
#24535=CARTESIAN_POINT('Ctrl Pts',(60.2400583134408,31.0010478526925,-63.));
#24536=CARTESIAN_POINT('Ctrl Pts',(60.2563274164638,31.0020628978659,-63.0000008227015));
#24537=CARTESIAN_POINT('Ctrl Pts',(60.5148220388131,31.0176669941819,-63.0000245808219));
#24538=CARTESIAN_POINT('Ctrl Pts',(60.7573028473863,31.0249999999999,-63.000156256104));
#24539=CARTESIAN_POINT('Ctrl Pts',(61.2426971526137,31.0249999999999,-63.000156256104));
#24540=CARTESIAN_POINT('Ctrl Pts',(61.4851779611869,31.0176669941819,-63.0000245808219));
#24541=CARTESIAN_POINT('Ctrl Pts',(61.7436725835362,31.0020628978659,-63.0000008227015));
#24542=CARTESIAN_POINT('Ctrl Pts',(61.7599416865592,31.0010478526925,-63.));
#24543=CARTESIAN_POINT('Ctrl Pts',(61.7762087348131,31.,-63.));
#24544=CARTESIAN_POINT('',(65.,31.,-63.));
#24545=CARTESIAN_POINT('',(53.,33.,-65.));
#24546=CARTESIAN_POINT('',(65.,33.,-65.));
#24547=CARTESIAN_POINT('',(53.,31.,-63.));
#24548=CARTESIAN_POINT('Origin',(53.,31.,-65.));
#24549=CARTESIAN_POINT('',(65.,31.,-63.));
#24550=CARTESIAN_POINT('Origin',(53.,25.,-65.));
#24551=CARTESIAN_POINT('Origin',(53.,25.,-63.));
#24552=CARTESIAN_POINT('Origin',(53.,25.,-65.));
#24553=CARTESIAN_POINT('Origin',(61.,0.,-63.));
#24554=CARTESIAN_POINT('Origin',(53.,14.,-63.));
#24555=CARTESIAN_POINT('Origin',(61.,25.,-63.));
#24556=CARTESIAN_POINT('Origin',(61.,0.,-63.));
#24557=CARTESIAN_POINT('Origin',(61.,25.,-63.));
#24558=CARTESIAN_POINT('Origin',(69.,14.,-63.));
#24559=CARTESIAN_POINT('Origin',(61.,25.,-65.));
#24560=CARTESIAN_POINT('Origin',(80.,2.,-8.));
#24561=CARTESIAN_POINT('Origin',(80.,-1.11022302462516E-15,-8.));
#24562=CARTESIAN_POINT('Origin',(80.,-4.9960036108132E-15,-26.75));
#24563=CARTESIAN_POINT('Origin',(80.,-6.10622663543836E-15,-33.));
#24564=CARTESIAN_POINT('Origin',(80.,5.92820323027551,5.73205080756888));
#24565=CARTESIAN_POINT('Origin',(80.,6.92820323027551,4.));
#24566=CARTESIAN_POINT('Origin',(80.,23.1661795512337,13.375));
#24567=CARTESIAN_POINT('Origin',(80.,28.5788383248865,16.5));
#24568=CARTESIAN_POINT('Origin',(80.,-2.,8.));
#24569=CARTESIAN_POINT('Origin',(80.,2.77555756156289E-16,8.));
#24570=CARTESIAN_POINT('Origin',(80.,1.80411241501588E-15,26.75));
#24571=CARTESIAN_POINT('Origin',(80.,2.22044604925031E-15,33.));
#24572=CARTESIAN_POINT('Origin',(80.,-7.92820323027551,2.26794919243112));
#24573=CARTESIAN_POINT('Origin',(80.,-6.92820323027551,4.));
#24574=CARTESIAN_POINT('Origin',(80.,-23.1661795512337,13.375));
#24575=CARTESIAN_POINT('Origin',(80.,-28.5788383248865,16.5));
#24576=CARTESIAN_POINT('Origin',(80.,-5.92820323027551,-5.73205080756888));
#24577=CARTESIAN_POINT('Origin',(80.,-6.92820323027551,-4.));
#24578=CARTESIAN_POINT('Origin',(80.,-23.1661795512337,-13.375));
#24579=CARTESIAN_POINT('Origin',(80.,-28.5788383248865,-16.5));
#24580=CARTESIAN_POINT('Origin',(80.,7.92820323027551,-2.26794919243113));
#24581=CARTESIAN_POINT('Origin',(80.,6.92820323027551,-4.));
#24582=CARTESIAN_POINT('Origin',(80.,23.1661795512337,-13.375));
#24583=CARTESIAN_POINT('Origin',(80.,28.5788383248865,-16.5));
#24584=CARTESIAN_POINT('Origin',(80.,27.5788383248865,-18.2320508075689));
#24585=CARTESIAN_POINT('Origin',(80.,-29.5788383248865,-14.7679491924311));
#24586=CARTESIAN_POINT('Origin',(80.,-27.5788383248865,18.2320508075689));
#24587=CARTESIAN_POINT('Origin',(80.,2.,33.));
#24588=CARTESIAN_POINT('Origin',(80.,29.5788383248865,14.7679491924311));
#24589=CARTESIAN_POINT('Origin',(80.,-2.00000000000001,-33.));
#24590=CARTESIAN_POINT('Origin',(61.,25.,68.));
#24591=CARTESIAN_POINT('Origin',(61.,-25.,68.));
#24592=CARTESIAN_POINT('Origin',(61.,25.,-63.));
#24593=CARTESIAN_POINT('Origin',(61.,-25.,-63.));
#24594=CARTESIAN_POINT('Origin',(61.,0.,-63.));
#24595=CARTESIAN_POINT('Origin',(69.,-14.,-63.));
#24596=CARTESIAN_POINT('Origin',(38.,-31.,-53.6935750346352));
#24597=CARTESIAN_POINT('',(38.,-31.,-49.1935750346352));
#24598=CARTESIAN_POINT('Origin',(38.,62.,0.));
#24599=CARTESIAN_POINT('',(38.,62.,4.5));
#24600=CARTESIAN_POINT('Origin',(38.,31.,53.6935750346352));
#24601=CARTESIAN_POINT('',(38.,31.,58.1935750346352));
#24602=CARTESIAN_POINT('Origin',(38.,-31.,53.6935750346352));
#24603=CARTESIAN_POINT('',(38.,-31.,58.1935750346352));
#24604=CARTESIAN_POINT('Origin',(38.,-62.,7.59281015471359E-15));
#24605=CARTESIAN_POINT('',(38.,-62.,4.50000000000001));
#24606=CARTESIAN_POINT('Origin',(38.,31.,-53.6935750346352));
#24607=CARTESIAN_POINT('',(38.,31.,-49.1935750346352));
#24608=CARTESIAN_POINT('Origin',(61.,0.,-74.05));
#24609=CARTESIAN_POINT('',(47.95,-1.5981640728873E-15,-71.));
#24610=CARTESIAN_POINT('',(47.95,-1.5981640728873E-15,-74.05));
#24611=CARTESIAN_POINT('Origin',(61.,0.,-71.));
#24612=CARTESIAN_POINT('Origin',(72.,0.,-71.));
#24613=CARTESIAN_POINT('',(50.,-1.34711147906209E-15,-71.));
#24614=CARTESIAN_POINT('Origin',(61.,0.,-71.));
#24615=CARTESIAN_POINT('Origin',(61.,0.,-60.5));
#24616=CARTESIAN_POINT('',(50.,-1.34711147906209E-15,-50.));
#24617=CARTESIAN_POINT('',(50.,-1.34711147906209E-15,-60.5));
#24618=CARTESIAN_POINT('Origin',(61.,0.,-50.));
#24619=CARTESIAN_POINT('Origin',(68.,0.,-50.));
#24620=CARTESIAN_POINT('Origin',(74.05,0.,76.));
#24621=CARTESIAN_POINT('',(47.95,-1.5981640728873E-15,76.));
#24622=CARTESIAN_POINT('Origin',(61.,0.,76.));
#24623=CARTESIAN_POINT('Origin',(61.,0.,79.05));
#24624=CARTESIAN_POINT('',(47.95,-1.5981640728873E-15,79.05));
#24625=CARTESIAN_POINT('Origin',(56.,0.,0.));
#24626=CARTESIAN_POINT('',(56.,-38.,-4.65365783675994E-15));
#24627=CARTESIAN_POINT('Origin',(62.,0.,0.));
#24628=CARTESIAN_POINT('Origin',(62.,0.,0.));
#24629=CARTESIAN_POINT('Origin',(69.,-25.,65.));
#24630=CARTESIAN_POINT('',(69.,-33.,65.));
#24631=CARTESIAN_POINT('Origin',(53.,-33.,65.));
#24632=CARTESIAN_POINT('',(53.,-33.,65.));
#24633=CARTESIAN_POINT('Origin',(53.,-25.,65.));
#24634=CARTESIAN_POINT('',(45.,-25.,65.));
#24635=CARTESIAN_POINT('Origin',(53.,25.,-77.));
#24636=CARTESIAN_POINT('',(45.,25.,-77.));
#24637=CARTESIAN_POINT('',(53.,33.,-77.));
#24638=CARTESIAN_POINT('Origin',(69.,33.,-77.));
#24639=CARTESIAN_POINT('Origin',(53.,14.,-77.));
#24640=CARTESIAN_POINT('Origin',(45.,14.,-77.));
#24641=CARTESIAN_POINT('Origin',(45.,14.,-77.));
#24642=CARTESIAN_POINT('Origin',(53.,-14.,-77.));
#24643=CARTESIAN_POINT('Origin',(53.,-14.,-77.));
#24644=CARTESIAN_POINT('',(53.,-22.,-77.));
#24645=CARTESIAN_POINT('Origin',(69.,14.,-77.));
#24646=CARTESIAN_POINT('Origin',(69.,-14.,-77.));
#24647=CARTESIAN_POINT('Origin',(53.,-22.,-77.));
#24648=CARTESIAN_POINT('',(69.,-22.,-77.));
#24649=CARTESIAN_POINT('Origin',(53.,14.,-77.));
#24650=CARTESIAN_POINT('',(53.,22.,-77.));
#24651=CARTESIAN_POINT('Origin',(69.,22.,-77.));
#24652=CARTESIAN_POINT('',(69.,22.,-77.));
#24653=CARTESIAN_POINT('Origin',(69.,14.,-77.));
#24654=CARTESIAN_POINT('Origin',(69.,-14.,-77.));
#24655=CARTESIAN_POINT('',(0.,0.,0.));
#24656=CARTESIAN_POINT('Origin',(-14.,-71.8232233047034,30.));
#24657=CARTESIAN_POINT('',(-25.3535533905933,-71.6464466094067,30.));
#24658=CARTESIAN_POINT('Origin',(-14.,-71.6464466094067,30.));
#24659=CARTESIAN_POINT('',(-24.5,-72.,30.));
#24660=CARTESIAN_POINT('',(-24.9267766952966,-71.8232233047034,30.));
#24661=CARTESIAN_POINT('Origin',(-14.,-72.,30.));
#24662=CARTESIAN_POINT('Origin',(-14.,-71.5,30.));
#24663=CARTESIAN_POINT('',(-25.6464466094067,-71.3535533905933,30.));
#24664=CARTESIAN_POINT('',(-25.5,-71.5,30.));
#24665=CARTESIAN_POINT('Origin',(-14.,-71.3535533905933,30.));
#24666=CARTESIAN_POINT('Origin',(-14.,-72.,30.));
#24667=CARTESIAN_POINT('',(-20.9,-72.,30.));
#24668=CARTESIAN_POINT('Origin',(-14.,-72.,30.));
#24669=CARTESIAN_POINT('Origin',(-14.,-70.9267766952966,30.));
#24670=CARTESIAN_POINT('',(-26.,-70.5,30.));
#24671=CARTESIAN_POINT('',(-25.8232233047034,-70.9267766952966,30.));
#24672=CARTESIAN_POINT('Origin',(-14.,-70.5,30.));
#24673=CARTESIAN_POINT('Origin',(-14.,-50.,30.));
#24674=CARTESIAN_POINT('',(-26.,-63.2455532033676,30.));
#24675=CARTESIAN_POINT('',(-26.,-50.,30.));
#24676=CARTESIAN_POINT('',(-14.,-67.6461381011511,18.));
#24677=CARTESIAN_POINT('Ctrl Pts',(-14.,-67.6461381011511,18.));
#24678=CARTESIAN_POINT('Ctrl Pts',(-15.4974143374287,-67.6461381011511,
18.));
#24679=CARTESIAN_POINT('Ctrl Pts',(-17.0915205041766,-67.569001302991,18.2980124136255));
#24680=CARTESIAN_POINT('Ctrl Pts',(-20.0138657590624,-67.2330346371868,
19.4963139645897));
#24681=CARTESIAN_POINT('Ctrl Pts',(-21.3418872514445,-66.9712006520621,
20.3962895865205));
#24682=CARTESIAN_POINT('Ctrl Pts',(-23.5213138818415,-66.2867646794087,
22.5260020891911));
#24683=CARTESIAN_POINT('Ctrl Pts',(-24.4747045274443,-65.8046030416515,
23.9238828818556));
#24684=CARTESIAN_POINT('Ctrl Pts',(-25.713131811207,-64.6337042024678,26.9273511571404));
#24685=CARTESIAN_POINT('Ctrl Pts',(-26.,-63.9422944830207,28.5311404109572));
#24686=CARTESIAN_POINT('Ctrl Pts',(-26.,-63.2455532033676,30.));
#24687=CARTESIAN_POINT('Ctrl Pts',(-26.,-63.2455532033676,30.));
#24688=CARTESIAN_POINT('Ctrl Pts',(-26.,-62.496760426176,31.5785937809389));
#24689=CARTESIAN_POINT('Ctrl Pts',(-25.6727630693155,-61.6315633847307,
33.2354648264254));
#24690=CARTESIAN_POINT('Ctrl Pts',(-24.366604146322,-59.898806525139,36.2653926472075));
#24691=CARTESIAN_POINT('Ctrl Pts',(-23.3890813807094,-59.033283877067,37.6402168655692));
#24692=CARTESIAN_POINT('Ctrl Pts',(-21.2292573598961,-57.6805770802603,
39.6766954896892));
#24693=CARTESIAN_POINT('Ctrl Pts',(-19.952736536109,-57.0753995031866,40.5328837235444));
#24694=CARTESIAN_POINT('Ctrl Pts',(-17.8109551249349,-56.4425965862802,
41.4048580623199));
#24695=CARTESIAN_POINT('Ctrl Pts',(-17.0595209591031,-56.2763096504852,
41.6294531705792));
#24696=CARTESIAN_POINT('Ctrl Pts',(-15.5328204392415,-56.0549204173022,
41.9270830875605));
#24697=CARTESIAN_POINT('Ctrl Pts',(-14.7575047347341,-56.,42.));
#24698=CARTESIAN_POINT('Ctrl Pts',(-13.2424952652659,-56.,42.));
#24699=CARTESIAN_POINT('Ctrl Pts',(-12.4671795607585,-56.0549204173022,
41.9270830875605));
#24700=CARTESIAN_POINT('Ctrl Pts',(-10.9404790408969,-56.2763096504852,
41.6294531705792));
#24701=CARTESIAN_POINT('Ctrl Pts',(-10.1890448750651,-56.4425965862802,
41.4048580623199));
#24702=CARTESIAN_POINT('Ctrl Pts',(-8.04726346389096,-57.0753995031866,
40.5328837235444));
#24703=CARTESIAN_POINT('Ctrl Pts',(-6.77074264010388,-57.6805770802603,
39.6766954896892));
#24704=CARTESIAN_POINT('Ctrl Pts',(-4.61091861929063,-59.033283877067,37.6402168655692));
#24705=CARTESIAN_POINT('Ctrl Pts',(-3.63339585367803,-59.898806525139,36.2653926472075));
#24706=CARTESIAN_POINT('Ctrl Pts',(-2.32723693068453,-61.6315633847307,
33.2354648264254));
#24707=CARTESIAN_POINT('Ctrl Pts',(-2.,-62.496760426176,31.578593780939));
#24708=CARTESIAN_POINT('Ctrl Pts',(-2.,-63.9422944830207,28.5311404109573));
#24709=CARTESIAN_POINT('Ctrl Pts',(-2.28686818879297,-64.6337042024678,
26.9273511571404));
#24710=CARTESIAN_POINT('Ctrl Pts',(-3.52529547255565,-65.8046030416515,
23.9238828818556));
#24711=CARTESIAN_POINT('Ctrl Pts',(-4.47868611815846,-66.2867646794087,
22.5260020891911));
#24712=CARTESIAN_POINT('Ctrl Pts',(-6.65811274855545,-66.9712006520621,
20.3962895865205));
#24713=CARTESIAN_POINT('Ctrl Pts',(-7.98613424093757,-67.2330346371868,
19.4963139645897));
#24714=CARTESIAN_POINT('Ctrl Pts',(-10.9084794958234,-67.569001302991,18.2980124136255));
#24715=CARTESIAN_POINT('Ctrl Pts',(-12.5025856625713,-67.6461381011511,
18.));
#24716=CARTESIAN_POINT('Ctrl Pts',(-14.,-67.6461381011511,18.));
#24717=CARTESIAN_POINT('Origin',(-0.8,0.,0.));
#24718=CARTESIAN_POINT('',(-0.5,69.4,-8.49904878608263E-15));
#24719=CARTESIAN_POINT('Origin',(-0.5,0.,0.));
#24720=CARTESIAN_POINT('',(-1.1,70.,8.57252759403147E-15));
#24721=CARTESIAN_POINT('',(-0.8,69.7,8.53578819005705E-15));
#24722=CARTESIAN_POINT('',(-1.1,-70.,-8.57252759403147E-15));
#24723=CARTESIAN_POINT('Origin',(-1.1,0.,0.));
#24724=CARTESIAN_POINT('Origin',(-1.1,0.,0.));
#24725=CARTESIAN_POINT('Origin',(-17.5,0.,0.));
#24726=CARTESIAN_POINT('',(-34.5,-70.,-8.57252759403147E-15));
#24727=CARTESIAN_POINT('',(-17.5,-70.,-8.57252759403147E-15));
#24728=CARTESIAN_POINT('Origin',(-34.5,0.,0.));
#24729=CARTESIAN_POINT('Origin',(-0.5,8.05,0.));
#24730=CARTESIAN_POINT('',(-0.5,-31.,-49.1935750346352));
#24731=CARTESIAN_POINT('Origin',(-0.5,-31.,-53.6935750346352));
#24732=CARTESIAN_POINT('',(-0.5,62.,4.5));
#24733=CARTESIAN_POINT('Origin',(-0.5,62.,0.));
#24734=CARTESIAN_POINT('',(-0.5,31.,58.1935750346352));
#24735=CARTESIAN_POINT('Origin',(-0.5,31.,53.6935750346352));
#24736=CARTESIAN_POINT('',(-0.5,-31.,58.1935750346352));
#24737=CARTESIAN_POINT('Origin',(-0.5,-31.,53.6935750346352));
#24738=CARTESIAN_POINT('',(-0.5,-62.,4.50000000000001));
#24739=CARTESIAN_POINT('Origin',(-0.5,-62.,7.59281015471359E-15));
#24740=CARTESIAN_POINT('',(-0.5,31.,-49.1935750346352));
#24741=CARTESIAN_POINT('Origin',(-0.5,31.,-53.6935750346352));
#24742=CARTESIAN_POINT('',(-0.5,-8.05,-9.85840673313619E-16));
#24743=CARTESIAN_POINT('Origin',(-0.5,0.,0.));
#24744=CARTESIAN_POINT('Origin',(-14.,-72.,30.));
#24745=CARTESIAN_POINT('',(-20.9,-60.,30.));
#24746=CARTESIAN_POINT('',(-20.9,-72.,30.));
#24747=CARTESIAN_POINT('Origin',(-14.,-60.,30.));
#24748=CARTESIAN_POINT('Origin',(-14.,-60.,30.));
#24749=CARTESIAN_POINT('Origin',(-0.4,-31.,-53.6935750346352));
#24750=CARTESIAN_POINT('',(-35.5,-31.,-49.1935750346352));
#24751=CARTESIAN_POINT('',(-0.4,-31.,-49.1935750346352));
#24752=CARTESIAN_POINT('Origin',(-35.5,-31.,-53.6935750346352));
#24753=CARTESIAN_POINT('Origin',(-0.4,62.,0.));
#24754=CARTESIAN_POINT('',(-35.5,62.,4.5));
#24755=CARTESIAN_POINT('',(-0.4,62.,4.5));
#24756=CARTESIAN_POINT('Origin',(-35.5,62.,0.));
#24757=CARTESIAN_POINT('Origin',(-0.4,31.,53.6935750346352));
#24758=CARTESIAN_POINT('',(-35.5,31.,58.1935750346352));
#24759=CARTESIAN_POINT('',(-0.4,31.,58.1935750346352));
#24760=CARTESIAN_POINT('Origin',(-35.5,31.,53.6935750346352));
#24761=CARTESIAN_POINT('Origin',(-0.4,-31.,53.6935750346352));
#24762=CARTESIAN_POINT('',(-35.5,-31.,58.1935750346352));
#24763=CARTESIAN_POINT('',(-0.4,-31.,58.1935750346352));
#24764=CARTESIAN_POINT('Origin',(-35.5,-31.,53.6935750346352));
#24765=CARTESIAN_POINT('Origin',(-0.4,-62.,7.59281015471359E-15));
#24766=CARTESIAN_POINT('',(-35.5,-62.,4.50000000000001));
#24767=CARTESIAN_POINT('',(-0.4,-62.,4.50000000000001));
#24768=CARTESIAN_POINT('Origin',(-35.5,-62.,7.59281015471359E-15));
#24769=CARTESIAN_POINT('Origin',(-0.4,31.,-53.6935750346352));
#24770=CARTESIAN_POINT('',(-35.5,31.,-49.1935750346352));
#24771=CARTESIAN_POINT('',(-0.4,31.,-49.1935750346352));
#24772=CARTESIAN_POINT('Origin',(-35.5,31.,-53.6935750346352));
#24773=CARTESIAN_POINT('Origin',(-20.,35.,0.));
#24774=CARTESIAN_POINT('',(-20.,-35.,-4.28626379701574E-15));
#24775=CARTESIAN_POINT('Origin',(-20.,0.,0.));
#24776=CARTESIAN_POINT('',(-20.,-8.05,-9.85840673313619E-16));
#24777=CARTESIAN_POINT('Origin',(-20.,0.,0.));
#24778=CARTESIAN_POINT('Origin',(-23.,0.,0.));
#24779=CARTESIAN_POINT('',(-26.,-45.,-5.51091059616309E-15));
#24780=CARTESIAN_POINT('',(-23.,-40.,-4.89858719658941E-15));
#24781=CARTESIAN_POINT('Origin',(-26.,0.,0.));
#24782=CARTESIAN_POINT('Origin',(-30.75,0.,0.));
#24783=CARTESIAN_POINT('',(-35.5,-50.,-6.12323399573677E-15));
#24784=CARTESIAN_POINT('',(-30.75,-47.5,-5.81707229594993E-15));
#24785=CARTESIAN_POINT('Origin',(-35.5,0.,0.));
#24786=CARTESIAN_POINT('Origin',(-35.5,69.,0.));
#24787=CARTESIAN_POINT('',(-35.5,-69.,-8.45006291411674E-15));
#24788=CARTESIAN_POINT('Origin',(-35.5,0.,0.));
#24789=CARTESIAN_POINT('Origin',(-35.,0.,0.));
#24790=CARTESIAN_POINT('',(-35.,-69.5,-8.51129525407411E-15));
#24791=CARTESIAN_POINT('Origin',(-10.25,0.,0.));
#24792=CARTESIAN_POINT('',(-10.25,-8.05,-9.85840673313619E-16));
#24793=CARTESIAN_POINT('',(0.,0.,0.));
#24794=CARTESIAN_POINT('Origin',(16.,69.8232233047034,-28.));
#24795=CARTESIAN_POINT('',(2.64644660940673,69.6464466094067,-28.));
#24796=CARTESIAN_POINT('Origin',(16.,69.6464466094067,-28.));
#24797=CARTESIAN_POINT('',(3.5,70.,-28.));
#24798=CARTESIAN_POINT('',(3.07322330470337,69.8232233047034,-28.));
#24799=CARTESIAN_POINT('Origin',(16.,70.,-28.));
#24800=CARTESIAN_POINT('Origin',(16.,69.5,-28.));
#24801=CARTESIAN_POINT('',(2.35355339059327,69.3535533905933,-28.));
#24802=CARTESIAN_POINT('',(2.5,69.5,-28.));
#24803=CARTESIAN_POINT('Origin',(16.,69.3535533905933,-28.));
#24804=CARTESIAN_POINT('Origin',(16.,70.,-28.));
#24805=CARTESIAN_POINT('',(7.4,70.,-28.));
#24806=CARTESIAN_POINT('Origin',(16.,70.,-28.));
#24807=CARTESIAN_POINT('Origin',(16.,68.9267766952966,-28.));
#24808=CARTESIAN_POINT('',(1.99999999999998,68.5,-28.));
#24809=CARTESIAN_POINT('',(2.17677669529664,68.9267766952966,-28.));
#24810=CARTESIAN_POINT('',(12.6224302964435,68.5,-14.4135353053998));
#24811=CARTESIAN_POINT('Origin',(16.,68.5,-28.));
#24812=CARTESIAN_POINT('',(19.3775697035565,68.5,-14.4135353053998));
#24813=CARTESIAN_POINT('Ctrl Pts',(19.3775697035564,68.5,-14.4135353053998));
#24814=CARTESIAN_POINT('Ctrl Pts',(18.2401900876009,68.5545924215965,-14.1540860585547));
#24815=CARTESIAN_POINT('Ctrl Pts',(17.0810687265813,68.5790231734206,-14.0327324701726));
#24816=CARTESIAN_POINT('Ctrl Pts',(14.9189312734187,68.5790231734206,-14.0327324701726));
#24817=CARTESIAN_POINT('Ctrl Pts',(13.7598099123991,68.5545924215965,-14.1540860585547));
#24818=CARTESIAN_POINT('Ctrl Pts',(12.6224302964436,68.5,-14.4135353053998));
#24819=CARTESIAN_POINT('Origin',(16.,68.5,-28.));
#24820=CARTESIAN_POINT('Origin',(0.8,0.,0.));
#24821=CARTESIAN_POINT('',(1.1,70.,-8.57252759403147E-15));
#24822=CARTESIAN_POINT('',(1.1,-70.,-8.57252759403147E-15));
#24823=CARTESIAN_POINT('Origin',(1.1,0.,0.));
#24824=CARTESIAN_POINT('Origin',(1.1,0.,0.));
#24825=CARTESIAN_POINT('',(0.5,69.4,8.49904878608263E-15));
#24826=CARTESIAN_POINT('',(0.8,69.7,8.53578819005705E-15));
#24827=CARTESIAN_POINT('Origin',(0.5,0.,0.));
#24828=CARTESIAN_POINT('Origin',(0.5,70.,0.));
#24829=CARTESIAN_POINT('',(0.5,-31.,-49.1935750346352));
#24830=CARTESIAN_POINT('Origin',(0.5,-31.,-53.6935750346352));
#24831=CARTESIAN_POINT('',(0.5,62.,4.5));
#24832=CARTESIAN_POINT('Origin',(0.5,62.,0.));
#24833=CARTESIAN_POINT('',(0.5,31.,58.1935750346352));
#24834=CARTESIAN_POINT('Origin',(0.5,31.,53.6935750346352));
#24835=CARTESIAN_POINT('',(0.5,-31.,58.1935750346352));
#24836=CARTESIAN_POINT('Origin',(0.5,-31.,53.6935750346352));
#24837=CARTESIAN_POINT('',(0.5,-62.,4.50000000000001));
#24838=CARTESIAN_POINT('Origin',(0.5,-62.,7.59281015471359E-15));
#24839=CARTESIAN_POINT('',(0.5,31.,-49.1935750346352));
#24840=CARTESIAN_POINT('Origin',(0.5,31.,-53.6935750346352));
#24841=CARTESIAN_POINT('',(0.5,-8.05,-9.85840673313619E-16));
#24842=CARTESIAN_POINT('Origin',(0.5,0.,0.));
#24843=CARTESIAN_POINT('Origin',(17.5,0.,0.));
#24844=CARTESIAN_POINT('',(34.5,-70.,-8.57252759403147E-15));
#24845=CARTESIAN_POINT('Origin',(34.5,0.,0.));
#24846=CARTESIAN_POINT('',(17.5,-70.,-8.57252759403147E-15));
#24847=CARTESIAN_POINT('Ctrl Pts',(12.6224302964435,68.5,-14.4135353053998));
#24848=CARTESIAN_POINT('Ctrl Pts',(11.961651315758,68.4654352022338,-14.5778037237174));
#24849=CARTESIAN_POINT('Ctrl Pts',(11.3086498622677,68.4198540566006,-14.7917039729986));
#24850=CARTESIAN_POINT('Ctrl Pts',(8.96544243852918,68.2077217953467,-15.7551700622329));
#24851=CARTESIAN_POINT('Ctrl Pts',(7.4085187040214,67.9622849181329,-16.8132432389867));
#24852=CARTESIAN_POINT('Ctrl Pts',(5.52865282034834,67.4697026576732,-18.662322985451));
#24853=CARTESIAN_POINT('Ctrl Pts',(4.92185391533271,67.2665458430878,-19.3877268629585));
#24854=CARTESIAN_POINT('Ctrl Pts',(3.86308556320828,66.7940167052205,-20.9578499606675));
#24855=CARTESIAN_POINT('Ctrl Pts',(3.41103432597997,66.5244670539494,-21.8024606531298));
#24856=CARTESIAN_POINT('Ctrl Pts',(2.69285272661507,65.9264475450032,-23.5490026297785));
#24857=CARTESIAN_POINT('Ctrl Pts',(2.42604000771721,65.5973478982984,-24.4523631079317));
#24858=CARTESIAN_POINT('Ctrl Pts',(2.07963484569203,64.8987933787199,-26.2502710623803));
#24859=CARTESIAN_POINT('Ctrl Pts',(2.,64.5293013793053,-27.1447959433577));
#24860=CARTESIAN_POINT('Ctrl Pts',(2.,63.3502542343366,-29.846332338228));
#24861=CARTESIAN_POINT('Ctrl Pts',(2.38368127295869,62.4029020453759,-31.7791199130009));
#24862=CARTESIAN_POINT('Ctrl Pts',(3.90370579200787,60.4779252834904,-35.3051723987867));
#24863=CARTESIAN_POINT('Ctrl Pts',(5.03827663924619,59.503053899969,-36.9007032860843));
#24864=CARTESIAN_POINT('Ctrl Pts',(7.54764440420928,57.9574883058695,-39.2770767611709));
#24865=CARTESIAN_POINT('Ctrl Pts',(9.04077336951332,57.2551849551873,-40.2808837812864));
#24866=CARTESIAN_POINT('Ctrl Pts',(11.54482569449,56.5177517111439,-41.3027868899282));
#24867=CARTESIAN_POINT('Ctrl Pts',(12.4232339913984,56.3233853470359,-41.5658925850891));
#24868=CARTESIAN_POINT('Ctrl Pts',(14.2079498821129,56.064391561522,-41.9145698091276));
#24869=CARTESIAN_POINT('Ctrl Pts',(15.1143193052168,56.,-42.));
#24870=CARTESIAN_POINT('Ctrl Pts',(16.8856806947832,56.,-42.));
#24871=CARTESIAN_POINT('Ctrl Pts',(17.7920501178871,56.064391561522,-41.9145698091276));
#24872=CARTESIAN_POINT('Ctrl Pts',(19.5767660086016,56.3233853470359,-41.5658925850891));
#24873=CARTESIAN_POINT('Ctrl Pts',(20.45517430551,56.5177517111439,-41.3027868899282));
#24874=CARTESIAN_POINT('Ctrl Pts',(22.9592266304867,57.2551849551873,-40.2808837812864));
#24875=CARTESIAN_POINT('Ctrl Pts',(24.4523555957907,57.9574883058695,-39.2770767611709));
#24876=CARTESIAN_POINT('Ctrl Pts',(26.9617233607538,59.503053899969,-36.9007032860843));
#24877=CARTESIAN_POINT('Ctrl Pts',(28.0962942079921,60.4779252834904,-35.3051723987867));
#24878=CARTESIAN_POINT('Ctrl Pts',(29.6163187270413,62.4029020453759,-31.7791199130009));
#24879=CARTESIAN_POINT('Ctrl Pts',(30.,63.3502542343366,-29.846332338228));
#24880=CARTESIAN_POINT('Ctrl Pts',(30.,64.5293013793053,-27.1447959433577));
#24881=CARTESIAN_POINT('Ctrl Pts',(29.920365154308,64.8987933787199,-26.2502710623803));
#24882=CARTESIAN_POINT('Ctrl Pts',(29.5739599922828,65.5973478982984,-24.4523631079317));
#24883=CARTESIAN_POINT('Ctrl Pts',(29.3071472733849,65.9264475450032,-23.5490026297785));
#24884=CARTESIAN_POINT('Ctrl Pts',(28.58896567402,66.5244670539494,-21.8024606531298));
#24885=CARTESIAN_POINT('Ctrl Pts',(28.1369144367917,66.7940167052205,-20.9578499606675));
#24886=CARTESIAN_POINT('Ctrl Pts',(27.0781460846673,67.2665458430878,-19.3877268629585));
#24887=CARTESIAN_POINT('Ctrl Pts',(26.4713471796517,67.4697026576732,-18.662322985451));
#24888=CARTESIAN_POINT('Ctrl Pts',(24.5914812959786,67.9622849181329,-16.8132432389867));
#24889=CARTESIAN_POINT('Ctrl Pts',(23.0345575614708,68.2077217953467,-15.7551700622329));
#24890=CARTESIAN_POINT('Ctrl Pts',(20.6913501377322,68.4198540566006,-14.7917039729986));
#24891=CARTESIAN_POINT('Ctrl Pts',(20.038348684242,68.4654352022338,-14.5778037237174));
#24892=CARTESIAN_POINT('Ctrl Pts',(19.3775697035565,68.5,-14.4135353053998));
#24893=CARTESIAN_POINT('Origin',(16.,50.,-28.));
#24894=CARTESIAN_POINT('Origin',(16.,70.,-28.));
#24895=CARTESIAN_POINT('',(7.4,58.,-28.));
#24896=CARTESIAN_POINT('',(7.4,70.,-28.));
#24897=CARTESIAN_POINT('Origin',(16.,58.,-28.));
#24898=CARTESIAN_POINT('Origin',(16.,58.,-28.));
#24899=CARTESIAN_POINT('Origin',(0.4,-31.,-53.6935750346352));
#24900=CARTESIAN_POINT('',(35.5,-31.,-49.1935750346352));
#24901=CARTESIAN_POINT('',(0.4,-31.,-49.1935750346352));
#24902=CARTESIAN_POINT('Origin',(35.5,-31.,-53.6935750346352));
#24903=CARTESIAN_POINT('Origin',(0.4,62.,0.));
#24904=CARTESIAN_POINT('',(35.5,62.,4.5));
#24905=CARTESIAN_POINT('',(0.4,62.,4.5));
#24906=CARTESIAN_POINT('Origin',(35.5,62.,0.));
#24907=CARTESIAN_POINT('Origin',(0.4,31.,53.6935750346352));
#24908=CARTESIAN_POINT('',(35.5,31.,58.1935750346352));
#24909=CARTESIAN_POINT('',(0.4,31.,58.1935750346352));
#24910=CARTESIAN_POINT('Origin',(35.5,31.,53.6935750346352));
#24911=CARTESIAN_POINT('Origin',(0.4,-31.,53.6935750346352));
#24912=CARTESIAN_POINT('',(35.5,-31.,58.1935750346352));
#24913=CARTESIAN_POINT('',(0.4,-31.,58.1935750346352));
#24914=CARTESIAN_POINT('Origin',(35.5,-31.,53.6935750346352));
#24915=CARTESIAN_POINT('Origin',(0.4,-62.,7.59281015471359E-15));
#24916=CARTESIAN_POINT('',(35.5,-62.,4.50000000000001));
#24917=CARTESIAN_POINT('',(0.4,-62.,4.50000000000001));
#24918=CARTESIAN_POINT('Origin',(35.5,-62.,7.59281015471359E-15));
#24919=CARTESIAN_POINT('Origin',(0.4,31.,-53.6935750346352));
#24920=CARTESIAN_POINT('',(35.5,31.,-49.1935750346352));
#24921=CARTESIAN_POINT('',(0.4,31.,-49.1935750346352));
#24922=CARTESIAN_POINT('Origin',(35.5,31.,-53.6935750346352));
#24923=CARTESIAN_POINT('Origin',(10.25,0.,0.));
#24924=CARTESIAN_POINT('',(20.,-8.05,-9.85840673313619E-16));
#24925=CARTESIAN_POINT('Origin',(20.,0.,0.));
#24926=CARTESIAN_POINT('',(10.25,-8.05,-9.85840673313619E-16));
#24927=CARTESIAN_POINT('Origin',(35.,0.,0.));
#24928=CARTESIAN_POINT('',(35.5,-69.,-8.45006291411674E-15));
#24929=CARTESIAN_POINT('Origin',(35.5,0.,0.));
#24930=CARTESIAN_POINT('',(35.,-69.5,-8.51129525407411E-15));
#24931=CARTESIAN_POINT('Origin',(35.5,50.,0.));
#24932=CARTESIAN_POINT('',(35.5,-50.,-6.12323399573677E-15));
#24933=CARTESIAN_POINT('Origin',(35.5,0.,0.));
#24934=CARTESIAN_POINT('Origin',(30.75,0.,0.));
#24935=CARTESIAN_POINT('',(26.,-45.,-5.51091059616309E-15));
#24936=CARTESIAN_POINT('',(30.75,-47.5,-5.81707229594993E-15));
#24937=CARTESIAN_POINT('Origin',(26.,0.,0.));
#24938=CARTESIAN_POINT('Origin',(23.,0.,0.));
#24939=CARTESIAN_POINT('',(20.,-35.,-4.28626379701574E-15));
#24940=CARTESIAN_POINT('',(23.,-40.,-4.89858719658941E-15));
#24941=CARTESIAN_POINT('Origin',(20.,0.,0.));
#24942=CARTESIAN_POINT('Origin',(20.,8.05,0.));
#24943=CARTESIAN_POINT('',(0.,0.,0.));
#24944=CARTESIAN_POINT('Origin',(-0.6,-31.,-53.6935750346352));
#24945=CARTESIAN_POINT('',(-0.5,-31.,-49.1935750346352));
#24946=CARTESIAN_POINT('Origin',(-0.5,-31.,-53.6935750346352));
#24947=CARTESIAN_POINT('',(0.5,-31.,-49.1935750346352));
#24948=CARTESIAN_POINT('',(-0.6,-31.,-49.1935750346352));
#24949=CARTESIAN_POINT('Origin',(0.5,-31.,-53.6935750346352));
#24950=CARTESIAN_POINT('Origin',(-0.6,62.,0.));
#24951=CARTESIAN_POINT('',(-0.5,62.,4.5));
#24952=CARTESIAN_POINT('Origin',(-0.5,62.,0.));
#24953=CARTESIAN_POINT('',(0.5,62.,4.5));
#24954=CARTESIAN_POINT('',(-0.6,62.,4.5));
#24955=CARTESIAN_POINT('Origin',(0.5,62.,0.));
#24956=CARTESIAN_POINT('Origin',(-0.6,31.,53.6935750346352));
#24957=CARTESIAN_POINT('',(-0.5,31.,58.1935750346352));
#24958=CARTESIAN_POINT('Origin',(-0.5,31.,53.6935750346352));
#24959=CARTESIAN_POINT('',(0.5,31.,58.1935750346352));
#24960=CARTESIAN_POINT('',(-0.6,31.,58.1935750346352));
#24961=CARTESIAN_POINT('Origin',(0.5,31.,53.6935750346352));
#24962=CARTESIAN_POINT('Origin',(-0.6,-31.,53.6935750346352));
#24963=CARTESIAN_POINT('',(-0.5,-31.,58.1935750346352));
#24964=CARTESIAN_POINT('Origin',(-0.5,-31.,53.6935750346352));
#24965=CARTESIAN_POINT('',(0.5,-31.,58.1935750346352));
#24966=CARTESIAN_POINT('',(-0.6,-31.,58.1935750346352));
#24967=CARTESIAN_POINT('Origin',(0.5,-31.,53.6935750346352));
#24968=CARTESIAN_POINT('Origin',(-0.6,-62.,7.59281015471359E-15));
#24969=CARTESIAN_POINT('',(-0.5,-62.,4.50000000000001));
#24970=CARTESIAN_POINT('Origin',(-0.5,-62.,7.59281015471359E-15));
#24971=CARTESIAN_POINT('',(0.5,-62.,4.50000000000001));
#24972=CARTESIAN_POINT('',(-0.6,-62.,4.50000000000001));
#24973=CARTESIAN_POINT('Origin',(0.5,-62.,7.59281015471359E-15));
#24974=CARTESIAN_POINT('Origin',(-0.6,31.,-53.6935750346352));
#24975=CARTESIAN_POINT('',(-0.5,31.,-49.1935750346352));
#24976=CARTESIAN_POINT('Origin',(-0.5,31.,-53.6935750346352));
#24977=CARTESIAN_POINT('',(0.5,31.,-49.1935750346352));
#24978=CARTESIAN_POINT('',(-0.6,31.,-49.1935750346352));
#24979=CARTESIAN_POINT('Origin',(0.5,31.,-53.6935750346352));
#24980=CARTESIAN_POINT('Origin',(0.,0.,0.));
#24981=CARTESIAN_POINT('',(0.5,-8.5,-1.04094977927525E-15));
#24982=CARTESIAN_POINT('Origin',(0.5,0.,0.));
#24983=CARTESIAN_POINT('',(-0.5,-8.5,-1.04094977927525E-15));
#24984=CARTESIAN_POINT('',(0.,-8.5,-1.04094977927525E-15));
#24985=CARTESIAN_POINT('Origin',(-0.5,0.,0.));
#24986=CARTESIAN_POINT('Origin',(-0.5,70.,0.));
#24987=CARTESIAN_POINT('',(-0.5,-70.,-8.57252759403147E-15));
#24988=CARTESIAN_POINT('Origin',(-0.5,0.,0.));
#24989=CARTESIAN_POINT('Origin',(0.,0.,0.));
#24990=CARTESIAN_POINT('',(0.5,-70.,-8.57252759403147E-15));
#24991=CARTESIAN_POINT('Origin',(0.5,0.,0.));
#24992=CARTESIAN_POINT('',(0.,-70.,-8.57252759403147E-15));
#24993=CARTESIAN_POINT('Origin',(0.5,8.5,0.));
#24994=CARTESIAN_POINT('',(0.,0.,0.));
#24995=CARTESIAN_POINT('Origin',(35.4,-31.,-53.6935750346352));
#24996=CARTESIAN_POINT('',(35.5,-31.,-49.1935750346352));
#24997=CARTESIAN_POINT('Origin',(35.5,-31.,-53.6935750346352));
#24998=CARTESIAN_POINT('',(38.5,-31.,-49.1935750346352));
#24999=CARTESIAN_POINT('',(35.4,-31.,-49.1935750346352));
#25000=CARTESIAN_POINT('Origin',(38.5,-31.,-53.6935750346352));
#25001=CARTESIAN_POINT('Origin',(35.4,62.,0.));
#25002=CARTESIAN_POINT('',(35.5,62.,4.5));
#25003=CARTESIAN_POINT('Origin',(35.5,62.,0.));
#25004=CARTESIAN_POINT('',(38.5,62.,4.5));
#25005=CARTESIAN_POINT('',(35.4,62.,4.5));
#25006=CARTESIAN_POINT('Origin',(38.5,62.,0.));
#25007=CARTESIAN_POINT('Origin',(35.4,31.,53.6935750346352));
#25008=CARTESIAN_POINT('',(35.5,31.,58.1935750346352));
#25009=CARTESIAN_POINT('Origin',(35.5,31.,53.6935750346352));
#25010=CARTESIAN_POINT('',(38.5,31.,58.1935750346352));
#25011=CARTESIAN_POINT('',(35.4,31.,58.1935750346352));
#25012=CARTESIAN_POINT('Origin',(38.5,31.,53.6935750346352));
#25013=CARTESIAN_POINT('Origin',(35.4,-31.,53.6935750346352));
#25014=CARTESIAN_POINT('',(35.5,-31.,58.1935750346352));
#25015=CARTESIAN_POINT('Origin',(35.5,-31.,53.6935750346352));
#25016=CARTESIAN_POINT('',(38.5,-31.,58.1935750346352));
#25017=CARTESIAN_POINT('',(35.4,-31.,58.1935750346352));
#25018=CARTESIAN_POINT('Origin',(38.5,-31.,53.6935750346352));
#25019=CARTESIAN_POINT('Origin',(35.4,-62.,7.59281015471359E-15));
#25020=CARTESIAN_POINT('',(35.5,-62.,4.50000000000001));
#25021=CARTESIAN_POINT('Origin',(35.5,-62.,7.59281015471359E-15));
#25022=CARTESIAN_POINT('',(38.5,-62.,4.50000000000001));
#25023=CARTESIAN_POINT('',(35.4,-62.,4.50000000000001));
#25024=CARTESIAN_POINT('Origin',(38.5,-62.,7.59281015471359E-15));
#25025=CARTESIAN_POINT('Origin',(35.4,31.,-53.6935750346352));
#25026=CARTESIAN_POINT('',(35.5,31.,-49.1935750346352));
#25027=CARTESIAN_POINT('Origin',(35.5,31.,-53.6935750346352));
#25028=CARTESIAN_POINT('',(38.5,31.,-49.1935750346352));
#25029=CARTESIAN_POINT('',(35.4,31.,-49.1935750346352));
#25030=CARTESIAN_POINT('Origin',(38.5,31.,-53.6935750346352));
#25031=CARTESIAN_POINT('Origin',(37.,0.,0.));
#25032=CARTESIAN_POINT('',(38.25,-5.2,-6.36816335556624E-16));
#25033=CARTESIAN_POINT('Origin',(38.25,0.,0.));
#25034=CARTESIAN_POINT('',(35.75,-5.2,-6.36816335556624E-16));
#25035=CARTESIAN_POINT('',(37.,-5.2,-6.36816335556624E-16));
#25036=CARTESIAN_POINT('Origin',(35.75,0.,0.));
#25037=CARTESIAN_POINT('Origin',(35.75,44.,0.));
#25038=CARTESIAN_POINT('',(35.75,-44.,-5.38844591624835E-15));
#25039=CARTESIAN_POINT('Origin',(35.75,0.,0.));
#25040=CARTESIAN_POINT('Origin',(35.625,0.,0.));
#25041=CARTESIAN_POINT('',(35.5,-46.,-5.63337527607782E-15));
#25042=CARTESIAN_POINT('',(35.625,-45.,-5.51091059616309E-15));
#25043=CARTESIAN_POINT('Origin',(35.5,0.,0.));
#25044=CARTESIAN_POINT('Origin',(35.5,70.,0.));
#25045=CARTESIAN_POINT('',(35.5,-70.,-8.57252759403147E-15));
#25046=CARTESIAN_POINT('Origin',(35.5,0.,0.));
#25047=CARTESIAN_POINT('Origin',(37.,0.,0.));
#25048=CARTESIAN_POINT('',(38.5,-70.,-8.57252759403147E-15));
#25049=CARTESIAN_POINT('Origin',(38.5,0.,0.));
#25050=CARTESIAN_POINT('',(37.,-70.,-8.57252759403147E-15));
#25051=CARTESIAN_POINT('Origin',(38.5,46.,0.));
#25052=CARTESIAN_POINT('',(38.5,-46.,-5.63337527607782E-15));
#25053=CARTESIAN_POINT('Origin',(38.5,0.,0.));
#25054=CARTESIAN_POINT('Origin',(38.375,0.,0.));
#25055=CARTESIAN_POINT('',(38.25,-44.,-5.38844591624835E-15));
#25056=CARTESIAN_POINT('',(38.375,-45.,-5.51091059616309E-15));
#25057=CARTESIAN_POINT('Origin',(38.25,0.,0.));
#25058=CARTESIAN_POINT('Origin',(38.25,5.2,0.));
#25059=CARTESIAN_POINT('',(0.,0.,0.));
#25060=CARTESIAN_POINT('Origin',(30.0813172798365,0.,-8.92848176705185E-16));
#25061=CARTESIAN_POINT('',(30.1626345596729,29.1626345596729,-3.57139270682074E-15));
#25062=CARTESIAN_POINT('',(30.1626345596729,-29.1626345596729,-3.57139270682074E-15));
#25063=CARTESIAN_POINT('Origin',(30.1626345596729,0.,-1.78569635341037E-15));
#25064=CARTESIAN_POINT('Origin',(30.1626345596729,0.,-1.78569635341037E-15));
#25065=CARTESIAN_POINT('',(30.,28.77,3.52330884114693E-15));
#25066=CARTESIAN_POINT('',(30.0813172798365,28.9663172798365,3.54735077398384E-15));
#25067=CARTESIAN_POINT('Origin',(30.,0.,0.));
#25068=CARTESIAN_POINT('Origin',(30.,29.,0.));
#25069=CARTESIAN_POINT('',(30.,-5.1,-6.2456986756515E-16));
#25070=CARTESIAN_POINT('Origin',(30.,0.,0.));
#25071=CARTESIAN_POINT('Origin',(30.5,0.,0.));
#25072=CARTESIAN_POINT('',(31.,-30.,-3.67394039744206E-15));
#25073=CARTESIAN_POINT('Origin',(31.,0.,0.));
#25074=CARTESIAN_POINT('',(30.5,-29.5,-3.61270805748469E-15));
#25075=CARTESIAN_POINT('Origin',(32.875,0.,0.));
#25076=CARTESIAN_POINT('',(35.75,-5.1,-6.2456986756515E-16));
#25077=CARTESIAN_POINT('Origin',(35.75,0.,0.));
#25078=CARTESIAN_POINT('',(32.875,-5.1,-6.2456986756515E-16));
#25079=CARTESIAN_POINT('Origin',(33.375,0.,0.));
#25080=CARTESIAN_POINT('',(35.75,-30.,-3.67394039744206E-15));
#25081=CARTESIAN_POINT('Origin',(35.75,0.,0.));
#25082=CARTESIAN_POINT('',(33.375,-30.,-3.67394039744206E-15));
#25083=CARTESIAN_POINT('Origin',(35.75,5.1,0.));
#25084=CARTESIAN_POINT('',(0.,0.,0.));
#25085=CARTESIAN_POINT('Origin',(43.9636338069081,0.,-5.57771420911391E-16));
#25086=CARTESIAN_POINT('',(44.,17.77,-2.17619736208484E-15));
#25087=CARTESIAN_POINT('Origin',(44.,0.,0.));
#25088=CARTESIAN_POINT('',(43.9272676138161,18.2181971585516,2.23108568364556E-15));
#25089=CARTESIAN_POINT('',(43.9636338069081,17.9940985792758,2.2036415228652E-15));
#25090=CARTESIAN_POINT('',(43.9272676138161,-18.2181971585516,-2.23108568364556E-15));
#25091=CARTESIAN_POINT('Origin',(43.9272676138161,0.,-1.11554284182278E-15));
#25092=CARTESIAN_POINT('Origin',(43.9272676138161,0.,-1.11554284182278E-15));
#25093=CARTESIAN_POINT('Origin',(44.,5.1,0.));
#25094=CARTESIAN_POINT('',(44.,5.33,6.52736743945539E-16));
#25095=CARTESIAN_POINT('Origin',(44.,0.,0.));
#25096=CARTESIAN_POINT('Origin',(42.,0.,0.));
#25097=CARTESIAN_POINT('',(40.,-30.,-3.67394039744206E-15));
#25098=CARTESIAN_POINT('',(42.,-24.,-2.93915231795365E-15));
#25099=CARTESIAN_POINT('Origin',(40.,0.,0.));
#25100=CARTESIAN_POINT('Origin',(38.365,0.,0.));
#25101=CARTESIAN_POINT('',(38.25,5.33,-6.52736743945539E-16));
#25102=CARTESIAN_POINT('Origin',(38.25,0.,0.));
#25103=CARTESIAN_POINT('',(38.48,5.1,6.2456986756515E-16));
#25104=CARTESIAN_POINT('',(38.365,5.215,-6.38653305755345E-16));
#25105=CARTESIAN_POINT('',(38.48,-5.1,-6.2456986756515E-16));
#25106=CARTESIAN_POINT('Origin',(38.48,0.,0.));
#25107=CARTESIAN_POINT('Origin',(38.48,0.,0.));
#25108=CARTESIAN_POINT('Origin',(41.125,0.,0.));
#25109=CARTESIAN_POINT('',(43.77,5.1,-6.2456986756515E-16));
#25110=CARTESIAN_POINT('',(43.77,-5.1,-6.2456986756515E-16));
#25111=CARTESIAN_POINT('Origin',(43.77,0.,0.));
#25112=CARTESIAN_POINT('Origin',(43.77,0.,0.));
#25113=CARTESIAN_POINT('',(41.125,-5.1,-6.2456986756515E-16));
#25114=CARTESIAN_POINT('Origin',(38.25,30.,0.));
#25115=CARTESIAN_POINT('',(38.25,-30.,-3.67394039744206E-15));
#25116=CARTESIAN_POINT('Origin',(38.25,0.,0.));
#25117=CARTESIAN_POINT('Origin',(43.885,0.,0.));
#25118=CARTESIAN_POINT('',(43.885,5.215,-6.38653305755345E-16));
#25119=CARTESIAN_POINT('Origin',(39.125,0.,0.));
#25120=CARTESIAN_POINT('',(39.125,-30.,-3.67394039744206E-15));
#25121=CARTESIAN_POINT('',(0.,0.,0.));
#25122=CARTESIAN_POINT('Origin',(-41.25,0.,0.));
#25123=CARTESIAN_POINT('',(-52.0911584740964,-4.92503359593706,0.000126434235863393));
#25124=CARTESIAN_POINT('',(-52.3088415259036,-4.92498877504697,8.594588268108E-5));
#25125=CARTESIAN_POINT('',(-41.25,-4.925,-6.03138548580071E-16));
#25126=CARTESIAN_POINT('',(-52.575,2.16848938207169,4.42202992386415));
#25127=CARTESIAN_POINT('Ctrl Pts',(-52.0911584740964,-4.92503359593706,
0.000126434235863393));
#25128=CARTESIAN_POINT('Ctrl Pts',(-52.0997969204186,-4.92521675924443,
0.178328848272776));
#25129=CARTESIAN_POINT('Ctrl Pts',(-52.1084353667407,-4.91573151990345,
0.356511816443558));
#25130=CARTESIAN_POINT('Ctrl Pts',(-52.1170738130628,-4.89642931932951,
0.533624833881526));
#25131=CARTESIAN_POINT('Ctrl Pts',(-52.1567101460612,-4.80786380407155,
1.3462837630126));
#25132=CARTESIAN_POINT('Ctrl Pts',(-52.1963464790595,-4.5126210099822,2.13641693282812));
#25133=CARTESIAN_POINT('Ctrl Pts',(-52.2359828120578,-4.04657310803694,
2.80802695734203));
#25134=CARTESIAN_POINT('Ctrl Pts',(-52.2756191450561,-3.58052520609168,
3.47963698185595));
#25135=CARTESIAN_POINT('Ctrl Pts',(-52.3152554780544,-2.94367219629051,
4.03272386106826));
#25136=CARTESIAN_POINT('Ctrl Pts',(-52.3548918110528,-2.21339245150104,
4.40007810178881));
#25137=CARTESIAN_POINT('Ctrl Pts',(-52.3945281440511,-1.48311270671156,
4.76743234250936));
#25138=CARTESIAN_POINT('Ctrl Pts',(-52.4341644770494,-0.659406226933773,
4.94905394473814));
#25139=CARTESIAN_POINT('Ctrl Pts',(-52.4738008100477,0.157646275526665,
4.92289359031672));
#25140=CARTESIAN_POINT('Ctrl Pts',(-52.5075338733652,0.853010395116791,
4.90062944968238));
#25141=CARTESIAN_POINT('Ctrl Pts',(-52.5412669366825,1.54355497078764,4.72786670979692));
#25142=CARTESIAN_POINT('Ctrl Pts',(-52.575,2.16858289183292,4.42210503781143));
#25143=CARTESIAN_POINT('',(-52.575,-2.16839587231069,4.42195480991676));
#25144=CARTESIAN_POINT('Origin',(-52.575,0.,0.));
#25145=CARTESIAN_POINT('Ctrl Pts',(-52.575,-2.16839587231068,4.42195480991676));
#25146=CARTESIAN_POINT('Ctrl Pts',(-52.5353636670017,-2.90256543874876,
4.06193976546849));
#25147=CARTESIAN_POINT('Ctrl Pts',(-52.4957273340034,-3.54497563996543,
3.51573282579364));
#25148=CARTESIAN_POINT('Ctrl Pts',(-52.456091001005,-4.01781939721874,2.84901257911266));
#25149=CARTESIAN_POINT('Ctrl Pts',(-52.4164546680067,-4.49066315447206,
2.18229233243166));
#25150=CARTESIAN_POINT('Ctrl Pts',(-52.3768183350084,-4.79394046776201,
1.39505877874451));
#25151=CARTESIAN_POINT('Ctrl Pts',(-52.3371820020101,-4.89076226499141,
0.583305000514948));
#25152=CARTESIAN_POINT('Ctrl Pts',(-52.3277351766413,-4.91383853217185,
0.389833616929986));
#25153=CARTESIAN_POINT('Ctrl Pts',(-52.3182883512724,-4.92518714038783,
0.194969367527474));
#25154=CARTESIAN_POINT('Ctrl Pts',(-52.3088415259036,-4.92498877504697,
8.594588268108E-5));
#25155=CARTESIAN_POINT('Origin',(-41.25,0.,0.));
#25156=CARTESIAN_POINT('',(-50.5911584740964,-4.92516278400206,-0.000113722891083023));
#25157=CARTESIAN_POINT('',(-50.8088415259036,-4.92521228692415,-0.000105349288354082));
#25158=CARTESIAN_POINT('',(-41.25,-4.925,-6.03138548580071E-16));
#25159=CARTESIAN_POINT('Ctrl Pts',(-50.5911584740964,-4.92516278400206,
-0.000113722891083023));
#25160=CARTESIAN_POINT('Ctrl Pts',(-50.6241609244387,-4.92448960067175,
0.680641940579653));
#25161=CARTESIAN_POINT('Ctrl Pts',(-50.657163374781,-4.78214557076829,1.36167034726095));
#25162=CARTESIAN_POINT('Ctrl Pts',(-50.6901658251233,-4.50788726697863,
1.98462275182099));
#25163=CARTESIAN_POINT('Ctrl Pts',(-50.7298021581216,-4.17849980199303,
2.73279595390601));
#25164=CARTESIAN_POINT('Ctrl Pts',(-50.7694384911199,-3.65883531069533,
3.39719862337027));
#25165=CARTESIAN_POINT('Ctrl Pts',(-50.8090748241183,-3.01203348417392,
3.89710525473833));
#25166=CARTESIAN_POINT('Ctrl Pts',(-50.8487111571166,-2.36523165765252,
4.39701188610637));
#25167=CARTESIAN_POINT('Ctrl Pts',(-50.8883474901149,-1.59129249590741,
4.73242247937822));
#25168=CARTESIAN_POINT('Ctrl Pts',(-50.9279838231132,-0.784250285390256,
4.8625843512811));
#25169=CARTESIAN_POINT('Ctrl Pts',(-50.9676201561115,0.0227919251269108,
4.99274622318398));
#25170=CARTESIAN_POINT('Ctrl Pts',(-51.0072564891099,0.862937184416126,
4.91765937371789));
#25171=CARTESIAN_POINT('Ctrl Pts',(-51.0468928221082,1.63410710728407,4.64644692538026));
#25172=CARTESIAN_POINT('Ctrl Pts',(-51.0865291551065,2.40527703015201,4.37523447704264));
#25173=CARTESIAN_POINT('Ctrl Pts',(-51.1261654881048,3.10747161659867,3.90789642983347));
#25174=CARTESIAN_POINT('Ctrl Pts',(-51.1658018211031,3.65537360881555,3.30121475710258));
#25175=CARTESIAN_POINT('Ctrl Pts',(-51.2054381541015,4.20327560103244,2.69453308437168));
#25176=CARTESIAN_POINT('Ctrl Pts',(-51.2450744870998,4.59688499901954,1.94850778611905));
#25177=CARTESIAN_POINT('Ctrl Pts',(-51.2847108200981,4.78837791632171,1.15378160772726));
#25178=CARTESIAN_POINT('Ctrl Pts',(-51.3243471530964,4.97987083362388,0.359055429335473));
#25179=CARTESIAN_POINT('Ctrl Pts',(-51.3639834860947,4.96924727024111,-0.484371629195479));
#25180=CARTESIAN_POINT('Ctrl Pts',(-51.4036198190931,4.75779799774183,-1.27402247672251));
#25181=CARTESIAN_POINT('Ctrl Pts',(-51.4432561520914,4.54634872524255,-2.06367332424954));
#25182=CARTESIAN_POINT('Ctrl Pts',(-51.4828924850897,4.13407374362675,-2.79954796077265));
#25183=CARTESIAN_POINT('Ctrl Pts',(-51.522528818088,3.57106482584788,-3.39223690197812));
#25184=CARTESIAN_POINT('Ctrl Pts',(-51.5621651510863,3.00805590806901,-3.98492584318359));
#25185=CARTESIAN_POINT('Ctrl Pts',(-51.6018014840847,2.29431305412705,-4.43442908907142));
#25186=CARTESIAN_POINT('Ctrl Pts',(-51.641437817083,1.51655664351954,-4.68613174316612));
#25187=CARTESIAN_POINT('Ctrl Pts',(-51.6810741500813,0.738800232912025,
-4.93783439726082));
#25188=CARTESIAN_POINT('Ctrl Pts',(-51.7207104830797,-0.102969734361041,
-4.99173645956238));
#25189=CARTESIAN_POINT('Ctrl Pts',(-51.760346816078,-0.906477464071566,
-4.84128849925518));
#25190=CARTESIAN_POINT('Ctrl Pts',(-51.7999831490763,-1.70998519378208,
-4.69084053894799));
#25191=CARTESIAN_POINT('Ctrl Pts',(-51.8396194820746,-2.47523068593005,
-4.33604255603204));
#25192=CARTESIAN_POINT('Ctrl Pts',(-51.8792558150729,-3.10923595356447,
-3.82000338107853));
#25193=CARTESIAN_POINT('Ctrl Pts',(-51.9188921480712,-3.74324122119889,
-3.30396420612501));
#25194=CARTESIAN_POINT('Ctrl Pts',(-51.9585284810696,-4.24600626431976,
-2.62668383913391));
#25195=CARTESIAN_POINT('Ctrl Pts',(-51.9981648140679,-4.55644466766691,
-1.87045131141505));
#25196=CARTESIAN_POINT('Ctrl Pts',(-52.0291627007441,-4.79922531155988,
-1.27903408328594));
#25197=CARTESIAN_POINT('Ctrl Pts',(-52.0601605874203,-4.92437633938499,
-0.639328628600892));
#25198=CARTESIAN_POINT('Ctrl Pts',(-52.0911584740964,-4.92503359593706,
0.000126434235863393));
#25199=CARTESIAN_POINT('Ctrl Pts',(-52.3088415259036,-4.92498877504697,
8.594588268108E-5));
#25200=CARTESIAN_POINT('Ctrl Pts',(-52.2786520182741,-4.92435485288396,
-0.622708941807593));
#25201=CARTESIAN_POINT('Ctrl Pts',(-52.2484625106446,-4.8057952323332,-1.24569962972635));
#25202=CARTESIAN_POINT('Ctrl Pts',(-52.2182730030151,-4.57520694571846,
-1.82405286031686));
#25203=CARTESIAN_POINT('Ctrl Pts',(-52.1786366700168,-4.27246354804726,
-2.58338294014709));
#25204=CARTESIAN_POINT('Ctrl Pts',(-52.1390003370185,-3.77661047153599,
-3.26576909703558));
#25205=CARTESIAN_POINT('Ctrl Pts',(-52.0993640040201,-3.14788146612183,
-3.78823038007532));
#25206=CARTESIAN_POINT('Ctrl Pts',(-52.0597276710218,-2.51915246070767,
-4.31069166311506));
#25207=CARTESIAN_POINT('Ctrl Pts',(-52.0200913380235,-1.75754752639063,
-4.67322807230605));
#25208=CARTESIAN_POINT('Ctrl Pts',(-51.9804550050252,-0.955608780981152,
-4.8318262860996));
#25209=CARTESIAN_POINT('Ctrl Pts',(-51.9408186720269,-0.153670035571674,
-4.99042449989316));
#25210=CARTESIAN_POINT('Ctrl Pts',(-51.9011823390286,0.688602520930237,
-4.94508451828928));
#25211=CARTESIAN_POINT('Ctrl Pts',(-51.8615460060302,1.4688752699207,-4.70129756843068));
#25212=CARTESIAN_POINT('Ctrl Pts',(-51.8219096730319,2.24914801891116,-4.45751061857207));
#25213=CARTESIAN_POINT('Ctrl Pts',(-51.7822733400336,2.96742096039018,-4.01527670045875));
#25214=CARTESIAN_POINT('Ctrl Pts',(-51.7426370070353,3.53642168058144,-3.42833645513739));
#25215=CARTESIAN_POINT('Ctrl Pts',(-51.7030006740369,4.10542240077269,-2.84139620981605));
#25216=CARTESIAN_POINT('Ctrl Pts',(-51.6633643410386,4.52515089967618,-2.10974963728667));
#25217=CARTESIAN_POINT('Ctrl Pts',(-51.6237280080403,4.7446106099284,-1.32228800957761));
#25218=CARTESIAN_POINT('Ctrl Pts',(-51.584091675042,4.96407032018062,-0.534826381868543));
#25219=CARTESIAN_POINT('Ctrl Pts',(-51.5444553420437,4.98326124178157,0.30845030102022));
#25220=CARTESIAN_POINT('Ctrl Pts',(-51.5048190090453,4.79985125332747,1.10508096343737));
#25221=CARTESIAN_POINT('Ctrl Pts',(-51.465182676047,4.61644126487337,1.90171162585452));
#25222=CARTESIAN_POINT('Ctrl Pts',(-51.4255463430487,4.23043036636422,2.65169626780005));
#25223=CARTESIAN_POINT('Ctrl Pts',(-51.3859100100504,3.68871942459624,3.26391221075199));
#25224=CARTESIAN_POINT('Ctrl Pts',(-51.3462736770521,3.14700848282826,3.87612815370392));
#25225=CARTESIAN_POINT('Ctrl Pts',(-51.3066373440538,2.44959749780146,4.35057539766226));
#25226=CARTESIAN_POINT('Ctrl Pts',(-51.2670010110554,1.68122241294815,4.6296076288689));
#25227=CARTESIAN_POINT('Ctrl Pts',(-51.2273646780571,0.912847328094825,
4.90863986007553));
#25228=CARTESIAN_POINT('Ctrl Pts',(-51.1877283450588,0.0735081434149867,
4.99225707853046));
#25229=CARTESIAN_POINT('Ctrl Pts',(-51.1480920120605,-0.734814643229353,
4.87029999855603));
#25230=CARTESIAN_POINT('Ctrl Pts',(-51.1084556790621,-1.54313742987369,
4.74834291858159));
#25231=CARTESIAN_POINT('Ctrl Pts',(-51.0688193460638,-2.32044381848253,
4.42081154017779));
#25232=CARTESIAN_POINT('Ctrl Pts',(-51.0291830130655,-2.97229042737678,
3.92750107267045));
#25233=CARTESIAN_POINT('Ctrl Pts',(-50.9895466800672,-3.62413703627103,
3.43419060516311));
#25234=CARTESIAN_POINT('Ctrl Pts',(-50.9499103470689,-4.1505238654507,2.77510104855222));
#25235=CARTESIAN_POINT('Ctrl Pts',(-50.9102740140705,-4.48749444095599,
2.03031243184926));
#25236=CARTESIAN_POINT('Ctrl Pts',(-50.8764631846815,-4.77493916087995,
1.39498824958286));
#25237=CARTESIAN_POINT('Ctrl Pts',(-50.8426523552926,-4.92455445259501,
0.697304833505213));
#25238=CARTESIAN_POINT('Ctrl Pts',(-50.8088415259036,-4.92521228692415,
-0.000105349288354082));
#25239=CARTESIAN_POINT('Origin',(-41.25,0.,0.));
#25240=CARTESIAN_POINT('',(-49.0911584740964,-4.92460059430091,3.93170950760413E-5));
#25241=CARTESIAN_POINT('',(-49.3088415259036,-4.92458892021405,2.43377720096698E-5));
#25242=CARTESIAN_POINT('',(-41.25,-4.925,-6.03138548580071E-16));
#25243=CARTESIAN_POINT('Ctrl Pts',(-49.0911584740964,-4.92460059430091,
3.93170950760413E-5));
#25244=CARTESIAN_POINT('Ctrl Pts',(-49.1088885954605,-4.92470301078537,
0.365886075098635));
#25245=CARTESIAN_POINT('Ctrl Pts',(-49.1266187168247,-4.88447438334452,
0.731710656523951));
#25246=CARTESIAN_POINT('Ctrl Pts',(-49.1443488381888,-4.80367404526498,
1.08834311923078));
#25247=CARTESIAN_POINT('Ctrl Pts',(-49.1839851711871,-4.62304194237499,
1.88560799743165));
#25248=CARTESIAN_POINT('Ctrl Pts',(-49.2236215041854,-4.23964771199399,
2.63693412870344));
#25249=CARTESIAN_POINT('Ctrl Pts',(-49.2632578371838,-3.70007408910792,
3.25103472965791));
#25250=CARTESIAN_POINT('Ctrl Pts',(-49.3028941701821,-3.16050046622184,
3.86513533061238));
#25251=CARTESIAN_POINT('Ctrl Pts',(-49.3425305031804,-2.46474745083068,
4.34201040124952));
#25252=CARTESIAN_POINT('Ctrl Pts',(-49.3821668361787,-1.69734964404053,
4.62371920256889));
#25253=CARTESIAN_POINT('Ctrl Pts',(-49.421803169177,-0.929951837250387,
4.90542800388826));
#25254=CARTESIAN_POINT('Ctrl Pts',(-49.4614395021754,-0.0909092390612466,
4.99197053588986));
#25255=CARTESIAN_POINT('Ctrl Pts',(-49.5010758351737,0.717833739536359,
4.87283180509178));
#25256=CARTESIAN_POINT('Ctrl Pts',(-49.540712168172,1.52657671813397,4.7536930742937));
#25257=CARTESIAN_POINT('Ctrl Pts',(-49.5803485011703,2.30502007714005,4.42887308069593));
#25258=CARTESIAN_POINT('Ctrl Pts',(-49.6199848341686,2.9585822662321,3.93783773818377));
#25259=CARTESIAN_POINT('Ctrl Pts',(-49.659621167167,3.61214445532415,3.44680239567161));
#25260=CARTESIAN_POINT('Ctrl Pts',(-49.6992575001653,4.14082547450218,2.78955170424504));
#25261=CARTESIAN_POINT('Ctrl Pts',(-49.7388938331636,4.48039011661659,2.04594219890398));
#25262=CARTESIAN_POINT('Ctrl Pts',(-49.7785301661619,4.81995475873101,1.30233269356293));
#25263=CARTESIAN_POINT('Ctrl Pts',(-49.8181664991602,4.97040302378181,0.472364374307389));
#25264=CARTESIAN_POINT('Ctrl Pts',(-49.8578028321585,4.91345531571728,-0.343120880710482));
#25265=CARTESIAN_POINT('Ctrl Pts',(-49.8974391651569,4.85650760765276,-1.15860613572836));
#25266=CARTESIAN_POINT('Ctrl Pts',(-49.9370754981552,4.59216392647291,-1.95960832650857));
#25267=CARTESIAN_POINT('Ctrl Pts',(-49.9767118311536,4.1525422611034,-2.64880498490713));
#25268=CARTESIAN_POINT('Ctrl Pts',(-50.0163481641519,3.71292059573389,-3.33800164330569));
#25269=CARTESIAN_POINT('Ctrl Pts',(-50.0559844971501,3.09802094617472,-3.91539276932261));
#25270=CARTESIAN_POINT('Ctrl Pts',(-50.0956208301485,2.38255415872639,-4.31082483512157));
#25271=CARTESIAN_POINT('Ctrl Pts',(-50.1352571631468,1.66708737127806,-4.70625690092052));
#25272=CARTESIAN_POINT('Ctrl Pts',(-50.1748934961451,0.851053445940566,
-4.91972990650151));
#25273=CARTESIAN_POINT('Ctrl Pts',(-50.2145298291434,0.0336012197881862,
-4.92530669464102));
#25274=CARTESIAN_POINT('Ctrl Pts',(-50.2541661621418,-0.7838510063642,-4.93088348278053));
#25275=CARTESIAN_POINT('Ctrl Pts',(-50.2938024951401,-1.60272153333147,
-4.72856405347856));
#25276=CARTESIAN_POINT('Ctrl Pts',(-50.3334388281384,-2.32351687445336,
-4.34293039463065));
#25277=CARTESIAN_POINT('Ctrl Pts',(-50.3730751611367,-3.04431221557524,
-3.95729673578274));
#25278=CARTESIAN_POINT('Ctrl Pts',(-50.4127114941351,-3.66703237085174,
-3.38834884738889));
#25279=CARTESIAN_POINT('Ctrl Pts',(-50.4523478271334,-4.11601629568715,
-2.70521439663872));
#25280=CARTESIAN_POINT('Ctrl Pts',(-50.4919841601317,-4.56500022052256,
-2.02207994588855));
#25281=CARTESIAN_POINT('Ctrl Pts',(-50.53162049313,-4.84024791491689,-1.22475893278206));
#25282=CARTESIAN_POINT('Ctrl Pts',(-50.5712568261283,-4.90831654277731,
-0.410126558875938));
#25283=CARTESIAN_POINT('Ctrl Pts',(-50.5778907087843,-4.91970910247252,
-0.27378257426661));
#25284=CARTESIAN_POINT('Ctrl Pts',(-50.5845245914404,-4.92529810180946,
-0.136953658776159));
#25285=CARTESIAN_POINT('Ctrl Pts',(-50.5911584740964,-4.92516278400206,
-0.000113722891083023));
#25286=CARTESIAN_POINT('Ctrl Pts',(-50.8088415259036,-4.92521228692415,
-0.000105349288354082));
#25287=CARTESIAN_POINT('Ctrl Pts',(-50.8030160222942,-4.92532562978879,
-0.120267013775082));
#25288=CARTESIAN_POINT('Ctrl Pts',(-50.7971905186849,-4.92101698471771,
-0.240420566990935));
#25289=CARTESIAN_POINT('Ctrl Pts',(-50.7913650150756,-4.91222943350402,
-0.36024565322302));
#25290=CARTESIAN_POINT('Ctrl Pts',(-50.7517286820772,-4.85243952871584,
-1.17552744479729));
#25291=CARTESIAN_POINT('Ctrl Pts',(-50.7120923490789,-4.58530539730858,
-1.97560335115078));
#25292=CARTESIAN_POINT('Ctrl Pts',(-50.6724560160806,-4.14328406711282,
-2.66326343083852));
#25293=CARTESIAN_POINT('Ctrl Pts',(-50.6328196830823,-3.70126273691706,
-3.35092351052627));
#25294=CARTESIAN_POINT('Ctrl Pts',(-50.593183350084,-3.08435420793282,-3.92616776354825));
#25295=CARTESIAN_POINT('Ctrl Pts',(-50.5535470170856,-2.36751340869681,
-4.31910351789033));
#25296=CARTESIAN_POINT('Ctrl Pts',(-50.5139106840873,-1.65067260946082,
-4.71203927223239));
#25297=CARTESIAN_POINT('Ctrl Pts',(-50.474274351089,-0.833899539973056,
-4.92266652789455));
#25298=CARTESIAN_POINT('Ctrl Pts',(-50.4346380180907,-0.0164328431554427,
-4.92539388428815));
#25299=CARTESIAN_POINT('Ctrl Pts',(-50.3950016850924,0.801033853662174,
-4.92812124068174));
#25300=CARTESIAN_POINT('Ctrl Pts',(-50.355365352094,1.61919417780964,-4.72294869780679));
#25301=CARTESIAN_POINT('Ctrl Pts',(-50.3157290190957,2.33864093248448,-4.33480490165446));
#25302=CARTESIAN_POINT('Ctrl Pts',(-50.2760926860974,3.05808768715931,-3.94666110550212));
#25303=CARTESIAN_POINT('Ctrl Pts',(-50.2364563530991,3.67882087236151,-3.3755460560724));
#25304=CARTESIAN_POINT('Ctrl Pts',(-50.1968200201008,4.1254208623028,-2.6908507312628));
#25305=CARTESIAN_POINT('Ctrl Pts',(-50.1571836871024,4.57202085224408,-2.00615540645321));
#25306=CARTESIAN_POINT('Ctrl Pts',(-50.1175473541041,4.84448764692445,-1.20787980626376));
#25307=CARTESIAN_POINT('Ctrl Pts',(-50.0779110211058,4.90971629190624,-0.393015116260266));
#25308=CARTESIAN_POINT('Ctrl Pts',(-50.0382746881075,4.97494493688802,0.421849573743228));
#25309=CARTESIAN_POINT('Ctrl Pts',(-49.9986383551092,4.83293543217122,1.25330335356076));
#25310=CARTESIAN_POINT('Ctrl Pts',(-49.9590020221108,4.50094205708306,2.00032386056488));
#25311=CARTESIAN_POINT('Ctrl Pts',(-49.9193656891125,4.1689486819949,2.747344367569));
#25312=CARTESIAN_POINT('Ctrl Pts',(-49.8797293561142,3.64697143653539,3.40993160175972));
#25313=CARTESIAN_POINT('Ctrl Pts',(-49.8400930231159,2.99843101344648,3.90758063337172));
#25314=CARTESIAN_POINT('Ctrl Pts',(-49.8004566901176,2.34989059035758,4.40522966498371));
#25315=CARTESIAN_POINT('Ctrl Pts',(-49.7608203571192,1.57478698963928,4.73794049401699));
#25316=CARTESIAN_POINT('Ctrl Pts',(-49.7211840241209,0.767295978068213,
4.86528846323715));
#25317=CARTESIAN_POINT('Ctrl Pts',(-49.6815476911226,-0.0401950335028599,
4.99263643245731));
#25318=CARTESIAN_POINT('Ctrl Pts',(-49.6419113581243,-0.880073455926696,
4.91462154186436));
#25319=CARTESIAN_POINT('Ctrl Pts',(-49.6022750251259,-1.65029332484226,
4.64072266899981));
#25320=CARTESIAN_POINT('Ctrl Pts',(-49.5626386921276,-2.42051319375783,
4.36682379613526));
#25321=CARTESIAN_POINT('Ctrl Pts',(-49.5230023591293,-3.12107450916513,
3.89704094099911));
#25322=CARTESIAN_POINT('Ctrl Pts',(-49.483366026131,-3.66685845728901,3.28845313221103));
#25323=CARTESIAN_POINT('Ctrl Pts',(-49.4437296931327,-4.21264240541289,
2.67986532342297));
#25324=CARTESIAN_POINT('Ctrl Pts',(-49.4040933601344,-4.60364898625336,
1.93247256098297));
#25325=CARTESIAN_POINT('Ctrl Pts',(-49.364457027136,-4.79237055757407,1.13708372051014));
#25326=CARTESIAN_POINT('Ctrl Pts',(-49.3459185267252,-4.88063843360605,
0.765068571013696));
#25327=CARTESIAN_POINT('Ctrl Pts',(-49.3273800263144,-4.92465501661941,
0.382553936074322));
#25328=CARTESIAN_POINT('Ctrl Pts',(-49.3088415259036,-4.92458892021405,
2.43377720096698E-5));
#25329=CARTESIAN_POINT('Origin',(-41.25,0.,0.));
#25330=CARTESIAN_POINT('',(-47.5911584740964,-4.92537656845547,5.17146674012571E-5));
#25331=CARTESIAN_POINT('',(-47.8088415259036,-4.92534557603861,6.69665181946809E-5));
#25332=CARTESIAN_POINT('',(-41.25,-4.925,-6.03138548580071E-16));
#25333=CARTESIAN_POINT('Ctrl Pts',(-47.5911584740964,-4.92537656845547,
5.17146674012571E-5));
#25334=CARTESIAN_POINT('Ctrl Pts',(-47.5936162664824,-4.92540395716342,
0.0507432792115421));
#25335=CARTESIAN_POINT('Ctrl Pts',(-47.5960740588683,-4.92463762300913,
0.101434014089762));
#25336=CARTESIAN_POINT('Ctrl Pts',(-47.5985318512543,-4.92307227746004,
0.152100063227692));
#25337=CARTESIAN_POINT('Ctrl Pts',(-47.6381681842526,-4.89782825856099,
0.969181443579074));
#25338=CARTESIAN_POINT('Ctrl Pts',(-47.6778045172509,-4.66478233650121,
1.77984271046711));
#25339=CARTESIAN_POINT('Ctrl Pts',(-47.7174408502493,-4.25224979504508,
2.48558780952685));
#25340=CARTESIAN_POINT('Ctrl Pts',(-47.7570771832476,-3.83971725358897,
3.19133290858659));
#25341=CARTESIAN_POINT('Ctrl Pts',(-47.7967135162459,-3.24769809273652,
3.79216183981804));
#25342=CARTESIAN_POINT('Ctrl Pts',(-47.8363498492442,-2.54812315935826,
4.21507336152901));
#25343=CARTESIAN_POINT('Ctrl Pts',(-47.8759861822425,-1.84854822598001,
4.63798488323999));
#25344=CARTESIAN_POINT('Ctrl Pts',(-47.9156225152409,-1.04141752007597,
4.88297899543049));
#25345=CARTESIAN_POINT('Ctrl Pts',(-47.9552588482392,-0.224798129757426,
4.92028869876423));
#25346=CARTESIAN_POINT('Ctrl Pts',(-47.9948951812375,0.591821260561127,
4.95759840209797));
#25347=CARTESIAN_POINT('Ctrl Pts',(-48.0345315142358,1.41792933529417,4.78722369657496));
#25348=CARTESIAN_POINT('Ctrl Pts',(-48.0741678472341,2.15315323938652,4.42986525822725));
#25349=CARTESIAN_POINT('Ctrl Pts',(-48.1138041802324,2.88837714347886,4.07250681987955));
#25350=CARTESIAN_POINT('Ctrl Pts',(-48.1534405132308,3.5327168769305,3.52816464870717));
#25351=CARTESIAN_POINT('Ctrl Pts',(-48.1930768462291,4.00788459744799,2.8629767955519));
#25352=CARTESIAN_POINT('Ctrl Pts',(-48.2327131792274,4.48305231796546,2.19778894239665));
#25353=CARTESIAN_POINT('Ctrl Pts',(-48.2723495122258,4.7890480255488,1.41175540725851));
#25354=CARTESIAN_POINT('Ctrl Pts',(-48.3119858452241,4.8886929735616,0.600379953511863));
#25355=CARTESIAN_POINT('Ctrl Pts',(-48.3516221782224,4.9883379215744,-0.21099550023481));
#25356=CARTESIAN_POINT('Ctrl Pts',(-48.3912585112207,4.88163211001666,-1.04771287259));
#25357=CARTESIAN_POINT('Ctrl Pts',(-48.430894844219,4.58154038850627,-1.80811026953979));
#25358=CARTESIAN_POINT('Ctrl Pts',(-48.4705311772173,4.28144866699588,-2.56850766648958));
#25359=CARTESIAN_POINT('Ctrl Pts',(-48.5101675102157,3.78797103553283,-3.25258508803395));
#25360=CARTESIAN_POINT('Ctrl Pts',(-48.549803843214,3.16106545880817,-3.77722652795134));
#25361=CARTESIAN_POINT('Ctrl Pts',(-48.5894401762123,2.5341598820835,-4.30186796786874));
#25362=CARTESIAN_POINT('Ctrl Pts',(-48.6290765092106,1.77382636009721,-4.66707342615914));
#25363=CARTESIAN_POINT('Ctrl Pts',(-48.6687128422089,0.972446082103007,
-4.8284701195857));
#25364=CARTESIAN_POINT('Ctrl Pts',(-48.7083491752073,0.171065804108807,
-4.98986681301226));
#25365=CARTESIAN_POINT('Ctrl Pts',(-48.7479855082056,-0.671361229893299,
-4.94745474157497));
#25366=CARTESIAN_POINT('Ctrl Pts',(-48.7876218412039,-1.4524793969955,-4.70638700912207));
#25367=CARTESIAN_POINT('Ctrl Pts',(-48.8272581742023,-2.2335975640977,-4.46531927666918));
#25368=CARTESIAN_POINT('Ctrl Pts',(-48.8668945072005,-2.9534068643,-4.02559588320067));
#25369=CARTESIAN_POINT('Ctrl Pts',(-48.9065308401989,-3.52444983680959,
-3.44064360638272));
#25370=CARTESIAN_POINT('Ctrl Pts',(-48.9461671731972,-4.09549280931918,
-2.85569132956477));
#25371=CARTESIAN_POINT('Ctrl Pts',(-48.9858035061955,-4.51776945413606,
-2.12551016939737));
#25372=CARTESIAN_POINT('Ctrl Pts',(-49.0254398391939,-4.73997278884501,
-1.3388177767487));
#25373=CARTESIAN_POINT('Ctrl Pts',(-49.0473460508281,-4.86278014532179,
-0.904028563399918));
#25374=CARTESIAN_POINT('Ctrl Pts',(-49.0692522624622,-4.92447405499882,
-0.451977696320464));
#25375=CARTESIAN_POINT('Ctrl Pts',(-49.0911584740964,-4.92460059430091,
3.93170950760413E-5));
#25376=CARTESIAN_POINT('Ctrl Pts',(-49.3088415259036,-4.92458892021405,
2.43377720096698E-5));
#25377=CARTESIAN_POINT('Ctrl Pts',(-49.2877436933161,-4.92451369887121,
-0.435315373957988));
#25378=CARTESIAN_POINT('Ctrl Pts',(-49.2666458607286,-4.86734395233281,
-0.870674465773623));
#25379=CARTESIAN_POINT('Ctrl Pts',(-49.2455480281411,-4.75332821260385,
-1.29059902828803));
#25380=CARTESIAN_POINT('Ctrl Pts',(-49.2059116951427,-4.53912773451197,
-2.07950801810765));
#25381=CARTESIAN_POINT('Ctrl Pts',(-49.1662753621445,-4.12429021652726,
-2.81394107924121));
#25382=CARTESIAN_POINT('Ctrl Pts',(-49.1266390291461,-3.55921878063583,
-3.40466395112918));
#25383=CARTESIAN_POINT('Ctrl Pts',(-49.0870026961478,-2.9941473447444,-3.99538682301714));
#25384=CARTESIAN_POINT('Ctrl Pts',(-49.0473663631495,-2.27884199094625,
-4.44239950565951));
#25385=CARTESIAN_POINT('Ctrl Pts',(-49.0077300301511,-1.50021294659875,
-4.69138956636627));
#25386=CARTESIAN_POINT('Ctrl Pts',(-48.9680936971528,-0.721583902251253,
-4.94037962707302));
#25387=CARTESIAN_POINT('Ctrl Pts',(-48.9284573641545,0.120368832645595,
-4.99134706584417));
#25388=CARTESIAN_POINT('Ctrl Pts',(-48.8888210311562,0.923347262940818,
-4.8380992942033));
#25389=CARTESIAN_POINT('Ctrl Pts',(-48.8491846981579,1.72632569323603,-4.68485152256244));
#25390=CARTESIAN_POINT('Ctrl Pts',(-48.8095483651595,2.49032981892962,-4.32738854050958));
#25391=CARTESIAN_POINT('Ctrl Pts',(-48.7699120321612,3.1225324692007,-3.80914241363316));
#25392=CARTESIAN_POINT('Ctrl Pts',(-48.7302756991629,3.75473511947177,-3.29089628675674));
#25393=CARTESIAN_POINT('Ctrl Pts',(-48.6906393661646,4.25513629432032,-2.61186701505678));
#25394=CARTESIAN_POINT('Ctrl Pts',(-48.6510030331663,4.56293681246637,-1.85455725012484));
#25395=CARTESIAN_POINT('Ctrl Pts',(-48.611366700168,4.87073733061243,-1.0972474851929));
#25396=CARTESIAN_POINT('Ctrl Pts',(-48.5717303671696,4.98593719205599,-0.261657227028983));
#25397=CARTESIAN_POINT('Ctrl Pts',(-48.5320940341713,4.89453951267414,0.550688575715041));
#25398=CARTESIAN_POINT('Ctrl Pts',(-48.492457701173,4.80314183329228,1.36303437845905));
#25399=CARTESIAN_POINT('Ctrl Pts',(-48.4528213681747,4.50514661308501,2.15213572578318));
#25400=CARTESIAN_POINT('Ctrl Pts',(-48.4131850351763,4.03676053246116,2.82211611244389));
#25401=CARTESIAN_POINT('Ctrl Pts',(-48.373548702178,3.5683744518373,3.4920964991046));
#25402=CARTESIAN_POINT('Ctrl Pts',(-48.3339123691797,2.92959751079684,4.04295592510191));
#25403=CARTESIAN_POINT('Ctrl Pts',(-48.2942760361814,2.19804166748022,4.40776448742128));
#25404=CARTESIAN_POINT('Ctrl Pts',(-48.2546397031831,1.4664858241636,4.77257304974066));
#25405=CARTESIAN_POINT('Ctrl Pts',(-48.2150033701847,0.642151078570819,
4.9513307483821));
#25406=CARTESIAN_POINT('Ctrl Pts',(-48.1753670371864,-0.174805175287565,
4.92231836630303));
#25407=CARTESIAN_POINT('Ctrl Pts',(-48.1357307041881,-0.99176142914595,
4.89330598422397));
#25408=CARTESIAN_POINT('Ctrl Pts',(-48.0960943711898,-1.80133919126995,
4.65652352142439));
#25409=CARTESIAN_POINT('Ctrl Pts',(-48.0564580381915,-2.50517405407298,
4.24074025464317));
#25410=CARTESIAN_POINT('Ctrl Pts',(-48.0168217051931,-3.20900891687601,
3.82495698786194));
#25411=CARTESIAN_POINT('Ctrl Pts',(-47.9771853721948,-3.80710088035809,
3.23017291709908));
#25412=CARTESIAN_POINT('Ctrl Pts',(-47.9375490391965,-4.22678124680716,
2.52865482820229));
#25413=CARTESIAN_POINT('Ctrl Pts',(-47.8979127061982,-4.64646161325623,
1.82713673930551));
#25414=CARTESIAN_POINT('Ctrl Pts',(-47.8582763731999,-4.88773038267229,
1.01888463227482));
#25415=CARTESIAN_POINT('Ctrl Pts',(-47.8186400402016,-4.92127318813094,
0.202101846441171));
#25416=CARTESIAN_POINT('Ctrl Pts',(-47.8153738687689,-4.92403723174125,
0.134796109508387));
#25417=CARTESIAN_POINT('Ctrl Pts',(-47.8121076973363,-4.92539074707072,
0.067432446433504));
#25418=CARTESIAN_POINT('Ctrl Pts',(-47.8088415259036,-4.92534557603861,
6.69665181946809E-5));
#25419=CARTESIAN_POINT('Origin',(-41.25,0.,0.));
#25420=CARTESIAN_POINT('',(-46.0911584740964,-4.92478006052077,-0.000110922936781277));
#25421=CARTESIAN_POINT('',(-46.3088415259036,-4.92482432270619,-0.000117749303604396));
#25422=CARTESIAN_POINT('',(-41.25,-4.925,-6.03138548580071E-16));
#25423=CARTESIAN_POINT('Ctrl Pts',(-46.0911584740964,-4.92478006052077,
-0.000110922936781277));
#25424=CARTESIAN_POINT('Ctrl Pts',(-46.1179802705025,-4.92432113727213,
0.553277446459616));
#25425=CARTESIAN_POINT('Ctrl Pts',(-46.1448020669086,-4.83122565564324,
1.10681635025798));
#25426=CARTESIAN_POINT('Ctrl Pts',(-46.1716238633147,-4.64828498189497,
1.62887132868731));
#25427=CARTESIAN_POINT('Ctrl Pts',(-46.2112601963131,-4.37794151370094,
2.4003463132539));
#25428=CARTESIAN_POINT('Ctrl Pts',(-46.2508965293114,-3.91139485952201,
3.10306696251328));
#25429=CARTESIAN_POINT('Ctrl Pts',(-46.2905328623097,-3.30533084670784,
3.65165210173844));
#25430=CARTESIAN_POINT('Ctrl Pts',(-46.330169195308,-2.69926683389369,4.20023724096358));
#25431=CARTESIAN_POINT('Ctrl Pts',(-46.3698055283064,-1.95368546244432,
4.59468687015451));
#25432=CARTESIAN_POINT('Ctrl Pts',(-46.4094418613047,-1.15917552239483,
4.78707501368114));
#25433=CARTESIAN_POINT('Ctrl Pts',(-46.449078194303,-0.364665582345333,
4.97946315720777));
#25434=CARTESIAN_POINT('Ctrl Pts',(-46.4887145273013,0.478772926304282,
4.96978981507011));
#25435=CARTESIAN_POINT('Ctrl Pts',(-46.5283508602996,1.26866148559008,4.75923030681535));
#25436=CARTESIAN_POINT('Ctrl Pts',(-46.567987193298,2.05855004487589,4.54867079856059));
#25437=CARTESIAN_POINT('Ctrl Pts',(-46.6076235262963,2.79488865479788,4.13722512418875));
#25438=CARTESIAN_POINT('Ctrl Pts',(-46.6472598592946,3.38821152894656,3.57488429371401));
#25439=CARTESIAN_POINT('Ctrl Pts',(-46.6868961922929,3.98153440309523,3.01254346323927));
#25440=CARTESIAN_POINT('Ctrl Pts',(-46.7265325252913,4.4318415414706,2.29930747666162));
#25441=CARTESIAN_POINT('Ctrl Pts',(-46.7661688582896,4.68442023212502,1.52183513140787));
#25442=CARTESIAN_POINT('Ctrl Pts',(-46.8058051912879,4.93699892277945,0.744362786154099));
#25443=CARTESIAN_POINT('Ctrl Pts',(-46.8454415242862,4.99184916571294,-0.097345917775786));
#25444=CARTESIAN_POINT('Ctrl Pts',(-46.8850778572845,4.84230660834004,-0.901022635207284));
#25445=CARTESIAN_POINT('Ctrl Pts',(-46.9247141902828,4.69276405096713,-1.70469935263878));
#25446=CARTESIAN_POINT('Ctrl Pts',(-46.9643505232812,4.33882869328785,-2.47034408357189));
#25447=CARTESIAN_POINT('Ctrl Pts',(-47.0039868562795,3.82350399143802,-3.10493032221128));
#25448=CARTESIAN_POINT('Ctrl Pts',(-47.0436231892778,3.3081792895882,-3.73951656085065));
#25449=CARTESIAN_POINT('Ctrl Pts',(-47.0832595222761,2.63146524356784,-4.24304430719631));
#25450=CARTESIAN_POINT('Ctrl Pts',(-47.1228958552744,1.87558320301932,-4.55433449879137));
#25451=CARTESIAN_POINT('Ctrl Pts',(-47.1625321882727,1.11970116247081,-4.86562469038643));
#25452=CARTESIAN_POINT('Ctrl Pts',(-47.2021685212711,0.284651127394135,
-4.9846773272309));
#25453=CARTESIAN_POINT('Ctrl Pts',(-47.2418048542694,-0.5281075911373,-4.89702740961419));
#25454=CARTESIAN_POINT('Ctrl Pts',(-47.2814411872678,-1.34086630966875,
-4.80937749199747));
#25455=CARTESIAN_POINT('Ctrl Pts',(-47.3210775202661,-2.13133371165496,
-4.51502501991956));
#25456=CARTESIAN_POINT('Ctrl Pts',(-47.3607138532644,-2.80346731501383,
-4.04973407669918));
#25457=CARTESIAN_POINT('Ctrl Pts',(-47.4003501862627,-3.4756009183727,-3.58444313347881));
#25458=CARTESIAN_POINT('Ctrl Pts',(-47.439986519261,-4.02940072310423,-2.94821371911597));
#25459=CARTESIAN_POINT('Ctrl Pts',(-47.4796228522593,-4.39757956760083,
-2.21834826502719));
#25460=CARTESIAN_POINT('Ctrl Pts',(-47.5168013928717,-4.74292816791932,
-1.53374072508281));
#25461=CARTESIAN_POINT('Ctrl Pts',(-47.553979933484,-4.92496226487288,-0.766749583062766));
#25462=CARTESIAN_POINT('Ctrl Pts',(-47.5911584740964,-4.92537656845547,
5.17146674012571E-5));
#25463=CARTESIAN_POINT('Ctrl Pts',(-47.8088415259036,-4.92534557603861,
6.69665181946809E-5));
#25464=CARTESIAN_POINT('Ctrl Pts',(-47.7724713643379,-4.92484257802704,
-0.750075345052349));
#25465=CARTESIAN_POINT('Ctrl Pts',(-47.7361012027722,-4.75090613579548,
-1.50044294007547));
#25466=CARTESIAN_POINT('Ctrl Pts',(-47.6997310412066,-4.41988711904088,
-2.17356223823657));
#25467=CARTESIAN_POINT('Ctrl Pts',(-47.6600947082082,-4.05914140299093,
-2.90713007244404));
#25468=CARTESIAN_POINT('Ctrl Pts',(-47.6204583752099,-3.51183312938981,
-3.54895227622236));
#25469=CARTESIAN_POINT('Ctrl Pts',(-47.5808220422116,-2.8444607331238,-4.02104688933967));
#25470=CARTESIAN_POINT('Ctrl Pts',(-47.5411857092133,-2.17708833685779,
-4.49314150245699));
#25471=CARTESIAN_POINT('Ctrl Pts',(-47.501549376215,-1.3896518179269,-4.7955085249133));
#25472=CARTESIAN_POINT('Ctrl Pts',(-47.4619130432167,-0.577825403465827,
-4.89141009849522));
#25473=CARTESIAN_POINT('Ctrl Pts',(-47.4222767102183,0.234001010995242,
-4.98731167207714));
#25474=CARTESIAN_POINT('Ctrl Pts',(-47.38264037722,1.07021732098649,-4.87674779678467));
#25475=CARTESIAN_POINT('Ctrl Pts',(-47.3430040442217,1.82922251201032,-4.57315208036056));
#25476=CARTESIAN_POINT('Ctrl Pts',(-47.3033677112234,2.58822770303417,-4.26955636393644));
#25477=CARTESIAN_POINT('Ctrl Pts',(-47.2637313782251,3.27002177509061,-3.77292880638065));
#25478=CARTESIAN_POINT('Ctrl Pts',(-47.2240950452267,3.79176615092188,-3.14361009116501));
#25479=CARTESIAN_POINT('Ctrl Pts',(-47.1844587122284,4.31351052675315,-2.51429137594937));
#25480=CARTESIAN_POINT('Ctrl Pts',(-47.1448223792301,4.67520520635928,-1.75228150307386));
#25481=CARTESIAN_POINT('Ctrl Pts',(-47.1051860462318,4.83290396919025,-0.950165339894358));
#25482=CARTESIAN_POINT('Ctrl Pts',(-47.0655497132334,4.99060273202123,-0.148049176714858));
#25483=CARTESIAN_POINT('Ctrl Pts',(-47.0259133802351,4.94430557807706,0.694173276768634));
#25484=CARTESIAN_POINT('Ctrl Pts',(-46.9862770472368,4.69963765213535,1.47417125436063));
#25485=CARTESIAN_POINT('Ctrl Pts',(-46.9466407142385,4.45496972619363,2.25416923195263));
#25486=CARTESIAN_POINT('Ctrl Pts',(-46.9070043812402,4.01193102825436,2.97194273365312));
#25487=CARTESIAN_POINT('Ctrl Pts',(-46.8673680482418,3.42435114838233,3.54028164997137));
#25488=CARTESIAN_POINT('Ctrl Pts',(-46.8277317152435,2.83677126851031,4.10862056628962));
#25489=CARTESIAN_POINT('Ctrl Pts',(-46.7880953822452,2.10465020670554,4.52752489722563));
#25490=CARTESIAN_POINT('Ctrl Pts',(-46.7484590492469,1.31694131358517,4.74609739945611));
#25491=CARTESIAN_POINT('Ctrl Pts',(-46.7088227162486,0.529232420464796,
4.96466990168658));
#25492=CARTESIAN_POINT('Ctrl Pts',(-46.6691863832503,-0.314064303971186,
4.98291057521152));
#25493=CARTESIAN_POINT('Ctrl Pts',(-46.6295500502519,-1.11048756866507,
4.79860316221208));
#25494=CARTESIAN_POINT('Ctrl Pts',(-46.5899137172536,-1.90691083335896,
4.61429574921265));
#25495=CARTESIAN_POINT('Ctrl Pts',(-46.5502773842553,-2.65646063831076,
4.22744024968884));
#25496=CARTESIAN_POINT('Ctrl Pts',(-46.5106410512569,-3.26806602533696,
3.6850399458608));
#25497=CARTESIAN_POINT('Ctrl Pts',(-46.4710047182586,-3.87967141236316,
3.14263964203275));
#25498=CARTESIAN_POINT('Ctrl Pts',(-46.4313683852603,-4.35333238146376,
2.44469453390046));
#25499=CARTESIAN_POINT('Ctrl Pts',(-46.391732052262,-4.63149870979145,1.67600556375914));
#25500=CARTESIAN_POINT('Ctrl Pts',(-46.3641018768092,-4.82540626569679,
1.14015853889599));
#25501=CARTESIAN_POINT('Ctrl Pts',(-46.3364717013564,-4.92431565913374,
0.569934423846609));
#25502=CARTESIAN_POINT('Ctrl Pts',(-46.3088415259036,-4.92482432270619,
-0.000117749303604396));
#25503=CARTESIAN_POINT('Origin',(-41.25,0.,0.));
#25504=CARTESIAN_POINT('',(-44.5911584740964,-4.92485068894608,0.000120817416453672));
#25505=CARTESIAN_POINT('',(-44.8088415259036,-4.9248046659208,0.000114993715491958));
#25506=CARTESIAN_POINT('',(-41.25,-4.925,-6.03138548580071E-16));
#25507=CARTESIAN_POINT('Ctrl Pts',(-44.5911584740964,-4.92485068894608,
0.000120817416453672));
#25508=CARTESIAN_POINT('Ctrl Pts',(-44.6027079415244,-4.92507068379112,
0.238400082149576));
#25509=CARTESIAN_POINT('Ctrl Pts',(-44.6142574089523,-4.90808726014739,
0.476648255516139));
#25510=CARTESIAN_POINT('Ctrl Pts',(-44.6258068763803,-4.87363743235764,
0.712343494047093));
#25511=CARTESIAN_POINT('Ctrl Pts',(-44.6654432093786,-4.75540991628145,
1.52122018198193));
#25512=CARTESIAN_POINT('Ctrl Pts',(-44.7050795423769,-4.43146713264999,
2.30002899398948));
#25513=CARTESIAN_POINT('Ctrl Pts',(-44.7447158753752,-3.94116841268779,
2.95414397473762));
#25514=CARTESIAN_POINT('Ctrl Pts',(-44.7843522083736,-3.4508696927256,3.60825895548577));
#25515=CARTESIAN_POINT('Ctrl Pts',(-44.8239885413719,-2.79421503643267,
4.13768010497451));
#25516=CARTESIAN_POINT('Ctrl Pts',(-44.8636248743702,-2.05098856046108,
4.47808229065024));
#25517=CARTESIAN_POINT('Ctrl Pts',(-44.9032612073685,-1.3077620844895,4.81848447632595));
#25518=CARTESIAN_POINT('Ctrl Pts',(-44.9428975403668,-0.47796378883926,
4.96986769818865));
#25519=CARTESIAN_POINT('Ctrl Pts',(-44.9825338733652,0.33758510658002,4.91383876157463));
#25520=CARTESIAN_POINT('Ctrl Pts',(-45.0221702063635,1.1531340019993,4.85780982496061));
#25521=CARTESIAN_POINT('Ctrl Pts',(-45.0618065393618,1.95443349718762,4.59436872986986));
#25522=CARTESIAN_POINT('Ctrl Pts',(-45.1014428723601,2.64412500113517,4.15552380049798));
#25523=CARTESIAN_POINT('Ctrl Pts',(-45.1410792053584,3.33381650508272,3.71667887112609));
#25524=CARTESIAN_POINT('Ctrl Pts',(-45.1807155383567,3.9119000177895,3.10243010747307));
#25525=CARTESIAN_POINT('Ctrl Pts',(-45.2203518713551,4.30813788590293,2.38740927249545));
#25526=CARTESIAN_POINT('Ctrl Pts',(-45.2599882043534,4.70437575401636,1.67238843751783));
#25527=CARTESIAN_POINT('Ctrl Pts',(-45.2996245373517,4.91876797753645,0.856595531215603));
#25528=CARTESIAN_POINT('Ctrl Pts',(-45.33926087035,4.9252657133911,0.039150106707696));
#25529=CARTESIAN_POINT('Ctrl Pts',(-45.3788972033484,4.93176344924574,-0.778295317800222));
#25530=CARTESIAN_POINT('Ctrl Pts',(-45.4185335363467,4.73036669743492,-1.59739326051383));
#25531=CARTESIAN_POINT('Ctrl Pts',(-45.458169869345,4.34554533981538,-2.31862260359579));
#25532=CARTESIAN_POINT('Ctrl Pts',(-45.4978062023433,3.96072398219585,-3.03985194667775));
#25533=CARTESIAN_POINT('Ctrl Pts',(-45.5374425353416,3.39247801876759,-3.66321269012808));
#25534=CARTESIAN_POINT('Ctrl Pts',(-45.57707886834,2.70984983207305,-4.11296595730674));
#25535=CARTESIAN_POINT('Ctrl Pts',(-45.6167152013383,2.02722164537851,-4.5627192244854));
#25536=CARTESIAN_POINT('Ctrl Pts',(-45.6563515343366,1.23021123541768,-4.8388650153924));
#25537=CARTESIAN_POINT('Ctrl Pts',(-45.6959878673349,0.415656065479166,
-4.90785137443562));
#25538=CARTESIAN_POINT('Ctrl Pts',(-45.7356242003332,-0.398899104459364,
-4.97683773347883));
#25539=CARTESIAN_POINT('Ctrl Pts',(-45.7752605333315,-1.23099903437559,
-4.83866466065824));
#25540=CARTESIAN_POINT('Ctrl Pts',(-45.8148968663299,-1.97954285356023,
-4.51012030540781));
#25541=CARTESIAN_POINT('Ctrl Pts',(-45.8545331993282,-2.72808667274487,
-4.18157595015737));
#25542=CARTESIAN_POINT('Ctrl Pts',(-45.8941695323265,-3.39307438119792,
-3.6626603124771));
#25543=CARTESIAN_POINT('Ctrl Pts',(-45.9338058653248,-3.89370938956717,
-3.01642209710863));
#25544=CARTESIAN_POINT('Ctrl Pts',(-45.9734421983232,-4.39434439793641,
-2.37018388174015));
#25545=CARTESIAN_POINT('Ctrl Pts',(-46.0130785313215,-4.73062670622184,
-1.59662308868348));
#25546=CARTESIAN_POINT('Ctrl Pts',(-46.0527148643198,-4.86169771925999,
-0.789728032218253));
#25547=CARTESIAN_POINT('Ctrl Pts',(-46.065529400912,-4.90407334197024,-0.528856618417667));
#25548=CARTESIAN_POINT('Ctrl Pts',(-46.0783439375042,-4.92499931834652,
-0.264500951179397));
#25549=CARTESIAN_POINT('Ctrl Pts',(-46.0911584740964,-4.92478006052077,
-0.000110922936781277));
#25550=CARTESIAN_POINT('Ctrl Pts',(-46.3088415259036,-4.92482432270619,
-0.000117749303604396));
#25551=CARTESIAN_POINT('Ctrl Pts',(-46.2968353683581,-4.92504535260877,
-0.247822879214976));
#25552=CARTESIAN_POINT('Ctrl Pts',(-46.2848292108125,-4.90668666485232,
-0.495495543595402));
#25553=CARTESIAN_POINT('Ctrl Pts',(-46.272823053267,-4.86946908996704,-0.740301107933112));
#25554=CARTESIAN_POINT('Ctrl Pts',(-46.2331867202687,-4.74660145426015,
-1.54848597733368));
#25555=CARTESIAN_POINT('Ctrl Pts',(-46.1935503872704,-4.41819449529159,
-2.32542288398449));
#25556=CARTESIAN_POINT('Ctrl Pts',(-46.1539140542721,-3.92414994638157,
-2.97671331284438));
#25557=CARTESIAN_POINT('Ctrl Pts',(-46.1142777212738,-3.43010539747155,
-3.62800374170428));
#25558=CARTESIAN_POINT('Ctrl Pts',(-46.0746413882754,-2.77042325862007,
-4.15364769277325));
#25559=CARTESIAN_POINT('Ctrl Pts',(-46.0350050552771,-2.02525548782224,
-4.48977896533864));
#25560=CARTESIAN_POINT('Ctrl Pts',(-45.9953687222788,-1.28008771702442,
-4.82591023790403));
#25561=CARTESIAN_POINT('Ctrl Pts',(-45.9557323892805,-0.449434314280258,
-4.97252883196583));
#25562=CARTESIAN_POINT('Ctrl Pts',(-45.9160960562821,0.365779604018302,
-4.91182045985354));
#25563=CARTESIAN_POINT('Ctrl Pts',(-45.8764597232838,1.18099352231686,-4.85111208774125));
#25564=CARTESIAN_POINT('Ctrl Pts',(-45.8368233902855,1.98076795616981,-4.58307674945487));
#25565=CARTESIAN_POINT('Ctrl Pts',(-45.7971870572872,2.6679296109669,-4.14028097349408));
#25566=CARTESIAN_POINT('Ctrl Pts',(-45.7575507242889,3.35509126576401,-3.69748519753329));
#25567=CARTESIAN_POINT('Ctrl Pts',(-45.7179143912905,3.92964014150524,-3.07992898389807));
#25568=CARTESIAN_POINT('Ctrl Pts',(-45.6782780582922,4.32176804627143,-2.36264595375167));
#25569=CARTESIAN_POINT('Ctrl Pts',(-45.6386417252939,4.71389595103761,-1.64536292360528));
#25570=CARTESIAN_POINT('Ctrl Pts',(-45.5990053922956,4.92360288482874,-0.828353076947685));
#25571=CARTESIAN_POINT('Ctrl Pts',(-45.5593690592973,4.92540927140877,-0.0108838261501201));
#25572=CARTESIAN_POINT('Ctrl Pts',(-45.519732726299,4.9272156579888,0.806585424647439));
#25573=CARTESIAN_POINT('Ctrl Pts',(-45.4800963933006,4.72112149735772,1.62451407958498));
#25574=CARTESIAN_POINT('Ctrl Pts',(-45.4404600603023,4.3321674106464,2.34352309028179));
#25575=CARTESIAN_POINT('Ctrl Pts',(-45.4008237273039,3.94321332393509,3.06253210097861));
#25576=CARTESIAN_POINT('Ctrl Pts',(-45.3611873943057,3.37139931114353,3.6826214674347));
#25577=CARTESIAN_POINT('Ctrl Pts',(-45.3215510613074,2.68620127594623,4.12844978819655));
#25578=CARTESIAN_POINT('Ctrl Pts',(-45.281914728309,2.00100324074892,4.5742781089584));
#25579=CARTESIAN_POINT('Ctrl Pts',(-45.2422783953107,1.20242118314586,4.84584538402601));
#25580=CARTESIAN_POINT('Ctrl Pts',(-45.2026420623123,0.387483522987002,
4.9101559514902));
#25581=CARTESIAN_POINT('Ctrl Pts',(-45.163005729314,-0.427454137171852,
4.9744665189544));
#25582=CARTESIAN_POINT('Ctrl Pts',(-45.1233693963158,-1.25874739988651,
4.83152037881518));
#25583=CARTESIAN_POINT('Ctrl Pts',(-45.0837330633174,-2.00539340521582,
4.49868561236386));
#25584=CARTESIAN_POINT('Ctrl Pts',(-45.0440967303191,-2.75203941054511,
4.16585084591255));
#25585=CARTESIAN_POINT('Ctrl Pts',(-45.0044603973208,-3.41403815848903,
3.64312745314915));
#25586=CARTESIAN_POINT('Ctrl Pts',(-44.9648240643225,-3.91095622102169,
2.9940267844109));
#25587=CARTESIAN_POINT('Ctrl Pts',(-44.9251877313241,-4.40787428355437,
2.34492611567263));
#25588=CARTESIAN_POINT('Ctrl Pts',(-44.8855513983258,-4.73971166067577,
1.5694481709595));
#25589=CARTESIAN_POINT('Ctrl Pts',(-44.8459150653275,-4.8661498202455,0.761814200122423));
#25590=CARTESIAN_POINT('Ctrl Pts',(-44.8335572188529,-4.90557080716081,
0.510009457748148));
#25591=CARTESIAN_POINT('Ctrl Pts',(-44.8211993723782,-4.92502550111584,
0.255078916523799));
#25592=CARTESIAN_POINT('Ctrl Pts',(-44.8088415259036,-4.9248046659208,0.000114993715491958));
#25593=CARTESIAN_POINT('Origin',(-41.25,0.,0.));
#25594=CARTESIAN_POINT('',(-43.0911584740964,-4.92532729948334,-7.01527563526372E-5));
#25595=CARTESIAN_POINT('',(-43.3088415259036,-4.92535985208058,-6.05620874156806E-5));
#25596=CARTESIAN_POINT('',(-41.25,-4.925,-6.03138548580071E-16));
#25597=CARTESIAN_POINT('Ctrl Pts',(-43.0911584740964,-4.92532729948334,
-7.01527563526372E-5));
#25598=CARTESIAN_POINT('Ctrl Pts',(-43.1270719455445,-4.92478402712806,
0.740663394333482));
#25599=CARTESIAN_POINT('Ctrl Pts',(-43.1629854169926,-4.75533079067205,
1.48162892060557));
#25600=CARTESIAN_POINT('Ctrl Pts',(-43.1988988884407,-4.43228738909528,
2.14815911814967));
#25601=CARTESIAN_POINT('Ctrl Pts',(-43.2385352214391,-4.07575666896397,
2.8837831555383));
#25602=CARTESIAN_POINT('Ctrl Pts',(-43.2781715544374,-3.53214241241189,
3.52873976951395));
#25603=CARTESIAN_POINT('Ctrl Pts',(-43.3178078874357,-2.8674907220931,4.00465760137893));
#25604=CARTESIAN_POINT('Ctrl Pts',(-43.357444220434,-2.20283903177432,4.4805754332439));
#25605=CARTESIAN_POINT('Ctrl Pts',(-43.3970805534323,-1.41714990768884,
4.7874544829982));
#25606=CARTESIAN_POINT('Ctrl Pts',(-43.4367168864307,-0.605887023971831,
4.88801296947649));
#25607=CARTESIAN_POINT('Ctrl Pts',(-43.476353219429,0.20537585974518,4.98857145595478));
#25608=CARTESIAN_POINT('Ctrl Pts',(-43.5159895524273,1.04221250309372,4.88280937915706));
#25609=CARTESIAN_POINT('Ctrl Pts',(-43.5556258854256,1.80294740105899,4.58357477299046));
#25610=CARTESIAN_POINT('Ctrl Pts',(-43.5952622184239,2.56368229902428,4.28434016682385));
#25611=CARTESIAN_POINT('Ctrl Pts',(-43.6348985514223,3.24831545160629,3.79163303128835));
#25612=CARTESIAN_POINT('Ctrl Pts',(-43.6745348844206,3.77366288949504,3.16531879318089));
#25613=CARTESIAN_POINT('Ctrl Pts',(-43.7141712174189,4.29901032738379,2.53900455507344));
#25614=CARTESIAN_POINT('Ctrl Pts',(-43.7538075504172,4.66507205057929,1.77908321439402));
#25615=CARTESIAN_POINT('Ctrl Pts',(-43.7934438834155,4.82737146005745,0.977885339744746));
#25616=CARTESIAN_POINT('Ctrl Pts',(-43.8330802164138,4.98967086953561,0.176687465095475));
#25617=CARTESIAN_POINT('Ctrl Pts',(-43.8727165494122,4.94820796529643,-0.665786943523648));
#25618=CARTESIAN_POINT('Ctrl Pts',(-43.9123528824105,4.7080204157121,-1.44717623639338));
#25619=CARTESIAN_POINT('Ctrl Pts',(-43.9519892154088,4.46783286612776,-2.22856552926312));
#25620=CARTESIAN_POINT('Ctrl Pts',(-43.9916255484071,4.02892067119828,-2.94886970638347));
#25621=CARTESIAN_POINT('Ctrl Pts',(-44.0312618814055,3.44461210279907,-3.52057131467165));
#25622=CARTESIAN_POINT('Ctrl Pts',(-44.0708982144038,2.86030353439988,-4.09227292295982));
#25623=CARTESIAN_POINT('Ctrl Pts',(-44.1105345474021,2.13059859253097,-4.51537196241583));
#25624=CARTESIAN_POINT('Ctrl Pts',(-44.1501708804004,1.34415703928449,-4.73846146095394));
#25625=CARTESIAN_POINT('Ctrl Pts',(-44.1898072133987,0.557715486037999,
-4.96155095949204));
#25626=CARTESIAN_POINT('Ctrl Pts',(-44.2294435463971,-0.285462678586069,
-4.98463091711224));
#25627=CARTESIAN_POINT('Ctrl Pts',(-44.2690798793954,-1.08293055470127,
-4.80489713281615));
#25628=CARTESIAN_POINT('Ctrl Pts',(-44.3087162123937,-1.88039843081648,
-4.62516334852005));
#25629=CARTESIAN_POINT('Ctrl Pts',(-44.348352545392,-2.63215601842282,-4.24261582230765));
#25630=CARTESIAN_POINT('Ctrl Pts',(-44.3879888783903,-3.24686411880041,
-3.70373439678756));
#25631=CARTESIAN_POINT('Ctrl Pts',(-44.4276252113887,-3.86157221917799,
-3.16485297126747));
#25632=CARTESIAN_POINT('Ctrl Pts',(-44.467261544387,-4.33923083232682,-2.4696376464397));
#25633=CARTESIAN_POINT('Ctrl Pts',(-44.5068978773853,-4.62180401464078,
-1.70255770209476));
#25634=CARTESIAN_POINT('Ctrl Pts',(-44.5349847429557,-4.82203936400522,
-1.15899401573013));
#25635=CARTESIAN_POINT('Ctrl Pts',(-44.563071608526,-4.92431568889719,-0.579344661707689));
#25636=CARTESIAN_POINT('Ctrl Pts',(-44.5911584740964,-4.92485068894608,
0.000120817416453672));
#25637=CARTESIAN_POINT('Ctrl Pts',(-44.8088415259036,-4.9248046659208,0.000114993715491958));
#25638=CARTESIAN_POINT('Ctrl Pts',(-44.7815630393799,-4.92431719831031,
-0.562687752428751));
#25639=CARTESIAN_POINT('Ctrl Pts',(-44.7542845528562,-4.82796002993066,
-1.12565315150297));
#25640=CARTESIAN_POINT('Ctrl Pts',(-44.7270060663325,-4.63886048406004,
-1.65552057009204));
#25641=CARTESIAN_POINT('Ctrl Pts',(-44.6873697333342,-4.36409404628679,
-2.42543137250844));
#25642=CARTESIAN_POINT('Ctrl Pts',(-44.6477334003359,-3.89352222872223,
-3.12546298038023));
#25643=CARTESIAN_POINT('Ctrl Pts',(-44.6080970673376,-3.28431991956177,
-3.67056094000945));
#25644=CARTESIAN_POINT('Ctrl Pts',(-44.5684607343393,-2.6751176104013,-4.21565889963868));
#25645=CARTESIAN_POINT('Ctrl Pts',(-44.5288244013409,-1.92728480964494,
-4.60582321102533));
#25646=CARTESIAN_POINT('Ctrl Pts',(-44.4891880683426,-1.13168385802756,
-4.79364856812068));
#25647=CARTESIAN_POINT('Ctrl Pts',(-44.4495517353443,-0.336082906410188,
-4.98147392521603));
#25648=CARTESIAN_POINT('Ctrl Pts',(-44.409915402346,0.507286196068199,-4.96696032802006));
#25649=CARTESIAN_POINT('Ctrl Pts',(-44.3702790693476,1.29595336448566,-4.75187119188491));
#25650=CARTESIAN_POINT('Ctrl Pts',(-44.3306427363493,2.08462053290311,-4.53678205574976));
#25651=CARTESIAN_POINT('Ctrl Pts',(-44.291006403351,2.81858576725963,-4.12111738067542));
#25652=CARTESIAN_POINT('Ctrl Pts',(-44.2513700703527,3.40867164809488,-3.55538078781478));
#25653=CARTESIAN_POINT('Ctrl Pts',(-44.2117337373544,3.99875752893012,-2.98964419495414));
#25654=CARTESIAN_POINT('Ctrl Pts',(-44.1720974043561,4.44496405624409,-2.2738356843072));
#25655=CARTESIAN_POINT('Ctrl Pts',(-44.1324610713577,4.69307674644938,-1.49492661951182));
#25656=CARTESIAN_POINT('Ctrl Pts',(-44.0928247383594,4.94118943665468,-0.716017554716438));
#25657=CARTESIAN_POINT('Ctrl Pts',(-44.0531884053611,4.9912082897513,0.12599206422738));
#25658=CARTESIAN_POINT('Ctrl Pts',(-44.0135520723628,4.83705597021055,0.928797335259682));
#25659=CARTESIAN_POINT('Ctrl Pts',(-43.9739157393644,4.68290365066981,1.73160260629197));
#25660=CARTESIAN_POINT('Ctrl Pts',(-43.9342794063661,4.32458015849171,2.49520352941275));
#25661=CARTESIAN_POINT('Ctrl Pts',(-43.8946430733678,3.80562211407888,3.12682191418588));
#25662=CARTESIAN_POINT('Ctrl Pts',(-43.8550067403695,3.28666406966605,3.75844029895903));
#25663=CARTESIAN_POINT('Ctrl Pts',(-43.8153704073711,2.60707147301845,4.25807614538456));
#25664=CARTESIAN_POINT('Ctrl Pts',(-43.7757340743728,1.84941541605414,4.56502327837135));
#25665=CARTESIAN_POINT('Ctrl Pts',(-43.7360977413745,1.09175935908982,4.87197041135815));
#25666=CARTESIAN_POINT('Ctrl Pts',(-43.6964614083762,0.256039841808794,
4.98622883090624));
#25667=CARTESIAN_POINT('Ctrl Pts',(-43.6568250753779,-0.556202473766204,
4.89391600277317));
#25668=CARTESIAN_POINT('Ctrl Pts',(-43.6171887423796,-1.36844478934118,
4.80160317464009));
#25669=CARTESIAN_POINT('Ctrl Pts',(-43.5775524093812,-2.15720990321009,
4.50271909882586));
#25670=CARTESIAN_POINT('Ctrl Pts',(-43.5379160763829,-2.8266621792954,4.03357852455539));
#25671=CARTESIAN_POINT('Ctrl Pts',(-43.4982797433846,-3.49611445538071,
3.56443795028493));
#25672=CARTESIAN_POINT('Ctrl Pts',(-43.4586434103863,-4.04625389368242,
2.92504087755824));
#25673=CARTESIAN_POINT('Ctrl Pts',(-43.419007077388,-4.41023803739531,2.19307446727405));
#25674=CARTESIAN_POINT('Ctrl Pts',(-43.3822852268932,-4.7474582163777,1.51492997073843));
#25675=CARTESIAN_POINT('Ctrl Pts',(-43.3455633763984,-4.92489281945989,
0.757328991673029));
#25676=CARTESIAN_POINT('Ctrl Pts',(-43.3088415259036,-4.92535985208058,
-6.05620874156806E-5));
#25677=CARTESIAN_POINT('Origin',(-41.25,0.,0.));
#25678=CARTESIAN_POINT('',(-41.5911584740964,-4.92312360382807,0.0065423075118709));
#25679=CARTESIAN_POINT('',(-41.8088415259036,-4.92470507325415,0.000456942424287175));
#25680=CARTESIAN_POINT('',(-41.25,-4.925,-6.03138548580071E-16));
#25681=CARTESIAN_POINT('Ctrl Pts',(-41.5911584740964,-4.92312360382807,
0.0065423075118709));
#25682=CARTESIAN_POINT('Ctrl Pts',(-41.6117996165663,-4.92719160457478,
0.433012434324011));
#25683=CARTESIAN_POINT('Ctrl Pts',(-41.6324407590363,-4.87680224873628,
0.858320394691805));
#25684=CARTESIAN_POINT('Ctrl Pts',(-41.6530819015062,-4.76835722634153,
1.26767901413433));
#25685=CARTESIAN_POINT('Ctrl Pts',(-41.7323545675029,-4.35187223517315,
2.83982789877944));
#25686=CARTESIAN_POINT('Ctrl Pts',(-41.8116272334995,-3.07909091744468,
4.17673080563311));
#25687=CARTESIAN_POINT('Ctrl Pts',(-41.8908998994962,-1.52838050839828,
4.68726148274619));
#25688=CARTESIAN_POINT('Ctrl Pts',(-41.9305362324945,-0.753025303875076,
4.94252682130273));
#25689=CARTESIAN_POINT('Ctrl Pts',(-41.9701725654928,0.0918121734776089,
4.99119910242413));
#25690=CARTESIAN_POINT('Ctrl Pts',(-42.0098088984911,0.896430390440525,
4.84098316384975));
#25691=CARTESIAN_POINT('Ctrl Pts',(-42.0494452314894,1.70104860740344,4.69076722527537));
#25692=CARTESIAN_POINT('Ctrl Pts',(-42.0890815644878,2.46544756397659,4.34166306700522));
#25693=CARTESIAN_POINT('Ctrl Pts',(-42.1287178974861,3.10020506573018,3.82803047845904));
#25694=CARTESIAN_POINT('Ctrl Pts',(-42.1683542304844,3.7349625674838,3.31439788991284));
#25695=CARTESIAN_POINT('Ctrl Pts',(-42.2079905634827,4.24007861441785,2.63623687109061));
#25696=CARTESIAN_POINT('Ctrl Pts',(-42.247626896481,4.55242617457846,1.88020454684251));
#25697=CARTESIAN_POINT('Ctrl Pts',(-42.2872632294794,4.86477373473906,1.12417222259442));
#25698=CARTESIAN_POINT('Ctrl Pts',(-42.3268995624777,4.98435280812624,0.290268592920477));
#25699=CARTESIAN_POINT('Ctrl Pts',(-42.366535895476,4.89751528977223,-0.52233608303516));
#25700=CARTESIAN_POINT('Ctrl Pts',(-42.4061722284743,4.81067777141822,-1.3349407589908));
#25701=CARTESIAN_POINT('Ctrl Pts',(-42.4458085614726,4.51742366132304,-2.12624648122812));
#25702=CARTESIAN_POINT('Ctrl Pts',(-42.485444894471,4.05294203299736,-2.79903036183311));
#25703=CARTESIAN_POINT('Ctrl Pts',(-42.5250812274693,3.58846040467168,-3.47181424243811));
#25704=CARTESIAN_POINT('Ctrl Pts',(-42.5647175604676,2.95275125811554,-4.02607628141074));
#25705=CARTESIAN_POINT('Ctrl Pts',(-42.6043538934659,2.22327510854644,-4.3950137648464));
#25706=CARTESIAN_POINT('Ctrl Pts',(-42.6439902264642,1.49379895897736,-4.76395124828203));
#25707=CARTESIAN_POINT('Ctrl Pts',(-42.6836265594626,0.670555806395326,
-4.94756417618069));
#25708=CARTESIAN_POINT('Ctrl Pts',(-42.7232628924609,-0.146540489007751,
-4.9232724815208));
#25709=CARTESIAN_POINT('Ctrl Pts',(-42.7628992254592,-0.963636784410876,
-4.89898078686091));
#25710=CARTESIAN_POINT('Ctrl Pts',(-42.8025355584575,-1.77458622263507,
-4.66678446964245));
#25711=CARTESIAN_POINT('Ctrl Pts',(-42.8421718914558,-2.4808021561186,-4.2550313666284));
#25712=CARTESIAN_POINT('Ctrl Pts',(-42.8818082244542,-3.18701808960212,
-3.84327826361436));
#25713=CARTESIAN_POINT('Ctrl Pts',(-42.9214445574525,-3.78850051834497,
-3.25196837480472));
#25714=CARTESIAN_POINT('Ctrl Pts',(-42.9610808904508,-4.2121966543097,-2.55287832287441));
#25715=CARTESIAN_POINT('Ctrl Pts',(-43.0007172234491,-4.63589279027442,
-1.8537882709441));
#25716=CARTESIAN_POINT('Ctrl Pts',(-43.0403535564474,-4.88180263346103,
-1.04691805589312));
#25717=CARTESIAN_POINT('Ctrl Pts',(-43.0799898894458,-4.92003396319907,
-0.230337217966836));
#25718=CARTESIAN_POINT('Ctrl Pts',(-43.083712750996,-4.92362485914551,-0.153639471878947));
#25719=CARTESIAN_POINT('Ctrl Pts',(-43.0874356125462,-4.92538361617124,
-0.0768560587192995));
#25720=CARTESIAN_POINT('Ctrl Pts',(-43.0911584740964,-4.92532729948334,
-7.01527563526372E-5));
#25721=CARTESIAN_POINT('Ctrl Pts',(-43.3088415259036,-4.92535985208058,
-6.05620874156806E-5));
#25722=CARTESIAN_POINT('Ctrl Pts',(-43.3059270434001,-4.92539691879654,
-0.0601718738282288));
#25723=CARTESIAN_POINT('Ctrl Pts',(-43.3030125608965,-4.92431926118984,
-0.12028185379436));
#25724=CARTESIAN_POINT('Ctrl Pts',(-43.300098078393,-4.92211828943658,-0.180350673472536));
#25725=CARTESIAN_POINT('Ctrl Pts',(-43.2604617453947,-4.89218554864086,
-0.997273656093239));
#25726=CARTESIAN_POINT('Ctrl Pts',(-43.2208254123963,-4.65449121792534,
-1.80658387349296));
#25727=CARTESIAN_POINT('Ctrl Pts',(-43.181189079398,-4.23791523576072,-2.50994999714146));
#25728=CARTESIAN_POINT('Ctrl Pts',(-43.1415527463997,-3.8213392535961,-3.21331612078998));
#25729=CARTESIAN_POINT('Ctrl Pts',(-43.1019164134014,-3.22588161998236,
-3.81073815068729));
#25730=CARTESIAN_POINT('Ctrl Pts',(-43.0622800804031,-2.52389122059721,
-4.22962764535383));
#25731=CARTESIAN_POINT('Ctrl Pts',(-43.0226437474048,-1.82190082121208,
-4.64851714002037));
#25732=CARTESIAN_POINT('Ctrl Pts',(-42.9830074144065,-1.01337765605554,
-4.88887409945616));
#25733=CARTESIAN_POINT('Ctrl Pts',(-42.9433710814081,-0.196557476917921,
-4.92149721905324));
#25734=CARTESIAN_POINT('Ctrl Pts',(-42.9037347484098,0.620262702219694,
-4.95412033865032));
#25735=CARTESIAN_POINT('Ctrl Pts',(-42.8640984154114,1.44537989533838,-4.77900961840868));
#25736=CARTESIAN_POINT('Ctrl Pts',(-42.8244620824131,2.17854060041163,-4.41743662298954));
#25737=CARTESIAN_POINT('Ctrl Pts',(-42.7848257494148,2.91170130548488,-4.0558636275704));
#25738=CARTESIAN_POINT('Ctrl Pts',(-42.7451894164165,3.55290552251269,-3.50782835697374));
#25739=CARTESIAN_POINT('Ctrl Pts',(-42.7055530834182,4.02424845167079,-2.83992663573984));
#25740=CARTESIAN_POINT('Ctrl Pts',(-42.6659167504199,4.4955913808289,-2.17202491450593));
#25741=CARTESIAN_POINT('Ctrl Pts',(-42.6262804174215,4.79707302211729,-1.38425674263476));
#25742=CARTESIAN_POINT('Ctrl Pts',(-42.5866440844232,4.89205895380208,-0.572318572971036));
#25743=CARTESIAN_POINT('Ctrl Pts',(-42.5470077514249,4.98704488548686,0.239619596692683));
#25744=CARTESIAN_POINT('Ctrl Pts',(-42.5073714184266,4.87553510756804,1.07572776414893));
#25745=CARTESIAN_POINT('Ctrl Pts',(-42.4677350854283,4.57108641037318,1.83438200794185));
#25746=CARTESIAN_POINT('Ctrl Pts',(-42.42809875243,4.26663771317832,2.59303625173476));
#25747=CARTESIAN_POINT('Ctrl Pts',(-42.3884624194316,3.76925009670744,3.27423657186432));
#25748=CARTESIAN_POINT('Ctrl Pts',(-42.3488260864333,3.13934012622938,3.79528843677308));
#25749=CARTESIAN_POINT('Ctrl Pts',(-42.309189753435,2.5094301557513,4.31634030168184));
#25750=CARTESIAN_POINT('Ctrl Pts',(-42.2695534204367,1.74699783126604,4.6772437113698));
#25751=CARTESIAN_POINT('Ctrl Pts',(-42.2299170874383,0.94471219436256,4.83400515256402));
#25752=CARTESIAN_POINT('Ctrl Pts',(-42.19028075444,0.142426557459092,4.99076659375824));
#25753=CARTESIAN_POINT('Ctrl Pts',(-42.1506444214417,-0.6997123918626,4.94338606645873));
#25754=CARTESIAN_POINT('Ctrl Pts',(-42.1110080884434,-1.47944955361049,
4.69790646084692));
#25755=CARTESIAN_POINT('Ctrl Pts',(-42.0713717554451,-2.25918671535837,
4.45242685523511));
#25756=CARTESIAN_POINT('Ctrl Pts',(-42.0317354224467,-2.97652208953246,
4.00884817131102));
#25757=CARTESIAN_POINT('Ctrl Pts',(-41.9920990894484,-3.54416810026081,
3.42049488856083));
#25758=CARTESIAN_POINT('Ctrl Pts',(-41.9524627564501,-4.11181411098918,
2.83214160581061));
#25759=CARTESIAN_POINT('Ctrl Pts',(-41.9128264234518,-4.52977075827182,
2.09901372423428));
#25760=CARTESIAN_POINT('Ctrl Pts',(-41.8731900904534,-4.74751667129617,
1.31132519489558));
#25761=CARTESIAN_POINT('Ctrl Pts',(-41.8517405689368,-4.86535162961004,
0.885061189616368));
#25762=CARTESIAN_POINT('Ctrl Pts',(-41.8302910474202,-4.92455446234782,
0.442818986350074));
#25763=CARTESIAN_POINT('Ctrl Pts',(-41.8088415259036,-4.92470507325415,
0.000456942424287175));
#25764=CARTESIAN_POINT('Origin',(-41.25,0.,0.));
#25765=CARTESIAN_POINT('',(-40.0911584740964,-4.92524004259795,0.000110578359120081));
#25766=CARTESIAN_POINT('',(-40.3088415259036,-4.92524227782323,-0.000582878416294945));
#25767=CARTESIAN_POINT('',(-41.25,-4.925,-6.03138548580071E-16));
#25768=CARTESIAN_POINT('Ctrl Pts',(-40.0911584740964,-4.92524004259795,
0.000110578359120081));
#25769=CARTESIAN_POINT('Ctrl Pts',(-40.0965272875882,-4.92534070715902,
0.110850123093416));
#25770=CARTESIAN_POINT('Ctrl Pts',(-40.1018961010799,-4.92168160674078,
0.221582646226159));
#25771=CARTESIAN_POINT('Ctrl Pts',(-40.1072649145717,-4.91421674044945,
0.332057546016099));
#25772=CARTESIAN_POINT('Ctrl Pts',(-40.14690124757,-4.85910588093371,1.14766045767274));
#25773=CARTESIAN_POINT('Ctrl Pts',(-40.1865375805684,-4.5965646381192,1.94922180436547));
#25774=CARTESIAN_POINT('Ctrl Pts',(-40.2261739135667,-4.15849852897051,
2.63942441705466));
#25775=CARTESIAN_POINT('Ctrl Pts',(-40.265810246565,-3.72043241982181,3.32962702974388));
#25776=CARTESIAN_POINT('Ctrl Pts',(-40.3054465795633,-3.1068414443389,3.90847090842957));
#25777=CARTESIAN_POINT('Ctrl Pts',(-40.3450829125617,-2.39226442208597,
4.30547987767221));
#25778=CARTESIAN_POINT('Ctrl Pts',(-40.38471924556,-1.67768739983307,4.70248884691484));
#25779=CARTESIAN_POINT('Ctrl Pts',(-40.4243555785583,-0.862124330810157,
4.91766290671443));
#25780=CARTESIAN_POINT('Ctrl Pts',(-40.4639919115566,-0.0446928256683937,
4.92514982034103));
#25781=CARTESIAN_POINT('Ctrl Pts',(-40.5036282445549,0.772738679473369,
4.93263673396762));
#25782=CARTESIAN_POINT('Ctrl Pts',(-40.5432645775532,1.59203862073399,4.73243650142123));
#25783=CARTESIAN_POINT('Ctrl Pts',(-40.5829009105516,2.31371317843134,4.3482917815222));
#25784=CARTESIAN_POINT('Ctrl Pts',(-40.6225372435499,3.03538773612872,3.96414706162317));
#25785=CARTESIAN_POINT('Ctrl Pts',(-40.6621735765482,3.65943691026281,3.39605785437153));
#25786=CARTESIAN_POINT('Ctrl Pts',(-40.7018099095465,4.10993480374446,2.71420833875427));
#25787=CARTESIAN_POINT('Ctrl Pts',(-40.7414462425449,4.56043269722609,2.03235882313705));
#25788=CARTESIAN_POINT('Ctrl Pts',(-40.7810825755432,4.83737931005529,1.23674899915422));
#25789=CARTESIAN_POINT('Ctrl Pts',(-40.8207189085415,4.907330772549,0.421732025992796));
#25790=CARTESIAN_POINT('Ctrl Pts',(-40.8603552415398,4.97728223504271,-0.393284947168637));
#25791=CARTESIAN_POINT('Ctrl Pts',(-40.8999915745381,4.84023854720093,-1.22770906950873));
#25792=CARTESIAN_POINT('Ctrl Pts',(-40.9396279075365,4.51245206730997,-1.97556704108476));
#25793=CARTESIAN_POINT('Ctrl Pts',(-40.9792642405348,4.18466558741899,-2.72342501266081));
#25794=CARTESIAN_POINT('Ctrl Pts',(-41.0189005735331,3.66613631547886,-3.38471683347276));
#25795=CARTESIAN_POINT('Ctrl Pts',(-41.0585369065314,3.02050095021258,-3.88783737408691));
#25796=CARTESIAN_POINT('Ctrl Pts',(-41.0981732395297,2.37486558494632,-4.39095791470104));
#25797=CARTESIAN_POINT('Ctrl Pts',(-41.1378095725281,1.60212412635394,-4.73590717511732));
#25798=CARTESIAN_POINT('Ctrl Pts',(-41.1774459055264,0.796172436899315,
-4.86543694202377));
#25799=CARTESIAN_POINT('Ctrl Pts',(-41.256718571523,-0.815730942009943,
-5.12449647583667));
#25800=CARTESIAN_POINT('Ctrl Pts',(-41.3359912375197,-2.5604752443682,-4.52187803561028));
#25801=CARTESIAN_POINT('Ctrl Pts',(-41.4152639035163,-3.65275306324319,
-3.3168713842788));
#25802=CARTESIAN_POINT('Ctrl Pts',(-41.473895427043,-4.46062185168256,-2.42562627552507));
#25803=CARTESIAN_POINT('Ctrl Pts',(-41.5325269505697,-4.91156837708445,
-1.20485349143866));
#25804=CARTESIAN_POINT('Ctrl Pts',(-41.5911584740964,-4.92312360382807,
0.0065423075118709));
#25805=CARTESIAN_POINT('Ctrl Pts',(-41.8088415259036,-4.92470507325415,
0.000456942424287175));
#25806=CARTESIAN_POINT('Ctrl Pts',(-41.7906547144219,-4.9248327745718,-0.374616930123598));
#25807=CARTESIAN_POINT('Ctrl Pts',(-41.7724679029402,-4.88250691188772,
-0.749776957992148));
#25808=CARTESIAN_POINT('Ctrl Pts',(-41.7542810914585,-4.79747141108739,
-1.11535651178711));
#25809=CARTESIAN_POINT('Ctrl Pts',(-41.7146447584602,-4.61214505908818,
-1.91210051203008));
#25810=CARTESIAN_POINT('Ctrl Pts',(-41.6750084254619,-4.22395717632369,
-2.66333933541497));
#25811=CARTESIAN_POINT('Ctrl Pts',(-41.6353720924635,-3.68111291696794,
-3.27330228550321));
#25812=CARTESIAN_POINT('Ctrl Pts',(-41.5957357594652,-3.13826865761218,
-3.88326523559146));
#25813=CARTESIAN_POINT('Ctrl Pts',(-41.5560994264669,-2.44076802166517,
-4.35195231238306));
#25814=CARTESIAN_POINT('Ctrl Pts',(-41.5164630934686,-1.67125955808265,
-4.63093578122739));
#25815=CARTESIAN_POINT('Ctrl Pts',(-41.4768267604703,-0.901751094500133,
-4.90991925007172));
#25816=CARTESIAN_POINT('Ctrl Pts',(-41.4371904274719,-0.0602348032821162,
-4.99919911096879));
#25817=CARTESIAN_POINT('Ctrl Pts',(-41.3975540944736,0.746297840191277,
-4.87333819933832));
#25818=CARTESIAN_POINT('Ctrl Pts',(-41.318281428477,2.35936312713807,-4.62161637607737));
#25819=CARTESIAN_POINT('Ctrl Pts',(-41.2390087624803,3.83249382310637,-3.5093314627062));
#25820=CARTESIAN_POINT('Ctrl Pts',(-41.1597360964837,4.49894414693498,-2.02576869565901));
#25821=CARTESIAN_POINT('Ctrl Pts',(-41.0804634304871,5.16539447076359,-0.542205928611831));
#25822=CARTESIAN_POINT('Ctrl Pts',(-41.0011907644904,5.02516442245251,1.31263469211137));
#25823=CARTESIAN_POINT('Ctrl Pts',(-40.9219180984938,4.14324287363601,2.6791371251985));
#25824=CARTESIAN_POINT('Ctrl Pts',(-40.8426454324971,3.26132132481951,4.04563955828564));
#25825=CARTESIAN_POINT('Ctrl Pts',(-40.7633727665005,1.63770827549757,4.9238038037367));
#25826=CARTESIAN_POINT('Ctrl Pts',(-40.6841001005038,0.00513262720455543,
4.93014800260014));
#25827=CARTESIAN_POINT('Ctrl Pts',(-40.6444637675055,-0.811155196941947,
4.93332010203186));
#25828=CARTESIAN_POINT('Ctrl Pts',(-40.6048274345072,-1.62968367083122,
4.71853718981668));
#25829=CARTESIAN_POINT('Ctrl Pts',(-40.5651911015089,-2.34850178207576,
4.32703294416875));
#25830=CARTESIAN_POINT('Ctrl Pts',(-40.5255547685105,-3.06731989332033,
3.93552869852081));
#25831=CARTESIAN_POINT('Ctrl Pts',(-40.4859184355122,-3.68642764192017,
3.36730311944011));
#25832=CARTESIAN_POINT('Ctrl Pts',(-40.4462821025139,-4.13139676932224,
2.6826592952111));
#25833=CARTESIAN_POINT('Ctrl Pts',(-40.4066457695156,-4.5763658967243,1.99801547098211));
#25834=CARTESIAN_POINT('Ctrl Pts',(-40.3670094365173,-4.84719640292859,
1.19695340160483));
#25835=CARTESIAN_POINT('Ctrl Pts',(-40.327373103519,-4.91062970795906,0.381402621774772));
#25836=CARTESIAN_POINT('Ctrl Pts',(-40.3211959109805,-4.92051558056338,
0.254301706760495));
#25837=CARTESIAN_POINT('Ctrl Pts',(-40.3150187184421,-4.92536414836018,
0.126848887041597));
#25838=CARTESIAN_POINT('Ctrl Pts',(-40.3088415259036,-4.92524227782323,
-0.000582878416294945));
#25839=CARTESIAN_POINT('Origin',(-41.25,0.,0.));
#25840=CARTESIAN_POINT('',(-38.5911584740964,-4.92495184350011,-0.000126817359744069));
#25841=CARTESIAN_POINT('',(-38.8088415259036,-4.92500387630964,-0.000126728579282317));
#25842=CARTESIAN_POINT('',(-41.25,-4.925,-6.03138548580071E-16));
#25843=CARTESIAN_POINT('Ctrl Pts',(-38.5911584740964,-4.92495184350011,
-0.000126817359744069));
#25844=CARTESIAN_POINT('Ctrl Pts',(-38.6208912916084,-4.92433626585009,
0.613260413089466));
#25845=CARTESIAN_POINT('Ctrl Pts',(-38.6506241091203,-4.80942795756713,
1.226871817165));
#25846=CARTESIAN_POINT('Ctrl Pts',(-38.6803569266322,-4.58560283228258,
1.79778245415366));
#25847=CARTESIAN_POINT('Ctrl Pts',(-38.7199932596305,-4.2872252165181,2.55885409194545));
#25848=CARTESIAN_POINT('Ctrl Pts',(-38.7596295926288,-3.79529021528604,
3.2440416829727));
#25849=CARTESIAN_POINT('Ctrl Pts',(-38.7992659256272,-3.16956836399035,
3.77009435283018));
#25850=CARTESIAN_POINT('Ctrl Pts',(-38.8389022586255,-2.54384651269465,
4.29614702268767));
#25851=CARTESIAN_POINT('Ctrl Pts',(-38.8785385916238,-1.78433781133531,
4.66306477137538));
#25852=CARTESIAN_POINT('Ctrl Pts',(-38.9181749246221,-0.98332322946878,
4.82626673419433));
#25853=CARTESIAN_POINT('Ctrl Pts',(-38.9578112576204,-0.182308647602273,
4.98946869701328));
#25854=CARTESIAN_POINT('Ctrl Pts',(-38.9974475906188,0.660211814771426,
4.94895487396347));
#25855=CARTESIAN_POINT('Ctrl Pts',(-39.0370839236171,1.441871176594,4.70964780323818));
#25856=CARTESIAN_POINT('Ctrl Pts',(-39.0767202566154,2.22353053841658,4.47034073251288));
#25857=CARTESIAN_POINT('Ctrl Pts',(-39.1163565896137,2.94432879968803,4.03224041411209));
#25858=CARTESIAN_POINT('Ctrl Pts',(-39.155992922612,3.5166883529919,3.4485762746204));
#25859=CARTESIAN_POINT('Ctrl Pts',(-39.1956292556103,4.08904790629577,2.86491213512871));
#25860=CARTESIAN_POINT('Ctrl Pts',(-39.2352655886087,4.51296875163206,2.13568417454611));
#25861=CARTESIAN_POINT('Ctrl Pts',(-39.274901921607,4.73694410881552,1.3494945205605));
#25862=CARTESIAN_POINT('Ctrl Pts',(-39.3145382546053,4.96091946599899,0.563304866574897));
#25863=CARTESIAN_POINT('Ctrl Pts',(-39.3541745876036,4.98494933502962,-0.279846480813713));
#25864=CARTESIAN_POINT('Ctrl Pts',(-39.393810920602,4.80611411757365,-1.07751647545427));
#25865=CARTESIAN_POINT('Ctrl Pts',(-39.4334472536003,4.62727890011768,-1.87518647009483));
#25866=CARTESIAN_POINT('Ctrl Pts',(-39.4730835865986,4.2455785961751,-2.62737511198735));
#25867=CARTESIAN_POINT('Ctrl Pts',(-39.5127199195969,3.70739002379865,-3.242689661688));
#25868=CARTESIAN_POINT('Ctrl Pts',(-39.5523562525952,3.1692014514222,-3.85800421138865));
#25869=CARTESIAN_POINT('Ctrl Pts',(-39.5919925855936,2.47452461061189,-4.33644466889744));
#25870=CARTESIAN_POINT('Ctrl Pts',(-39.6316289185919,1.70776355261603,-4.61988241451491));
#25871=CARTESIAN_POINT('Ctrl Pts',(-39.6712652515902,0.941002494620145,
-4.90332016013239));
#25872=CARTESIAN_POINT('Ctrl Pts',(-39.7109015845885,0.102157219438717,
-4.99175519385855));
#25873=CARTESIAN_POINT('Ctrl Pts',(-39.7505379175868,-0.706852248500371,
-4.8744379618949));
#25874=CARTESIAN_POINT('Ctrl Pts',(-39.7901742505852,-1.51586171643944,
-4.75712072993124));
#25875=CARTESIAN_POINT('Ctrl Pts',(-39.8298105835835,-2.29503537713616,
-4.43405123227779));
#25876=CARTESIAN_POINT('Ctrl Pts',(-39.8694469165818,-2.94970212657891,
-3.94449191416061));
#25877=CARTESIAN_POINT('Ctrl Pts',(-39.9090832495801,-3.60436887602165,
-3.45493259604344));
#25878=CARTESIAN_POINT('Ctrl Pts',(-39.9487195825784,-4.13452871421041,
-2.79888345746255));
#25879=CARTESIAN_POINT('Ctrl Pts',(-39.9883559155767,-4.4757683951963,-2.05603664986182));
#25880=CARTESIAN_POINT('Ctrl Pts',(-40.0226234350833,-4.77078653991438,
-1.41380979525057));
#25881=CARTESIAN_POINT('Ctrl Pts',(-40.0568909545898,-4.92459753102333,
-0.706706582480056));
#25882=CARTESIAN_POINT('Ctrl Pts',(-40.0911584740964,-4.92524004259795,
0.000110578359120081));
#25883=CARTESIAN_POINT('Ctrl Pts',(-40.3088415259036,-4.92524227782323,
-0.000582878416294945));
#25884=CARTESIAN_POINT('Ctrl Pts',(-40.2753823854437,-4.92458215862047,
-0.690824814856074));
#25885=CARTESIAN_POINT('Ctrl Pts',(-40.2419232449839,-4.77809368542024,
-1.38044903752072));
#25886=CARTESIAN_POINT('Ctrl Pts',(-40.208464104524,-4.49640309152601,-2.01018594899038));
#25887=CARTESIAN_POINT('Ctrl Pts',(-40.1688277715257,-4.16270706620585,
-2.75618424964264));
#25888=CARTESIAN_POINT('Ctrl Pts',(-40.1291914385274,-3.63927891170889,
-3.41814136066434));
#25889=CARTESIAN_POINT('Ctrl Pts',(-40.0895551055291,-2.98962897640359,
-3.91446438086044));
#25890=CARTESIAN_POINT('Ctrl Pts',(-40.0499187725307,-2.33997904109829,
-4.41078740105654));
#25891=CARTESIAN_POINT('Ctrl Pts',(-40.0102824395324,-1.56410732498466,
-4.74147633042705));
#25892=CARTESIAN_POINT('Ctrl Pts',(-39.9706461065341,-0.756326330344129,
-4.86693605655279));
#25893=CARTESIAN_POINT('Ctrl Pts',(-39.9310097735357,0.0514546642963978,
-4.99239578267854));
#25894=CARTESIAN_POINT('Ctrl Pts',(-39.8913734405374,0.891144937463817,
-4.91262630555953));
#25895=CARTESIAN_POINT('Ctrl Pts',(-39.8517371075391,1.66074314480816,-4.63702697341363));
#25896=CARTESIAN_POINT('Ctrl Pts',(-39.8121007745408,2.43034135215252,-4.36142764126772));
#25897=CARTESIAN_POINT('Ctrl Pts',(-39.7724644415425,3.12984749367381,-3.8899984540949));
#25898=CARTESIAN_POINT('Ctrl Pts',(-39.7328281085442,3.6742600519052,-3.28016521191097));
#25899=CARTESIAN_POINT('Ctrl Pts',(-39.6931917755458,4.21867261013657,-2.67033196972706));
#25900=CARTESIAN_POINT('Ctrl Pts',(-39.6535554425475,4.60799158507806,-1.92209467253203));
#25901=CARTESIAN_POINT('Ctrl Pts',(-39.6139191095492,4.7949198484931,-1.12629124505432));
#25902=CARTESIAN_POINT('Ctrl Pts',(-39.5742827765509,4.98184811190814,-0.330487817576609));
#25903=CARTESIAN_POINT('Ctrl Pts',(-39.5346464435525,4.96638566379675,0.512881740183794));
#25904=CARTESIAN_POINT('Ctrl Pts',(-39.4950101105542,4.75040846378853,1.301310410167));
#25905=CARTESIAN_POINT('Ctrl Pts',(-39.4553737775559,4.53443126378031,2.08973908015021));
#25906=CARTESIAN_POINT('Ctrl Pts',(-39.4157374445576,4.11793931187527,2.82322686235623));
#25907=CARTESIAN_POINT('Ctrl Pts',(-39.3761011115593,3.55153811950529,3.41267283560264));
#25908=CARTESIAN_POINT('Ctrl Pts',(-39.3364647785609,2.98513692713531,4.00211880884906));
#25909=CARTESIAN_POINT('Ctrl Pts',(-39.2968284455626,2.26882649430039,4.44752297313588));
#25910=CARTESIAN_POINT('Ctrl Pts',(-39.2571921125643,1.48963847740388,4.69475906436197));
#25911=CARTESIAN_POINT('Ctrl Pts',(-39.217555779566,0.710450460507369,4.94199515558807));
#25912=CARTESIAN_POINT('Ctrl Pts',(-39.1779194465677,-0.131615140450732,
4.99106317375344));
#25913=CARTESIAN_POINT('Ctrl Pts',(-39.1382831135694,-0.934246271622569,
4.83600595769282));
#25914=CARTESIAN_POINT('Ctrl Pts',(-39.098646780571,-1.73687740279441,4.6809487416322));
#25915=CARTESIAN_POINT('Ctrl Pts',(-39.0590104475727,-2.50007406417998,
4.32176629134559));
#25916=CARTESIAN_POINT('Ctrl Pts',(-39.0193741145744,-3.13110736571771,
3.80209726021013));
#25917=CARTESIAN_POINT('Ctrl Pts',(-38.979737781576,-3.76214066725545,3.28242822907467));
#25918=CARTESIAN_POINT('Ctrl Pts',(-38.9401014485777,-4.26101060894535,
2.60227261709036));
#25919=CARTESIAN_POINT('Ctrl Pts',(-38.9004651155794,-4.56710396888216,
1.84427109478626));
#25920=CARTESIAN_POINT('Ctrl Pts',(-38.8699239190208,-4.80295972959322,
1.26020411045154));
#25921=CARTESIAN_POINT('Ctrl Pts',(-38.8393827224622,-4.92435926091217,
0.629918081833665));
#25922=CARTESIAN_POINT('Ctrl Pts',(-38.8088415259036,-4.92500387630964,
-0.000126728579282317));
#25923=CARTESIAN_POINT('Origin',(-41.25,0.,0.));
#25924=CARTESIAN_POINT('',(-37.0911584740964,-4.92470114822472,9.20081863105271E-5));
#25925=CARTESIAN_POINT('',(-37.3088415259036,-4.92466879478489,8.05726076643189E-5));
#25926=CARTESIAN_POINT('',(-41.25,-4.925,-6.03138548580071E-16));
#25927=CARTESIAN_POINT('Ctrl Pts',(-37.0911584740964,-4.92470114822472,
9.20081863105271E-5));
#25928=CARTESIAN_POINT('Ctrl Pts',(-37.1056189626302,-4.92490181486345,
0.29845508628429));
#25929=CARTESIAN_POINT('Ctrl Pts',(-37.1200794511639,-4.89822120621134,
0.596782699785559));
#25930=CARTESIAN_POINT('Ctrl Pts',(-37.1345399396977,-4.84432452014131,
0.890109556114513));
#25931=CARTESIAN_POINT('Ctrl Pts',(-37.174176272696,-4.69659320445376,1.69412118598857));
#25932=CARTESIAN_POINT('Ctrl Pts',(-37.2138126056943,-4.3443839128035,2.46056146826631));
#25933=CARTESIAN_POINT('Ctrl Pts',(-37.2534489386926,-3.83049038279097,
3.09630723696455));
#25934=CARTESIAN_POINT('Ctrl Pts',(-37.293085271691,-3.31659685277845,3.73205300566278));
#25935=CARTESIAN_POINT('Ctrl Pts',(-37.3327216046893,-2.64101908440367,
4.2371042607815));
#25936=CARTESIAN_POINT('Ctrl Pts',(-37.3723579376876,-1.88584036857968,
4.55009683221736));
#25937=CARTESIAN_POINT('Ctrl Pts',(-37.4119942706859,-1.13066165275566,
4.86308940365323));
#25938=CARTESIAN_POINT('Ctrl Pts',(-37.4516306036843,-0.295881989482435,
4.98402329140623));
#25939=CARTESIAN_POINT('Ctrl Pts',(-37.4912669366826,0.517072160578491,
4.89820492212251));
#25940=CARTESIAN_POINT('Ctrl Pts',(-37.5309032696809,1.33002631063939,4.81238655283879));
#25941=CARTESIAN_POINT('Ctrl Pts',(-37.5705396026792,2.12115494748799,4.51981592651836));
#25942=CARTESIAN_POINT('Ctrl Pts',(-37.6101759356775,2.79433524842529,4.05604063067722));
#25943=CARTESIAN_POINT('Ctrl Pts',(-37.6498122686759,3.46751554936259,3.59226533483608));
#25944=CARTESIAN_POINT('Ctrl Pts',(-37.6894486016742,4.0227475143886,2.95728536947423));
#25945=CARTESIAN_POINT('Ctrl Pts',(-37.7290849346725,4.39256997316809,2.22825135682294));
#25946=CARTESIAN_POINT('Ctrl Pts',(-37.7687212676708,4.76239243194758,1.49921734417164));
#25947=CARTESIAN_POINT('Ctrl Pts',(-37.8083576006691,4.94680538448055,0.676129284230918));
#25948=CARTESIAN_POINT('Ctrl Pts',(-37.8479939336675,4.92340249541402,-0.141006902314823));
#25949=CARTESIAN_POINT('Ctrl Pts',(-37.8876302666658,4.89999960634749,-0.958143088860554));
#25950=CARTESIAN_POINT('Ctrl Pts',(-37.9272665996641,4.66878087568145,-1.76932740201133));
#25951=CARTESIAN_POINT('Ctrl Pts',(-37.9669029326624,4.25783958183768,-2.4760002369688));
#25952=CARTESIAN_POINT('Ctrl Pts',(-38.0065392656607,3.84689828799389,-3.18267307192628));
#25953=CARTESIAN_POINT('Ctrl Pts',(-38.0461755986591,3.25623443097236,-3.78483442869049));
#25954=CARTESIAN_POINT('Ctrl Pts',(-38.0858119316574,2.55761418701446,-4.20932117440809));
#25955=CARTESIAN_POINT('Ctrl Pts',(-38.1254482646557,1.85899394305657,-4.63380792012569));
#25956=CARTESIAN_POINT('Ctrl Pts',(-38.165084597654,1.05241731216232,-4.88062005479668));
#25957=CARTESIAN_POINT('Ctrl Pts',(-38.2047209306523,0.235884061895514,
-4.91976968834123));
#25958=CARTESIAN_POINT('Ctrl Pts',(-38.2443572636507,-0.580649188371287,
-4.95891932188577));
#25959=CARTESIAN_POINT('Ctrl Pts',(-38.283993596649,-1.40713905801063,-4.79040645430388));
#25960=CARTESIAN_POINT('Ctrl Pts',(-38.3236299296473,-2.14316630365493,
-4.43470554552663));
#25961=CARTESIAN_POINT('Ctrl Pts',(-38.3632662626456,-2.87919354929924,
-4.07900463674938));
#25962=CARTESIAN_POINT('Ctrl Pts',(-38.4029025956439,-3.52475817094849,
-3.53611568677679));
#25963=CARTESIAN_POINT('Ctrl Pts',(-38.4425389286422,-4.00142350111364,
-2.87200018111494));
#25964=CARTESIAN_POINT('Ctrl Pts',(-38.4821752616406,-4.47808883127881,
-2.20788467545306));
#25965=CARTESIAN_POINT('Ctrl Pts',(-38.5218115946389,-4.78585486995985,
-1.42254261410192));
#25966=CARTESIAN_POINT('Ctrl Pts',(-38.5614479276372,-4.88732777415191,
-0.611393741148177));
#25967=CARTESIAN_POINT('Ctrl Pts',(-38.5713514431236,-4.9126817461795,-0.408720465963794));
#25968=CARTESIAN_POINT('Ctrl Pts',(-38.58125495861,-4.9251568823528,-0.204436077101899));
#25969=CARTESIAN_POINT('Ctrl Pts',(-38.5911584740964,-4.92495184350011,
-0.000126817359744069));
#25970=CARTESIAN_POINT('Ctrl Pts',(-38.8088415259036,-4.92500387630964,
-0.000126728579282317));
#25971=CARTESIAN_POINT('Ctrl Pts',(-38.7997463894639,-4.92519584210181,
-0.187753415138211));
#25972=CARTESIAN_POINT('Ctrl Pts',(-38.7906512530242,-4.91467875260689,
-0.37535870944927));
#25973=CARTESIAN_POINT('Ctrl Pts',(-38.7815561165845,-4.89328625908847,
-0.561715592844029));
#25974=CARTESIAN_POINT('Ctrl Pts',(-38.7419197835861,-4.80005841117423,
-1.37385332554627));
#25975=CARTESIAN_POINT('Ctrl Pts',(-38.7022834505878,-4.50028593716205,
-2.16228135832685));
#25976=CARTESIAN_POINT('Ctrl Pts',(-38.6626471175895,-4.03039143354269,
-2.83120470081615));
#25977=CARTESIAN_POINT('Ctrl Pts',(-38.6230107845912,-3.56049692992333,
-3.50012804330547));
#25978=CARTESIAN_POINT('Ctrl Pts',(-38.5833744515929,-2.92048039669678,
-4.04954669550349));
#25979=CARTESIAN_POINT('Ctrl Pts',(-38.5437381185945,-2.18810441447545,
-4.41270595677602));
#25980=CARTESIAN_POINT('Ctrl Pts',(-38.5041017855962,-1.45572843225415,
-4.77586521804853));
#25981=CARTESIAN_POINT('Ctrl Pts',(-38.4644654525979,-0.630993001038065,
-4.95276508839556));
#25982=CARTESIAN_POINT('Ctrl Pts',(-38.4248291195996,0.185895806989685,
-4.92191200479718));
#25983=CARTESIAN_POINT('Ctrl Pts',(-38.3851927866013,1.00278461501741,-4.89105892119881));
#25984=CARTESIAN_POINT('Ctrl Pts',(-38.3455564536029,1.81182679985681,-4.65245288365504));
#25985=CARTESIAN_POINT('Ctrl Pts',(-38.3059201206046,2.51472302428267,-4.23508477180253));
#25986=CARTESIAN_POINT('Ctrl Pts',(-38.2662837876063,3.21761924870857,-3.81771665994999));
#25987=CARTESIAN_POINT('Ctrl Pts',(-38.226647454608,3.81436951272092,-3.22158647378869));
#25988=CARTESIAN_POINT('Ctrl Pts',(-38.1870111216097,4.23246813764672,-2.5191245348344));
#25989=CARTESIAN_POINT('Ctrl Pts',(-38.1473747886113,4.6505667625725,-1.81666259588013));
#25990=CARTESIAN_POINT('Ctrl Pts',(-38.107738455613,4.89001374841174,-1.00786890413288));
#25991=CARTESIAN_POINT('Ctrl Pts',(-38.0681021226147,4.92171607585052,-0.191012611231857));
#25992=CARTESIAN_POINT('Ctrl Pts',(-38.0284657896164,4.95341840328931,0.625843681669167));
#25993=CARTESIAN_POINT('Ctrl Pts',(-37.988829456618,4.77737607232763,1.45076257572397));
#25994=CARTESIAN_POINT('Ctrl Pts',(-37.9491931236197,4.41497838080154,2.18351570702937));
#25995=CARTESIAN_POINT('Ctrl Pts',(-37.9095567906214,4.05258068927544,2.91626883833478));
#25996=CARTESIAN_POINT('Ctrl Pts',(-37.8699204576231,3.50382763718491,3.55685620689079));
#25997=CARTESIAN_POINT('Ctrl Pts',(-37.8302841246248,2.8353932010953,4.02744588369239));
#25998=CARTESIAN_POINT('Ctrl Pts',(-37.7906477916265,2.1669587650057,4.498035560494));
#25999=CARTESIAN_POINT('Ctrl Pts',(-37.7510114586281,1.37884294491701,4.79862754554121));
#26000=CARTESIAN_POINT('Ctrl Pts',(-37.7113751256298,0.566802503736936,
4.89269965039189));
#26001=CARTESIAN_POINT('Ctrl Pts',(-37.6717387926315,-0.245237937443135,
4.98677175524258));
#26002=CARTESIAN_POINT('Ctrl Pts',(-37.6321024596332,-1.08120299971459,
4.87432397989675));
#26003=CARTESIAN_POINT('Ctrl Pts',(-37.5924661266348,-1.83952219544158,
4.56901882701783));
#26004=CARTESIAN_POINT('Ctrl Pts',(-37.5528297936365,-2.59784139116857,
4.26371367413892));
#26005=CARTESIAN_POINT('Ctrl Pts',(-37.5131934606382,-3.2785147203511,3.76555114372692));
#26006=CARTESIAN_POINT('Ctrl Pts',(-37.4735571276399,-3.79883977695093,
3.13505842009503));
#26007=CARTESIAN_POINT('Ctrl Pts',(-37.4339207946416,-4.31916483355077,
2.50456569646312));
#26008=CARTESIAN_POINT('Ctrl Pts',(-37.3942844616432,-4.6791416175679,1.7417427796113));
#26009=CARTESIAN_POINT('Ctrl Pts',(-37.3546481286449,-4.83503263428287,
0.939273322303626));
#26010=CARTESIAN_POINT('Ctrl Pts',(-37.3393792610645,-4.89508559859979,
0.63014281112589));
#26011=CARTESIAN_POINT('Ctrl Pts',(-37.324110393484,-4.92485273578263,0.315128850619065));
#26012=CARTESIAN_POINT('Ctrl Pts',(-37.3088415259036,-4.92466879478489,
8.05726076643189E-5));
#26013=CARTESIAN_POINT('Origin',(-41.25,0.,0.));
#26014=CARTESIAN_POINT('',(-35.5911584740964,-4.92541600273781,-1.76250312958204E-5));
#26015=CARTESIAN_POINT('',(-35.8088415259036,-4.92542129650244,-7.54510851721086E-8));
#26016=CARTESIAN_POINT('',(-41.25,-4.925,-6.03138548580071E-16));
#26017=CARTESIAN_POINT('Ctrl Pts',(-35.5911584740964,-4.92541600273781,
-1.76250312958204E-5));
#26018=CARTESIAN_POINT('Ctrl Pts',(-35.6299829666503,-4.9252530757446,0.80071250682744));
#26019=CARTESIAN_POINT('Ctrl Pts',(-35.6688074592043,-4.72610527736418,
1.6015207460239));
#26020=CARTESIAN_POINT('Ctrl Pts',(-35.7076319517582,-4.35075868010393,
2.30882523934354));
#26021=CARTESIAN_POINT('Ctrl Pts',(-35.7472682847565,-3.96756338918973,
3.0309198395368));
#26022=CARTESIAN_POINT('Ctrl Pts',(-35.7869046177548,-3.4007234384037,3.65555938488601));
#26023=CARTESIAN_POINT('Ctrl Pts',(-35.8265409507531,-2.71911037852704,
4.1068496232168));
#26024=CARTESIAN_POINT('Ctrl Pts',(-35.8661772837514,-2.03749731865039,
4.55813986154758));
#26025=CARTESIAN_POINT('Ctrl Pts',(-35.9058136167498,-1.2411111496831,4.83608079285994));
#26026=CARTESIAN_POINT('Ctrl Pts',(-35.9454499497481,-0.426713489082491,
4.90690235042073));
#26027=CARTESIAN_POINT('Ctrl Pts',(-35.9850862827464,0.387684171518116,
4.97772390798152));
#26028=CARTESIAN_POINT('Ctrl Pts',(-36.0247226157447,1.22009332375204,4.84142609179075));
#26029=CARTESIAN_POINT('Ctrl Pts',(-36.064358948743,1.96937552612566,4.5145692059627));
#26030=CARTESIAN_POINT('Ctrl Pts',(-36.1039952817413,2.71865772849929,4.18771232013466));
#26031=CARTESIAN_POINT('Ctrl Pts',(-36.1436316147397,3.38481298101262,3.67029636466934));
#26032=CARTESIAN_POINT('Ctrl Pts',(-36.183267947738,3.88690283668777,3.02518783160286));
#26033=CARTESIAN_POINT('Ctrl Pts',(-36.2229042807363,4.38899269236293,2.38007929853637));
#26034=CARTESIAN_POINT('Ctrl Pts',(-36.2625406137347,4.7270171511999,1.6072781878687));
#26035=CARTESIAN_POINT('Ctrl Pts',(-36.302176946733,4.859905945216,0.800680511804564));
#26036=CARTESIAN_POINT('Ctrl Pts',(-36.3418132797313,4.99279473923209,-0.00591716425955069));
#26037=CARTESIAN_POINT('Ctrl Pts',(-36.3814496127296,4.92054786842731,-0.846311405720133));
#26038=CARTESIAN_POINT('Ctrl Pts',(-36.4210859457279,4.65194339091933,-1.61839357574463));
#26039=CARTESIAN_POINT('Ctrl Pts',(-36.4607222787262,4.38333891341134,-2.39047574576912));
#26040=CARTESIAN_POINT('Ctrl Pts',(-36.5003586117246,3.91837682920014,-3.09424584435753));
#26041=CARTESIAN_POINT('Ctrl Pts',(-36.5399949447229,3.31355043899555,-3.64419518776942));
#26042=CARTESIAN_POINT('Ctrl Pts',(-36.5796312777212,2.70872404879096,-4.1941445311813));
#26043=CARTESIAN_POINT('Ctrl Pts',(-36.6192676107195,1.96403335259296,-4.59027311941667));
#26044=CARTESIAN_POINT('Ctrl Pts',(-36.6589039437178,1.16995892261312,-4.78445098185022));
#26045=CARTESIAN_POINT('Ctrl Pts',(-36.6985402767162,0.375884492633281,
-4.97862884428377));
#26046=CARTESIAN_POINT('Ctrl Pts',(-36.7381766097145,-0.467573671128411,
-4.97085598091549));
#26047=CARTESIAN_POINT('Ctrl Pts',(-36.7778129427128,-1.25793466259469,
-4.76207680145668));
#26048=CARTESIAN_POINT('Ctrl Pts',(-36.8174492757111,-2.048295654061,-4.55329762199787));
#26049=CARTESIAN_POINT('Ctrl Pts',(-36.8570856087095,-2.78555947323189,
-4.1435121264485));
#26050=CARTESIAN_POINT('Ctrl Pts',(-36.8967219417078,-3.3801479199633,-3.58250961164066));
#26051=CARTESIAN_POINT('Ctrl Pts',(-36.9363582747061,-3.9747363666947,-3.02150709683283));
#26052=CARTESIAN_POINT('Ctrl Pts',(-36.9759946077044,-4.42664944098663,
-2.30928756276654));
#26053=CARTESIAN_POINT('Ctrl Pts',(-37.0156309407027,-4.68097930827017,
-1.53238630699822));
#26054=CARTESIAN_POINT('Ctrl Pts',(-37.0408067851673,-4.84252223358805,
-1.03892125359955));
#26055=CARTESIAN_POINT('Ctrl Pts',(-37.0659826296318,-4.92435178574819,
-0.51936087410214));
#26056=CARTESIAN_POINT('Ctrl Pts',(-37.0911584740964,-4.92470114822472,
9.20081863105271E-5));
#26057=CARTESIAN_POINT('Ctrl Pts',(-37.3088415259036,-4.92466879478489,
8.05726076643189E-5));
#26058=CARTESIAN_POINT('Ctrl Pts',(-37.2844740604857,-4.92437524479646,
-0.502702490966497));
#26059=CARTESIAN_POINT('Ctrl Pts',(-37.2601065950678,-4.84780014286267,
-1.00557295682021));
#26060=CARTESIAN_POINT('Ctrl Pts',(-37.23573912965,-4.69630408694853,-1.48475683918074));
#26061=CARTESIAN_POINT('Ctrl Pts',(-37.1961027966517,-4.44987927348641,
-2.26420154559395));
#26062=CARTESIAN_POINT('Ctrl Pts',(-37.1564664636533,-4.00522439714935,
-2.98097496065685));
#26063=CARTESIAN_POINT('Ctrl Pts',(-37.116830130655,-3.4163654150966,-3.54798848631869));
#26064=CARTESIAN_POINT('Ctrl Pts',(-37.0771937976567,-2.82750643304386,
-4.11500201198053));
#26065=CARTESIAN_POINT('Ctrl Pts',(-37.0375574646584,-2.09444334527543,
-4.53225564824131));
#26066=CARTESIAN_POINT('Ctrl Pts',(-36.99792113166,-1.30624395938722,-4.74905271260881));
#26067=CARTESIAN_POINT('Ctrl Pts',(-36.9582847986617,-0.518044573499021,
-4.96584977697631));
#26068=CARTESIAN_POINT('Ctrl Pts',(-36.9186484656634,0.325291110508953,
-4.98219026945052));
#26069=CARTESIAN_POINT('Ctrl Pts',(-36.8790121326651,1.12129706795617,-4.79608880588485));
#26070=CARTESIAN_POINT('Ctrl Pts',(-36.8393757996668,1.91730302540342,-4.60998734231918));
#26071=CARTESIAN_POINT('Ctrl Pts',(-36.7997394666684,2.66597925628991,-4.22144392271361));
#26072=CARTESIAN_POINT('Ctrl Pts',(-36.7601031336701,3.27636094244697,-3.67766691305279));
#26073=CARTESIAN_POINT('Ctrl Pts',(-36.7204668006718,3.88674262860402,-3.13388990339198));
#26074=CARTESIAN_POINT('Ctrl Pts',(-36.6808304676735,4.35882977003166,-2.43487930367593));
#26075=CARTESIAN_POINT('Ctrl Pts',(-36.6411941346751,4.63526336532393,-1.66556551436338));
#26076=CARTESIAN_POINT('Ctrl Pts',(-36.6015578016768,4.91169696061621,-0.896251725050832));
#26077=CARTESIAN_POINT('Ctrl Pts',(-36.5619214686785,4.99247700977312,-0.0566347461417782));
#26078=CARTESIAN_POINT('Ctrl Pts',(-36.5222851356802,4.86778866602909,0.751271223613593));
#26079=CARTESIAN_POINT('Ctrl Pts',(-36.4826488026819,4.74310032228506,1.55917719336896));
#26080=CARTESIAN_POINT('Ctrl Pts',(-36.4430124696835,4.4129435856401,2.33537215397065));
#26081=CARTESIAN_POINT('Ctrl Pts',(-36.4033761366852,3.9174327889355,2.98554773747212));
#26082=CARTESIAN_POINT('Ctrl Pts',(-36.3637398036869,3.4219219922309,3.63572332097359));
#26083=CARTESIAN_POINT('Ctrl Pts',(-36.3241034706886,2.76105713546667,4.15987952737483));
#26084=CARTESIAN_POINT('Ctrl Pts',(-36.2844671376903,2.01513387790084,4.49433091824439));
#26085=CARTESIAN_POINT('Ctrl Pts',(-36.244830804692,1.26921062033501,4.82878230911394));
#26086=CARTESIAN_POINT('Ctrl Pts',(-36.2051944716936,0.438228961967596,
4.97352888445181));
#26087=CARTESIAN_POINT('Ctrl Pts',(-36.1655581386953,-0.376846097463596,
4.91098380850294));
#26088=CARTESIAN_POINT('Ctrl Pts',(-36.125921805697,-1.19192115689479,4.84843873255408));
#26089=CARTESIAN_POINT('Ctrl Pts',(-36.0862854726987,-1.99108961738975,
4.57860200531848));
#26090=CARTESIAN_POINT('Ctrl Pts',(-36.0466491397003,-2.67725181063225,
4.13425902563176));
#26091=CARTESIAN_POINT('Ctrl Pts',(-36.007012806702,-3.36341400387475,3.68991604594505));
#26092=CARTESIAN_POINT('Ctrl Pts',(-35.9673764737037,-3.93656992986478,
3.07106681380722));
#26093=CARTESIAN_POINT('Ctrl Pts',(-35.9277401407054,-4.32708064129874,
2.35290205326299));
#26094=CARTESIAN_POINT('Ctrl Pts',(-35.8881072691048,-4.7175572498583,1.63480000926379));
#26095=CARTESIAN_POINT('Ctrl Pts',(-35.8484743975042,-4.92542054288352,
0.817399782334272));
#26096=CARTESIAN_POINT('Ctrl Pts',(-35.8088415259036,-4.92542129645401,
-7.54510764981203E-8));
#26097=CARTESIAN_POINT('Origin',(-41.25,0.,0.));
#26098=CARTESIAN_POINT('',(-34.0911584740964,-4.92464097398149,-6.78464643288912E-5));
#26099=CARTESIAN_POINT('',(-34.3088415259036,-4.92466853775765,-8.04693041996219E-5));
#26100=CARTESIAN_POINT('',(-41.25,-4.925,-6.03138548580071E-16));
#26101=CARTESIAN_POINT('Ctrl Pts',(-34.0911584740964,-4.92464097398149,
-6.78464643288912E-5));
#26102=CARTESIAN_POINT('Ctrl Pts',(-34.1147106376722,-4.92440379270329,
0.485900653683976));
#26103=CARTESIAN_POINT('Ctrl Pts',(-34.1382628012479,-4.85294370455535,
0.97193739581646));
#26104=CARTESIAN_POINT('Ctrl Pts',(-34.1618149648236,-4.71126926056628,
1.43656431557125));
#26105=CARTESIAN_POINT('Ctrl Pts',(-34.201451297822,-4.47284295118532,2.21849278902783));
#26106=CARTESIAN_POINT('Ctrl Pts',(-34.2410876308203,-4.03555490192482,
2.93978416801083));
#26107=CARTESIAN_POINT('Ctrl Pts',(-34.2807239638186,-3.45253599399545,
3.51280091785676));
#26108=CARTESIAN_POINT('Ctrl Pts',(-34.320360296817,-2.86951708606611,4.08581766770266));
#26109=CARTESIAN_POINT('Ctrl Pts',(-34.3599966298152,-2.1407673194679,4.51055978841149));
#26110=CARTESIAN_POINT('Ctrl Pts',(-34.3996329628136,-1.35483042949589,
4.73542074008651));
#26111=CARTESIAN_POINT('Ctrl Pts',(-34.4392692958119,-0.568893539523873,
4.96028169176152));
#26112=CARTESIAN_POINT('Ctrl Pts',(-34.4789056288102,0.274230473821956,
4.98526147440271));
#26113=CARTESIAN_POINT('Ctrl Pts',(-34.5185419618086,1.07210130403271,4.80732502252769));
#26114=CARTESIAN_POINT('Ctrl Pts',(-34.5581782948069,1.86997213424345,4.62938857065266));
#26115=CARTESIAN_POINT('Ctrl Pts',(-34.5978146278052,2.62258978131911,4.24853588426143));
#26116=CARTESIAN_POINT('Ctrl Pts',(-34.6374509608035,3.23851054156959,3.71104089851783));
#26117=CARTESIAN_POINT('Ctrl Pts',(-34.6770872938018,3.85443130182009,3.17354591277422));
#26118=CARTESIAN_POINT('Ctrl Pts',(-34.7167236268002,4.3336551752454,2.47940862767824));
#26119=CARTESIAN_POINT('Ctrl Pts',(-34.7563599597985,4.61795604124761,1.71296733168913));
#26120=CARTESIAN_POINT('Ctrl Pts',(-34.7959962927968,4.90225690724982,0.946526035699991));
#26121=CARTESIAN_POINT('Ctrl Pts',(-34.8356326257951,4.99163476582893,0.107780728817722));
#26122=CARTESIAN_POINT('Ctrl Pts',(-34.8752689587934,4.87523012883963,-0.701360299121477));
#26123=CARTESIAN_POINT('Ctrl Pts',(-34.9149052917917,4.75882549185033,-1.51050132706065));
#26124=CARTESIAN_POINT('Ctrl Pts',(-34.9545416247901,4.43663835929263,-2.29003807605676));
#26125=CARTESIAN_POINT('Ctrl Pts',(-34.9941779577884,3.94781475012695,-2.94525614794529));
#26126=CARTESIAN_POINT('Ctrl Pts',(-35.0338142907867,3.45899114096128,-3.60047421983382));
#26127=CARTESIAN_POINT('Ctrl Pts',(-35.073450623785,2.80353105518763,-4.13137361461476));
#26128=CARTESIAN_POINT('Ctrl Pts',(-35.1130869567833,2.0610734676521,-4.47344959055872));
#26129=CARTESIAN_POINT('Ctrl Pts',(-35.1527232897817,1.31861588011658,-4.81552556650267));
#26130=CARTESIAN_POINT('Ctrl Pts',(-35.19235962278,0.489160790819186,-4.96877812360963));
#26131=CARTESIAN_POINT('Ctrl Pts',(-35.2319959557783,-0.326512279982104,
-4.91458694188538));
#26132=CARTESIAN_POINT('Ctrl Pts',(-35.2716322887766,-1.14218535078339,
-4.86039576016113));
#26133=CARTESIAN_POINT('Ctrl Pts',(-35.3112686217749,-1.94407640308858,
-4.59876083960567));
#26134=CARTESIAN_POINT('Ctrl Pts',(-35.3509049547733,-2.63475497129048,
-4.16147105235511));
#26135=CARTESIAN_POINT('Ctrl Pts',(-35.3905412877716,-3.32543353949239,
-3.72418126510454));
#26136=CARTESIAN_POINT('Ctrl Pts',(-35.4301776207699,-3.90489962359101,
-3.11123661115887));
#26137=CARTESIAN_POINT('Ctrl Pts',(-35.4698139537682,-4.30274758654252,
-2.3971104031379));
#26138=CARTESIAN_POINT('Ctrl Pts',(-35.5094502867666,-4.70059554949403,
-1.68298419511693));
#26139=CARTESIAN_POINT('Ctrl Pts',(-35.5490866197649,-4.91682539129844,
-0.867676433020666));
#26140=CARTESIAN_POINT('Ctrl Pts',(-35.5887229527632,-4.92516499667947,
-0.0502477244538784));
#26141=CARTESIAN_POINT('Ctrl Pts',(-35.5895347932076,-4.92533581038564,
-0.0335049625525403));
#26142=CARTESIAN_POINT('Ctrl Pts',(-35.590346633652,-4.92541940962645,-0.0167613108681338));
#26143=CARTESIAN_POINT('Ctrl Pts',(-35.5911584740964,-4.92541600273781,
-1.76250312958204E-5));
#26144=CARTESIAN_POINT('Ctrl Pts',(-35.8088415259036,-4.92542129645401,
-7.54510764981203E-8));
#26145=CARTESIAN_POINT('Ctrl Pts',(-35.7692017315076,-4.92542205015613,
-0.817542710980693));
#26146=CARTESIAN_POINT('Ctrl Pts',(-35.7295619371115,-4.71748323020035,
-1.63508497704526));
#26147=CARTESIAN_POINT('Ctrl Pts',(-35.6899221427155,-4.32687593559207,
-2.35327847619989));
#26148=CARTESIAN_POINT('Ctrl Pts',(-35.6502858097172,-3.93630274931405,
-3.07140926177648));
#26149=CARTESIAN_POINT('Ctrl Pts',(-35.6106494767188,-3.36309298906717,
-3.69020863020926));
#26150=CARTESIAN_POINT('Ctrl Pts',(-35.5710131437205,-2.67689214306444,
-4.13449191593736));
#26151=CARTESIAN_POINT('Ctrl Pts',(-35.5313768107222,-1.99069129706169,
-4.57877520166546));
#26152=CARTESIAN_POINT('Ctrl Pts',(-35.4917404777239,-1.19149936530308,
-4.84854240468886));
#26153=CARTESIAN_POINT('Ctrl Pts',(-35.4521041447255,-0.376418867883944,
-4.91101657342473));
#26154=CARTESIAN_POINT('Ctrl Pts',(-35.4124678117272,0.438661629535188,
-4.9734907421606));
#26155=CARTESIAN_POINT('Ctrl Pts',(-35.3728314787289,1.26963069261483,-4.82867187660894));
#26156=CARTESIAN_POINT('Ctrl Pts',(-35.3331951457306,2.01552485195566,-4.49415559584896));
#26157=CARTESIAN_POINT('Ctrl Pts',(-35.2935588127323,2.76141901129648,-4.159639315089));
#26158=CARTESIAN_POINT('Ctrl Pts',(-35.2539224797339,3.42223826689847,-3.63542561912073));
#26159=CARTESIAN_POINT('Ctrl Pts',(-35.2142861467356,3.91769250008482,-2.98520693140871));
#26160=CARTESIAN_POINT('Ctrl Pts',(-35.1746498137373,4.41314673327116,-2.33498824369668));
#26161=CARTESIAN_POINT('Ctrl Pts',(-35.135013480739,4.74323594404185,-1.5587645642409));
#26162=CARTESIAN_POINT('Ctrl Pts',(-35.0953771477407,4.86785400400843,-0.750847750353243));
#26163=CARTESIAN_POINT('Ctrl Pts',(-35.0557408147424,4.99247206397501,0.0570690635343918));
#26164=CARTESIAN_POINT('Ctrl Pts',(-35.016104481744,4.9116189731375,0.896679011853955));
#26165=CARTESIAN_POINT('Ctrl Pts',(-34.9764681487457,4.63511845288976,1.66596875007676));
#26166=CARTESIAN_POINT('Ctrl Pts',(-34.9368318157474,4.35861793264201,2.43525848829959));
#26167=CARTESIAN_POINT('Ctrl Pts',(-34.897195482749,3.88646998298403,3.1342280164257));
#26168=CARTESIAN_POINT('Ctrl Pts',(-34.8575591497507,3.27604099357486,3.6779519242329));
#26169=CARTESIAN_POINT('Ctrl Pts',(-34.8179228167524,2.66561200416568,4.22167583204011));
#26170=CARTESIAN_POINT('Ctrl Pts',(-34.7782864837541,1.91690197500532,4.61015411952837));
#26171=CARTESIAN_POINT('Ctrl Pts',(-34.7386501507558,1.12087983078267,4.79618633431772));
#26172=CARTESIAN_POINT('Ctrl Pts',(-34.6990138177574,0.324857686560062,
4.98221854910706));
#26173=CARTESIAN_POINT('Ctrl Pts',(-34.6593774847591,-0.518476572724812,
4.96580469119751));
#26174=CARTESIAN_POINT('Ctrl Pts',(-34.6197411517608,-1.30665709549724,
4.74893905870966));
#26175=CARTESIAN_POINT('Ctrl Pts',(-34.5801048187625,-2.0948376182697,4.5320734262218));
#26176=CARTESIAN_POINT('Ctrl Pts',(-34.5404684857642,-2.8278644045297,4.11475601915564));
#26177=CARTESIAN_POINT('Ctrl Pts',(-34.5008321527658,-3.41667405734504,
3.54769126819355));
#26178=CARTESIAN_POINT('Ctrl Pts',(-34.4611958197675,-4.00548371016042,
2.98062651723144));
#26179=CARTESIAN_POINT('Ctrl Pts',(-34.4215594867692,-4.45007622953113,
2.26381442237339));
#26180=CARTESIAN_POINT('Ctrl Pts',(-34.3819231537709,-4.69643323472671,
1.48434828133623));
#26181=CARTESIAN_POINT('Ctrl Pts',(-34.3575626111485,-4.84784457557038,
1.00528736133934));
#26182=CARTESIAN_POINT('Ctrl Pts',(-34.333202068526,-4.92437546731788,0.502559828752335));
#26183=CARTESIAN_POINT('Ctrl Pts',(-34.3088415259036,-4.92466853775765,
-8.04693041996219E-5));
#26184=CARTESIAN_POINT('Origin',(-41.25,0.,0.));
#26185=CARTESIAN_POINT('',(-32.5911584740964,-4.92505699337764,0.000124540890476602));
#26186=CARTESIAN_POINT('',(-32.8088415259036,-4.92500432546286,0.000126715614278523));
#26187=CARTESIAN_POINT('',(-41.25,-4.925,-6.03138548580071E-16));
#26188=CARTESIAN_POINT('Ctrl Pts',(-32.5911584740964,-4.92505699337764,
0.000124540890476602));
#26189=CARTESIAN_POINT('Ctrl Pts',(-32.599438308694,-4.92523260524548,0.170926811184958));
#26190=CARTESIAN_POINT('Ctrl Pts',(-32.6077181432915,-4.9165200525162,0.341711253364765));
#26191=CARTESIAN_POINT('Ctrl Pts',(-32.6159979778891,-4.89878435312716,
0.51155345732391));
#26192=CARTESIAN_POINT('Ctrl Pts',(-32.6556343108875,-4.81388192196659,
1.32460377541339));
#26193=CARTESIAN_POINT('Ctrl Pts',(-32.6952706438858,-4.52220277615496,
2.11606152374493));
#26194=CARTESIAN_POINT('Ctrl Pts',(-32.7349069768841,-4.05918618745925,
2.78976389216296));
#26195=CARTESIAN_POINT('Ctrl Pts',(-32.7745433098825,-3.59616959876357,
3.46346626058094));
#26196=CARTESIAN_POINT('Ctrl Pts',(-32.8141796428808,-2.96181556718383,
4.01941324908544));
#26197=CARTESIAN_POINT('Ctrl Pts',(-32.8538159758791,-2.23319866351874,
4.39005681142113));
#26198=CARTESIAN_POINT('Ctrl Pts',(-32.8934523088774,-1.50458175985363,
4.76070037375683));
#26199=CARTESIAN_POINT('Ctrl Pts',(-32.9330886418757,-0.681701984103161,
4.94604050992373));
#26200=CARTESIAN_POINT('Ctrl Pts',(-32.972724974874,0.135460049849992,4.92355823091998));
#26201=CARTESIAN_POINT('Ctrl Pts',(-33.0123613078724,0.952622083803168,
4.90107595191623));
#26202=CARTESIAN_POINT('Ctrl Pts',(-33.0519976408707,1.76406637595904,4.67077125774183));
#26203=CARTESIAN_POINT('Ctrl Pts',(-33.091633973869,2.4712017336879,4.26062637058644));
#26204=CARTESIAN_POINT('Ctrl Pts',(-33.1312703068673,3.17833709141674,3.85048148343106));
#26205=CARTESIAN_POINT('Ctrl Pts',(-33.1709066398656,3.78116351471858,3.26049640329468));
#26206=CARTESIAN_POINT('Ctrl Pts',(-33.210542972864,4.20643706486838,2.56235483445041));
#26207=CARTESIAN_POINT('Ctrl Pts',(-33.2501793058623,4.63171061501819,1.86421326560614));
#26208=CARTESIAN_POINT('Ctrl Pts',(-33.2898156388606,4.87943129201598,1.05791520805396));
#26209=CARTESIAN_POINT('Ctrl Pts',(-33.3294519718589,4.91950081650975,0.241426582404654));
#26210=CARTESIAN_POINT('Ctrl Pts',(-33.3690883048572,4.95957034100353,-0.575062043244695));
#26211=CARTESIAN_POINT('Ctrl Pts',(-33.4087246378556,4.7919887129933,-1.40174123699112));
#26212=CARTESIAN_POINT('Ctrl Pts',(-33.4483609708539,4.43711724714662,-2.13816875232085));
#26213=CARTESIAN_POINT('Ctrl Pts',(-33.4879973038522,4.08224578129997,-2.87459626765054));
#26214=CARTESIAN_POINT('Ctrl Pts',(-33.5276336368505,3.54008447761688,-3.5207721045635));
#26215=CARTESIAN_POINT('Ctrl Pts',(-33.5672699698489,2.87650640962745,-3.99818533258564));
#26216=CARTESIAN_POINT('Ctrl Pts',(-33.6069063028472,2.21292834163802,-4.47559856060777));
#26217=CARTESIAN_POINT('Ctrl Pts',(-33.6465426358455,1.42793350934223,-4.78424917973909));
#26218=CARTESIAN_POINT('Ctrl Pts',(-33.6861789688438,0.616899472809076,
-4.88663586926392));
#26219=CARTESIAN_POINT('Ctrl Pts',(-33.7258153018421,-0.194134563724077,
-4.98902255878875));
#26220=CARTESIAN_POINT('Ctrl Pts',(-33.7654516348405,-1.0312078044946,-4.8851453187071));
#26221=CARTESIAN_POINT('Ctrl Pts',(-33.8050879678388,-1.79261511716435,
-4.5876253247234));
#26222=CARTESIAN_POINT('Ctrl Pts',(-33.8447243008371,-2.5540224298341,-4.29010533073969));
#26223=CARTESIAN_POINT('Ctrl Pts',(-33.8843606338354,-3.23976381440308,
-3.79894258285393));
#26224=CARTESIAN_POINT('Ctrl Pts',(-33.9239969668337,-3.76652109168392,
-3.17381378537394));
#26225=CARTESIAN_POINT('Ctrl Pts',(-33.963633299832,-4.29327836896475,-2.54868498789394));
#26226=CARTESIAN_POINT('Ctrl Pts',(-34.0032696328304,-4.66105153895743,
-1.7895901408197));
#26227=CARTESIAN_POINT('Ctrl Pts',(-34.0429059658287,-4.82515583920305,
-0.988759933317539));
#26228=CARTESIAN_POINT('Ctrl Pts',(-34.0589901352513,-4.89174831051554,
-0.663788177309668));
#26229=CARTESIAN_POINT('Ctrl Pts',(-34.0750743046738,-4.92480294907351,
-0.331943925079275));
#26230=CARTESIAN_POINT('Ctrl Pts',(-34.0911584740964,-4.92464097398149,
-6.78464643288912E-5));
#26231=CARTESIAN_POINT('Ctrl Pts',(-34.3088415259036,-4.92466853775765,
-8.04693041996219E-5));
#26232=CARTESIAN_POINT('Ctrl Pts',(-34.2935657355277,-4.92485231373804,
-0.315271635058983));
#26233=CARTESIAN_POINT('Ctrl Pts',(-34.2782899451518,-4.89505800095221,
-0.630428498620279));
#26234=CARTESIAN_POINT('Ctrl Pts',(-34.2630141547759,-4.834950904457,-0.939693939557906));
#26235=CARTESIAN_POINT('Ctrl Pts',(-34.2233778217776,-4.67899007797124,
-1.74214983219882));
#26236=CARTESIAN_POINT('Ctrl Pts',(-34.1837414887793,-4.31894693397922,
-2.50494143026443));
#26237=CARTESIAN_POINT('Ctrl Pts',(-34.144105155781,-3.79856703000646,-3.13538888610318));
#26238=CARTESIAN_POINT('Ctrl Pts',(-34.1044688227826,-3.27818712603374,
-3.76583634194189));
#26239=CARTESIAN_POINT('Ctrl Pts',(-34.0648324897843,-2.59747046208028,
-4.26393965555378));
#26240=CARTESIAN_POINT('Ctrl Pts',(-34.025196156786,-1.83912470937512,-4.56917883781291));
#26241=CARTESIAN_POINT('Ctrl Pts',(-33.9855598237877,-1.0807789566699,-4.87441802007206));
#26242=CARTESIAN_POINT('Ctrl Pts',(-33.9459234907894,-0.24480411521302,
-4.98679307097843));
#26243=CARTESIAN_POINT('Ctrl Pts',(-33.906287157791,0.567228139136565,-4.89265032336495));
#26244=CARTESIAN_POINT('Ctrl Pts',(-33.8666508247927,1.3792603934861,-4.79850757575147));
#26245=CARTESIAN_POINT('Ctrl Pts',(-33.8270144917944,2.16735006072829,-4.49784702961813));
#26246=CARTESIAN_POINT('Ctrl Pts',(-33.7873781587961,2.83574355563621,-4.02719920480961));
#26247=CARTESIAN_POINT('Ctrl Pts',(-33.7477418257978,3.50413705054412,-3.55655138000108));
#26248=CARTESIAN_POINT('Ctrl Pts',(-33.7081054927994,4.05283437311776,-2.91591627651736));
#26249=CARTESIAN_POINT('Ctrl Pts',(-33.6684691598011,4.41516831780336,-2.18313162086415));
#26250=CARTESIAN_POINT('Ctrl Pts',(-33.6288328268028,4.77750226248896,-1.45034696521094));
#26251=CARTESIAN_POINT('Ctrl Pts',(-33.5891964938045,4.95347282928651,-0.625412757388233));
#26252=CARTESIAN_POINT('Ctrl Pts',(-33.5495601608062,4.92169944011505,0.191440773407072));
#26253=CARTESIAN_POINT('Ctrl Pts',(-33.5099238278078,4.88992605094358,1.00829430420238));
#26254=CARTESIAN_POINT('Ctrl Pts',(-33.4702874948095,4.65040870580311,1.8170671579703));
#26255=CARTESIAN_POINT('Ctrl Pts',(-33.4306511618112,4.23224897203365,2.519492724195));
#26256=CARTESIAN_POINT('Ctrl Pts',(-33.3910148288129,3.81408923826417,3.22191829041972));
#26257=CARTESIAN_POINT('Ctrl Pts',(-33.3513784958145,3.21728711586574,3.81799656910118));
#26258=CARTESIAN_POINT('Ctrl Pts',(-33.3117421628162,2.51435458572833,4.23530352699527));
#26259=CARTESIAN_POINT('Ctrl Pts',(-33.2721058298179,1.81142205559096,4.65261048488934));
#26260=CARTESIAN_POINT('Ctrl Pts',(-33.2324694968196,1.00235911771458,4.89114612199604));
#26261=CARTESIAN_POINT('Ctrl Pts',(-33.1928331638213,0.185467628088543,
4.921928149362));
#26262=CARTESIAN_POINT('Ctrl Pts',(-33.153196830823,-0.631423861537568,
4.95271017672796));
#26263=CARTESIAN_POINT('Ctrl Pts',(-33.1135604978246,-1.45614390291336,
4.77573859435319));
#26264=CARTESIAN_POINT('Ctrl Pts',(-33.0739241648263,-2.1884882882529,4.412515604588));
#26265=CARTESIAN_POINT('Ctrl Pts',(-33.034287831828,-2.9208326735924,4.04929261482283));
#26266=CARTESIAN_POINT('Ctrl Pts',(-32.9946514988297,-3.5608014028956,3.49981821766725));
#26267=CARTESIAN_POINT('Ctrl Pts',(-32.9550151658314,-4.03063771470406,
2.83085403391884));
#26268=CARTESIAN_POINT('Ctrl Pts',(-32.915378832833,-4.50047402651251,2.16188985017043));
#26269=CARTESIAN_POINT('Ctrl Pts',(-32.8757424998347,-4.80017792082623,
1.37343587982916));
#26270=CARTESIAN_POINT('Ctrl Pts',(-32.8361061668364,-4.89333511183429,
0.561289971265626));
#26271=CARTESIAN_POINT('Ctrl Pts',(-32.8270179531921,-4.91469512146023,
0.375073059432364));
#26272=CARTESIAN_POINT('Ctrl Pts',(-32.8179297395479,-4.92519616725995,
0.187610570225986));
#26273=CARTESIAN_POINT('Ctrl Pts',(-32.8088415259036,-4.92500432546286,
0.000126715614278523));
#26274=CARTESIAN_POINT('Origin',(-41.25,0.,0.));
#26275=CARTESIAN_POINT('',(-31.0911584740964,-4.92514031288301,-0.000116505347877993));
#26276=CARTESIAN_POINT('',(-31.3088415259036,-4.9251906134473,-0.000109311167407344));
#26277=CARTESIAN_POINT('',(-41.25,-4.925,-6.03138548580071E-16));
#26278=CARTESIAN_POINT('Ctrl Pts',(-31.0911584740964,-4.92514031288301,
-0.000116505347877993));
#26279=CARTESIAN_POINT('Ctrl Pts',(-31.1238023127141,-4.92446467357143,
0.673250866068188));
#26280=CARTESIAN_POINT('Ctrl Pts',(-31.1564461513319,-4.78528366208081,
1.34688857869454));
#26281=CARTESIAN_POINT('Ctrl Pts',(-31.1890899899496,-4.51678499905435,
1.9642879928124));
#26282=CARTESIAN_POINT('Ctrl Pts',(-31.2287263229479,-4.19077240776744,
2.71393784427457));
#26283=CARTESIAN_POINT('Ctrl Pts',(-31.2683626559462,-3.67410740557199,
3.38067583437288));
#26284=CARTESIAN_POINT('Ctrl Pts',(-31.3079989889446,-3.02956497379938,
3.8834922164745));
#26285=CARTESIAN_POINT('Ctrl Pts',(-31.3476353219429,-2.38502254202674,
4.38630859857615));
#26286=CARTESIAN_POINT('Ctrl Pts',(-31.3872716549412,-1.61260268067694,
4.72520337268107));
#26287=CARTESIAN_POINT('Ctrl Pts',(-31.4269079879395,-0.806155214751121,
4.85900077557536));
#26288=CARTESIAN_POINT('Ctrl Pts',(-31.4665443209379,0.000292251174648372,
4.99279817846964));
#26289=CARTESIAN_POINT('Ctrl Pts',(-31.5061806539362,0.840767321676489,
4.9214982101533));
#26290=CARTESIAN_POINT('Ctrl Pts',(-31.5458169869345,1.61315160673935,4.65376375455655));
#26291=CARTESIAN_POINT('Ctrl Pts',(-31.5854533199328,2.38553589180226,4.38602929895978));
#26292=CARTESIAN_POINT('Ctrl Pts',(-31.6250896529312,3.0898293914262,3.92186035608262));
#26293=CARTESIAN_POINT('Ctrl Pts',(-31.6647259859295,3.64045979429983,3.3176539217641));
#26294=CARTESIAN_POINT('Ctrl Pts',(-31.7043623189278,4.19109019717344,2.71344748744561));
#26295=CARTESIAN_POINT('Ctrl Pts',(-31.7439986519261,4.58805750329668,1.96920356168581));
#26296=CARTESIAN_POINT('Ctrl Pts',(-31.7836349849244,4.78312985406825,1.17534840237615));
#26297=CARTESIAN_POINT('Ctrl Pts',(-31.8232713179227,4.97820220483983,0.381493243066466));
#26298=CARTESIAN_POINT('Ctrl Pts',(-31.8629076509211,4.97137960025971,-0.461973149793131));
#26299=CARTESIAN_POINT('Ctrl Pts',(-31.9025439839194,4.76349098425275,-1.25256885458638));
#26300=CARTESIAN_POINT('Ctrl Pts',(-31.9421803169177,4.55560236824579,-2.0431645593796));
#26301=CARTESIAN_POINT('Ctrl Pts',(-31.981816649916,4.14664774081201,-2.78088957610653));
#26302=CARTESIAN_POINT('Ctrl Pts',(-32.0214529829143,3.58631545184477,-3.37610967658211));
#26303=CARTESIAN_POINT('Ctrl Pts',(-32.0610893159127,3.02598316287755,-3.97132977705768));
#26304=CARTESIAN_POINT('Ctrl Pts',(-32.100725648911,2.31427321237688,-4.42404496128188));
#26305=CARTESIAN_POINT('Ctrl Pts',(-32.1403619819093,1.53765898091128,-4.67924993368397));
#26306=CARTESIAN_POINT('Ctrl Pts',(-32.1799983149076,0.761044749445631,
-4.93445490608606));
#26307=CARTESIAN_POINT('Ctrl Pts',(-32.219634647906,-0.0804737629849417,
-4.992149666666));
#26308=CARTESIAN_POINT('Ctrl Pts',(-32.2592709809043,-0.884651318568558,
-4.8453242534271));
#26309=CARTESIAN_POINT('Ctrl Pts',(-32.2989073139026,-1.68882887415215,
-4.6984988401882));
#26310=CARTESIAN_POINT('Ctrl Pts',(-32.3385436469009,-2.45566547288878,
-4.34715325313046));
#26311=CARTESIAN_POINT('Ctrl Pts',(-32.3781799798992,-3.09198979653732,
-3.83397628799953));
#26312=CARTESIAN_POINT('Ctrl Pts',(-32.4178163128975,-3.72831412018587,
-3.32079932286859));
#26313=CARTESIAN_POINT('Ctrl Pts',(-32.4574526458959,-4.23412616874633,
-2.64579097966446));
#26314=CARTESIAN_POINT('Ctrl Pts',(-32.4970889788942,-4.54796933477179,
-1.8909653641387));
#26315=CARTESIAN_POINT('Ctrl Pts',(-32.5284454772949,-4.79625221033389,
-1.29381909919356));
#26316=CARTESIAN_POINT('Ctrl Pts',(-32.5598019756957,-4.92439193501344,
-0.646719433129764));
#26317=CARTESIAN_POINT('Ctrl Pts',(-32.5911584740964,-4.92505699337764,
0.000124540890476602));
#26318=CARTESIAN_POINT('Ctrl Pts',(-32.8088415259036,-4.92500432546286,
0.000126715614278523));
#26319=CARTESIAN_POINT('Ctrl Pts',(-32.7782934065495,-4.92435948959698,
-0.630060842889056));
#26320=CARTESIAN_POINT('Ctrl Pts',(-32.7477452871955,-4.80290353570356,
-1.26048979348428));
#26321=CARTESIAN_POINT('Ctrl Pts',(-32.7171971678414,-4.56694350005811,
-1.84466853820109));
#26322=CARTESIAN_POINT('Ctrl Pts',(-32.6775608348431,-4.26078420957148,
-2.60264329231841));
#26323=CARTESIAN_POINT('Ctrl Pts',(-32.6379245018448,-3.76185514089583,
-3.28275495376725));
#26324=CARTESIAN_POINT('Ctrl Pts',(-32.5982881688465,-3.13077661311804,
-3.80236935966164));
#26325=CARTESIAN_POINT('Ctrl Pts',(-32.5586518358481,-2.49969808534025,
-4.32198376555603));
#26326=CARTESIAN_POINT('Ctrl Pts',(-32.5190155028498,-1.73647009846033,
-4.68110091589597));
#26327=CARTESIAN_POINT('Ctrl Pts',(-32.4793791698515,-0.933825521759056,
-4.83608776217916));
#26328=CARTESIAN_POINT('Ctrl Pts',(-32.4397428368532,-0.131180945057805,
-4.99107460846236));
#26329=CARTESIAN_POINT('Ctrl Pts',(-32.4001065038549,0.710880221464788,
-4.94193115068882));
#26330=CARTESIAN_POINT('Ctrl Pts',(-32.3604701708565,1.49004680813205,-4.69462836207976));
#26331=CARTESIAN_POINT('Ctrl Pts',(-32.3208338378582,2.26921339479935,-4.44732557347068));
#26332=CARTESIAN_POINT('Ctrl Pts',(-32.2811975048599,2.98548540161131,-4.00186345402606));
#26333=CARTESIAN_POINT('Ctrl Pts',(-32.2415611718616,3.55183515199862,-3.4123660415797));
#26334=CARTESIAN_POINT('Ctrl Pts',(-32.2019248388633,4.11818490238593,-2.82286862913336));
#26335=CARTESIAN_POINT('Ctrl Pts',(-32.1622885058649,4.53461239634859,-2.08933592368529));
#26336=CARTESIAN_POINT('Ctrl Pts',(-32.1226521728666,4.75052132847285,-1.30089279192747));
#26337=CARTESIAN_POINT('Ctrl Pts',(-32.0830158398683,4.96643026059711,-0.512449660169646));
#26338=CARTESIAN_POINT('Ctrl Pts',(-32.04337950687,4.98182063088296,0.330903897897914));
#26339=CARTESIAN_POINT('Ctrl Pts',(-32.0037431738717,4.79482249575999,1.12669968615089));
#26340=CARTESIAN_POINT('Ctrl Pts',(-31.9641068408733,4.60782436063702,1.92249547440389));
#26341=CARTESIAN_POINT('Ctrl Pts',(-31.924470507875,4.21843772010518,2.67073349284236));
#26342=CARTESIAN_POINT('Ctrl Pts',(-31.8848341748767,3.67397339242095,3.28050216595624));
#26343=CARTESIAN_POINT('Ctrl Pts',(-31.8451978418784,3.12950906473676,3.89027083907008));
#26344=CARTESIAN_POINT('Ctrl Pts',(-31.8055615088801,2.42996704990017,4.36157016685941));
#26345=CARTESIAN_POINT('Ctrl Pts',(-31.7659251758817,1.66034231540023,4.63713686903792));
#26346=CARTESIAN_POINT('Ctrl Pts',(-31.7262888428834,0.890717580900255,
4.91270357121643));
#26347=CARTESIAN_POINT('Ctrl Pts',(-31.6866525098851,0.0510101267369292,
4.99253764778412));
#26348=CARTESIAN_POINT('Ctrl Pts',(-31.6470161768868,-0.756754854777219,
4.86693918633553));
#26349=CARTESIAN_POINT('Ctrl Pts',(-31.6073798438884,-1.56451983629139,
4.74134072488694));
#26350=CARTESIAN_POINT('Ctrl Pts',(-31.5677435108901,-2.34034234515637,
4.41030972542208));
#26351=CARTESIAN_POINT('Ctrl Pts',(-31.5281071778918,-2.98995926811177,
3.91406674874667));
#26352=CARTESIAN_POINT('Ctrl Pts',(-31.4884708448935,-3.63957619106713,
3.41782377207128));
#26353=CARTESIAN_POINT('Ctrl Pts',(-31.4488345118952,-4.16298752811293,
2.75636881818537));
#26354=CARTESIAN_POINT('Ctrl Pts',(-31.4091981788969,-4.49659834015827,
2.01006923515549));
#26355=CARTESIAN_POINT('Ctrl Pts',(-31.3757459612324,-4.77815873325062,
1.38020834223579));
#26356=CARTESIAN_POINT('Ctrl Pts',(-31.342293743568,-4.92452422896182,0.689912627386944));
#26357=CARTESIAN_POINT('Ctrl Pts',(-31.3088415259036,-4.9251906134473,-0.000109311167407344));
#26358=CARTESIAN_POINT('Origin',(-55.3478126690739,0.,0.));
#26359=CARTESIAN_POINT('',(-30.5978126690739,-4.07061596824169,-9.62913744964106E-5));
#26360=CARTESIAN_POINT('',(-30.3021873309261,-4.0701702520628,4.41716588962804E-5));
#26361=CARTESIAN_POINT('',(-55.3478126690739,-4.0705,-3.42898509504556E-13));
#26362=CARTESIAN_POINT('',(-30.,3.27123863458584,-2.42269058837956));
#26363=CARTESIAN_POINT('Ctrl Pts',(-30.5978126690739,-4.07061596824169,
-9.62913744964253E-5));
#26364=CARTESIAN_POINT('Ctrl Pts',(-30.5908201746933,-4.07073558370832,
-0.119309532774532));
#26365=CARTESIAN_POINT('Ctrl Pts',(-30.5441913473144,-4.03650708564677,
-0.914204073344773));
#26366=CARTESIAN_POINT('Ctrl Pts',(-30.4579261869372,-3.53493172767287,
-2.34618303071339));
#26367=CARTESIAN_POINT('Ctrl Pts',(-30.3390171879422,-1.98456278272466,
-3.74990799775467));
#26368=CARTESIAN_POINT('Ctrl Pts',(-30.2201081889473,0.0480654627907762,
-4.24241178043034));
#26369=CARTESIAN_POINT('Ctrl Pts',(-30.1071024596332,1.96866978992971,-3.73070684879719));
#26370=CARTESIAN_POINT('Ctrl Pts',(-30.0337330633174,2.92852673884923,-2.88450283314551));
#26371=CARTESIAN_POINT('Ctrl Pts',(-30.,3.27123863458584,-2.42269058837956));
#26372=CARTESIAN_POINT('',(-30.,-1.22233170237264,-3.88263769354994));
#26373=CARTESIAN_POINT('Origin',(-30.,0.,0.));
#26374=CARTESIAN_POINT('Ctrl Pts',(-30.3021873309261,-4.0701702520628,4.41716588963498E-5));
#26375=CARTESIAN_POINT('Ctrl Pts',(-30.280730886614,-4.07009405811129,-0.365864875771756));
#26376=CARTESIAN_POINT('Ctrl Pts',(-30.2196381093036,-3.93089507694675,
-1.40778857362903));
#26377=CARTESIAN_POINT('Ctrl Pts',(-30.118908998995,-3.05253333388674,-2.94673281729211));
#26378=CARTESIAN_POINT('Ctrl Pts',(-30.0396363329983,-1.86695937376294,
-3.67969605923881));
#26379=CARTESIAN_POINT('Ctrl Pts',(-30.,-1.22233170237264,-3.88263769354994));
#26380=CARTESIAN_POINT('Origin',(-55.3478126690739,0.,0.));
#26381=CARTESIAN_POINT('',(-32.0978126690739,-4.07054710488196,0.0001029327297676));
#26382=CARTESIAN_POINT('',(-31.8021873309261,-4.07065754153041,-9.03454027129102E-5));
#26383=CARTESIAN_POINT('',(-55.3478126690739,-4.0705,-3.42898509504556E-13));
#26384=CARTESIAN_POINT('Ctrl Pts',(-32.0978126690739,-4.07054710488196,
0.000102932729767729));
#26385=CARTESIAN_POINT('Ctrl Pts',(-32.0664561706731,-4.0699974358319,-0.534511970061966));
#26386=CARTESIAN_POINT('Ctrl Pts',(-31.9954633392741,-3.83021782586463,
-1.74538787858084));
#26387=CARTESIAN_POINT('Ctrl Pts',(-31.8848341748767,-2.66338978325909,
-3.30252489436533));
#26388=CARTESIAN_POINT('Ctrl Pts',(-31.7659251758817,-0.762024275548931,
-4.17368360225475));
#26389=CARTESIAN_POINT('Ctrl Pts',(-31.6470161768868,1.32451446852128,-4.03062988269698));
#26390=CARTESIAN_POINT('Ctrl Pts',(-31.5281071778918,3.08919387167645,-2.90812603048288));
#26391=CARTESIAN_POINT('Ctrl Pts',(-31.4091981788968,4.10319375653073,-1.07894246870398));
#26392=CARTESIAN_POINT('Ctrl Pts',(-31.2902891799019,4.12011035263834,1.01242603005823));
#26393=CARTESIAN_POINT('Ctrl Pts',(-31.1713801809069,3.13583293969945,2.85777317714776));
#26394=CARTESIAN_POINT('Ctrl Pts',(-31.0524711819119,1.38954257002262,4.00867653673046));
#26395=CARTESIAN_POINT('Ctrl Pts',(-30.933562182917,-0.694408967730227,
4.18546426527762));
#26396=CARTESIAN_POINT('Ctrl Pts',(-30.8146531839221,-2.6096181325775,3.34517725330154));
#26397=CARTESIAN_POINT('Ctrl Pts',(-30.7027366793076,-3.81535138401945,
1.78922095425846));
#26398=CARTESIAN_POINT('Ctrl Pts',(-30.6304565076916,-4.07005755406551,
0.556440132046678));
#26399=CARTESIAN_POINT('Ctrl Pts',(-30.5978126690739,-4.07061596824169,
-9.62913744964253E-5));
#26400=CARTESIAN_POINT('Ctrl Pts',(-31.8021873309261,-4.07065754153041,
-9.0345402713049E-5));
#26401=CARTESIAN_POINT('Ctrl Pts',(-31.7960032155922,-4.07075935824244,
-0.105518617748798));
#26402=CARTESIAN_POINT('Ctrl Pts',(-31.75018276726,-4.04102178465253,-0.88661924731187));
#26403=CARTESIAN_POINT('Ctrl Pts',(-31.6647259859294,-3.55858318971203,
-2.31015180080996));
#26404=CARTESIAN_POINT('Ctrl Pts',(-31.5458169869345,-2.02255110907419,
-3.72955802299772));
#26405=CARTESIAN_POINT('Ctrl Pts',(-31.4269079879395,0.00496435902457082,
-4.24267488557468));
#26406=CARTESIAN_POINT('Ctrl Pts',(-31.3079989889446,2.03127363286532,-3.72481475967269));
#26407=CARTESIAN_POINT('Ctrl Pts',(-31.1890899899496,3.56397954706214,-2.30181723085673));
#26408=CARTESIAN_POINT('Ctrl Pts',(-31.0701809909547,4.23063279613937,-0.319475851207252));
#26409=CARTESIAN_POINT('Ctrl Pts',(-30.9512719919596,3.86923364069296,1.74050225247754));
#26410=CARTESIAN_POINT('Ctrl Pts',(-30.8323629929648,2.56760636218215,3.37752821215737));
#26411=CARTESIAN_POINT('Ctrl Pts',(-30.7134539939697,0.642041383293453,
4.19382295160038));
#26412=CARTESIAN_POINT('Ctrl Pts',(-30.5945449949749,-1.43953109436157,
3.99098332553759));
#26413=CARTESIAN_POINT('Ctrl Pts',(-30.4756359959798,-3.17131430799793,
2.8183836925229));
#26414=CARTESIAN_POINT('Ctrl Pts',(-30.378183441297,-3.9589973334931,1.29599045009805));
#26415=CARTESIAN_POINT('Ctrl Pts',(-30.3203672196124,-4.07023481064188,
0.310076237309551));
#26416=CARTESIAN_POINT('Ctrl Pts',(-30.3021873309261,-4.0701702520628,4.41716588963498E-5));
#26417=CARTESIAN_POINT('Origin',(-55.3478126690739,0.,0.));
#26418=CARTESIAN_POINT('',(-33.5978126690739,-4.07020326590693,-5.60749306866135E-5));
#26419=CARTESIAN_POINT('',(-33.3021873309261,-4.07050357498408,0.000104730133066722));
#26420=CARTESIAN_POINT('',(-55.3478126690739,-4.0705,-3.42898509504556E-13));
#26421=CARTESIAN_POINT('Ctrl Pts',(-33.5978126690739,-4.07020326590693,
-5.60749306863922E-5));
#26422=CARTESIAN_POINT('Ctrl Pts',(-33.5817284996513,-4.07033713790938,
-0.274350811580848));
#26423=CARTESIAN_POINT('Ctrl Pts',(-33.5260079972304,-3.97569374054994,
-1.22450089022107));
#26424=CARTESIAN_POINT('Ctrl Pts',(-33.4306511618112,-3.24442008373921,
-2.73387163822095));
#26425=CARTESIAN_POINT('Ctrl Pts',(-33.3117421628162,-1.5441295420815,-3.95170593178579));
#26426=CARTESIAN_POINT('Ctrl Pts',(-33.1928331638213,0.531387184754894,
-4.20926875762475));
#26427=CARTESIAN_POINT('Ctrl Pts',(-33.0739241648263,2.47777589431427,-3.44397189762026));
#26428=CARTESIAN_POINT('Ctrl Pts',(-32.9550151658313,3.82206071866471,-1.84178383011512));
#26429=CARTESIAN_POINT('Ctrl Pts',(-32.8361061668364,4.23757808931381,0.207960936267553));
#26430=CARTESIAN_POINT('Ctrl Pts',(-32.7171971678414,3.62335655689582,2.20717083064289));
#26431=CARTESIAN_POINT('Ctrl Pts',(-32.5982881688465,2.12865303036779,3.67003434456881));
#26432=CARTESIAN_POINT('Ctrl Pts',(-32.4793791698515,0.116683086477182,
4.24107308018517));
#26433=CARTESIAN_POINT('Ctrl Pts',(-32.3604701708566,-1.92364105191405,
3.78152362377861));
#26434=CARTESIAN_POINT('Ctrl Pts',(-32.2415611718616,-3.49651704310921,
2.40305729888056));
#26435=CARTESIAN_POINT('Ctrl Pts',(-32.1540086712673,-4.0290199584954,0.95813549201353));
#26436=CARTESIAN_POINT('Ctrl Pts',(-32.1060925036714,-4.07069224764503,
0.141270575619876));
#26437=CARTESIAN_POINT('Ctrl Pts',(-32.0978126690739,-4.07054710488196,
0.000102932729767729));
#26438=CARTESIAN_POINT('Ctrl Pts',(-33.3021873309261,-4.07050357498408,
0.00010473013306686));
#26439=CARTESIAN_POINT('Ctrl Pts',(-33.2716392115721,-4.0699706197775,-0.520743687508975));
#26440=CARTESIAN_POINT('Ctrl Pts',(-33.2014547592197,-3.83934010403903,
-1.71785382786294));
#26441=CARTESIAN_POINT('Ctrl Pts',(-33.091633973869,-2.69680011715167,-3.27529919943904));
#26442=CARTESIAN_POINT('Ctrl Pts',(-32.9727249748741,-0.804382135063499,
-4.16572743931235));
#26443=CARTESIAN_POINT('Ctrl Pts',(-32.853815975879,1.28350211569609,-4.04387660995158));
#26444=CARTESIAN_POINT('Ctrl Pts',(-32.7349069768842,3.05949310273849,-2.93935667663218));
#26445=CARTESIAN_POINT('Ctrl Pts',(-32.6159979778891,4.09202190325118,-1.12056791874808));
#26446=CARTESIAN_POINT('Ctrl Pts',(-32.4970889788942,4.13018220918936,0.970520807006677));
#26447=CARTESIAN_POINT('Ctrl Pts',(-32.3781799798992,3.16470099886364,2.82577127648086));
#26448=CARTESIAN_POINT('Ctrl Pts',(-32.2592709809043,1.43019189953828,3.99435437116099));
#26449=CARTESIAN_POINT('Ctrl Pts',(-32.1403619819093,-0.651856339348117,
4.19230235613684));
#26450=CARTESIAN_POINT('Ctrl Pts',(-32.0214529829143,-2.57550234280079,
3.37151351350433));
#26451=CARTESIAN_POINT('Ctrl Pts',(-31.9087280992533,-3.80580220902221,
1.8167364506488));
#26452=CARTESIAN_POINT('Ctrl Pts',(-31.8356395485905,-4.07010677644452,
0.570211035487816));
#26453=CARTESIAN_POINT('Ctrl Pts',(-31.8021873309261,-4.07065754153041,
-9.0345402713049E-5));
#26454=CARTESIAN_POINT('Origin',(-55.3478126690739,0.,0.));
#26455=CARTESIAN_POINT('',(-35.0978126690738,-4.07084382520696,-1.45670438658383E-5));
#26456=CARTESIAN_POINT('',(-34.8021873309261,-4.07022604729798,-6.65076760328343E-5));
#26457=CARTESIAN_POINT('',(-55.3478126690739,-4.0705,-3.42898509504556E-13));
#26458=CARTESIAN_POINT('Ctrl Pts',(-35.0978126690738,-4.07084382520696,
-1.45670438656941E-5));
#26459=CARTESIAN_POINT('Ctrl Pts',(-35.0970008286294,-4.07084664099177,
-0.0138531808912899));
#26460=CARTESIAN_POINT('Ctrl Pts',(-35.0565526551867,-4.0674041557348,-0.703330423914037));
#26461=CARTESIAN_POINT('Ctrl Pts',(-34.9764681487457,-3.70631687576659,
-2.06483196179423));
#26462=CARTESIAN_POINT('Ctrl Pts',(-34.8575591497507,-2.26953513242235,
-3.58462356416123));
#26463=CARTESIAN_POINT('Ctrl Pts',(-34.7386501507558,-0.281252374001066,
-4.2333453575344));
#26464=CARTESIAN_POINT('Ctrl Pts',(-34.6197411517608,1.77537520426393,-3.8533568090853));
#26465=CARTESIAN_POINT('Ctrl Pts',(-34.5008321527659,3.40058349612684,-2.5369958021071));
#26466=CARTESIAN_POINT('Ctrl Pts',(-34.3819231537709,4.19944403810212,-0.604140368530221));
#26467=CARTESIAN_POINT('Ctrl Pts',(-34.2630141547759,3.97783231829727,1.47552223349874));
#26468=CARTESIAN_POINT('Ctrl Pts',(-34.144105155781,2.78960037305193,3.19663034658495));
#26469=CARTESIAN_POINT('Ctrl Pts',(-34.025196156786,0.92349064771896,4.14095168259845));
#26470=CARTESIAN_POINT('Ctrl Pts',(-33.9062871577911,-1.16702892364603,
4.07901450174094));
#26471=CARTESIAN_POINT('Ctrl Pts',(-33.7873781587961,-2.97395842107017,
3.02586964752038));
#26472=CARTESIAN_POINT('Ctrl Pts',(-33.6845533292237,-3.9115499238755,1.47934517898094));
#26473=CARTESIAN_POINT('Ctrl Pts',(-33.6213648326496,-4.07000723618249,
0.401595657019318));
#26474=CARTESIAN_POINT('Ctrl Pts',(-33.5978126690739,-4.07020326590693,
-5.60749306863922E-5));
#26475=CARTESIAN_POINT('Ctrl Pts',(-34.8021873309261,-4.07022604729797,
-6.65076760328689E-5));
#26476=CARTESIAN_POINT('Ctrl Pts',(-34.7869115405502,-4.07037793767931,
-0.260571206194689));
#26477=CARTESIAN_POINT('Ctrl Pts',(-34.731999417176,-3.98185833732723,-1.19690962121964));
#26478=CARTESIAN_POINT('Ctrl Pts',(-34.6374509608035,-3.27202393444525,
-2.70077305417611));
#26479=CARTESIAN_POINT('Ctrl Pts',(-34.5185419618086,-1.5841921492944,-3.93581642761199));
#26480=CARTESIAN_POINT('Ctrl Pts',(-34.3996329628135,0.488601104807327,
-4.21444951068671));
#26481=CARTESIAN_POINT('Ctrl Pts',(-34.2807239638187,2.44266343405159,-3.46896397584259));
#26482=CARTESIAN_POINT('Ctrl Pts',(-34.1618149648236,3.80315426747452,-1.88051411468693));
#26483=CARTESIAN_POINT('Ctrl Pts',(-34.0429059658287,4.2394719479716,0.164903972384525));
#26484=CARTESIAN_POINT('Ctrl Pts',(-33.9239969668337,3.64559051443191,2.17025010513313));
#26485=CARTESIAN_POINT('Ctrl Pts',(-33.8050879678388,2.1658241961235,3.64822165845675));
#26486=CARTESIAN_POINT('Ctrl Pts',(-33.6861789688438,0.159758802036821,
4.23966895440156));
#26487=CARTESIAN_POINT('Ctrl Pts',(-33.5672699698489,-1.88512826096029,
3.80086926340264));
#26488=CARTESIAN_POINT('Ctrl Pts',(-33.4483609708539,-3.47192585240921,
2.43845167947057));
#26489=CARTESIAN_POINT('Ctrl Pts',(-33.360000091213,-4.02413102782502,0.985723265658703));
#26490=CARTESIAN_POINT('Ctrl Pts',(-33.3112755445704,-4.07066213174249,
0.155059660122451));
#26491=CARTESIAN_POINT('Ctrl Pts',(-33.3021873309261,-4.07050357498408,
0.00010473013306686));
#26492=CARTESIAN_POINT('Origin',(-55.3478126690739,0.,0.));
#26493=CARTESIAN_POINT('',(-36.5978126690739,-4.07025299976624,7.60445323442731E-5));
#26494=CARTESIAN_POINT('',(-36.3021873309261,-4.07084820048865,-6.23604784373507E-8));
#26495=CARTESIAN_POINT('',(-55.3478126690739,-4.0705,-3.42898509504556E-13));
#26496=CARTESIAN_POINT('Ctrl Pts',(-36.5978126690739,-4.07025299976624,
7.60445323443742E-5));
#26497=CARTESIAN_POINT('Ctrl Pts',(-36.5726368246093,-4.06996425256608,
-0.42925044427071));
#26498=CARTESIAN_POINT('Ctrl Pts',(-36.5078246471464,-3.89585403258829,
-1.53472847241628));
#26499=CARTESIAN_POINT('Ctrl Pts',(-36.4033761366853,-2.91160450999496,
-3.08591558397465));
#26500=CARTESIAN_POINT('Ctrl Pts',(-36.2844671376902,-1.08356448404466,
-4.10197559999513));
#26501=CARTESIAN_POINT('Ctrl Pts',(-36.1655581386953,1.00778361073219,-4.1212483555325));
#26502=CARTESIAN_POINT('Ctrl Pts',(-36.0466491397003,2.85423852172137,-3.1390505372104));
#26503=CARTESIAN_POINT('Ctrl Pts',(-35.9277401407054,4.00710846920256,-1.394057936416));
#26504=CARTESIAN_POINT('Ctrl Pts',(-35.8088311417104,4.18624403525991,0.689693186344611));
#26505=CARTESIAN_POINT('Ctrl Pts',(-35.6899221427155,3.34811496336391,2.60584765597262));
#26506=CARTESIAN_POINT('Ctrl Pts',(-35.5710131437205,1.69638808700519,3.88877657783347));
#26507=CARTESIAN_POINT('Ctrl Pts',(-35.4521041447256,-0.36756406781807,
4.22672597527783));
#26508=CARTESIAN_POINT('Ctrl Pts',(-35.3331951457305,-2.34219750991838,
3.53757355239032));
#26509=CARTESIAN_POINT('Ctrl Pts',(-35.2150979871801,-3.73807709597292,
1.99935877273991));
#26510=CARTESIAN_POINT('Ctrl Pts',(-35.1366371616278,-4.07070916646062,
0.661786854627458));
#26511=CARTESIAN_POINT('Ctrl Pts',(-35.0978126690738,-4.07084382520696,
-1.45670438656941E-5));
#26512=CARTESIAN_POINT('Ctrl Pts',(-36.3021873309261,-4.07084820044996,
-6.23604713442248E-8));
#26513=CARTESIAN_POINT('Ctrl Pts',(-36.3021838695284,-4.07084820050436,
-5.90650820220945E-5));
#26514=CARTESIAN_POINT('Ctrl Pts',(-36.2625440751324,-4.07083381658627,
-0.675755978339213));
#26515=CARTESIAN_POINT('Ctrl Pts',(-36.183267947738,-3.72710064368882,-2.02707585195046));
#26516=CARTESIAN_POINT('Ctrl Pts',(-36.064358948743,-2.30583140769797,-3.56138417430919));
#26517=CARTESIAN_POINT('Ctrl Pts',(-35.9454499497481,-0.324241098120267,
-4.23026990014066));
#26518=CARTESIAN_POINT('Ctrl Pts',(-35.8265409507531,1.73614036661006,-3.87119262568701));
#26519=CARTESIAN_POINT('Ctrl Pts',(-35.7076319517581,3.37463667925653,-2.5714087580085));
#26520=CARTESIAN_POINT('Ctrl Pts',(-35.5887229527632,4.19309036399278,-0.646768055130456));
#26521=CARTESIAN_POINT('Ctrl Pts',(-35.4698139537682,3.99261574089381,1.43503841875865));
#26522=CARTESIAN_POINT('Ctrl Pts',(-35.3509049547733,2.82192849475196,3.16812804164435));
#26523=CARTESIAN_POINT('Ctrl Pts',(-35.2319959557783,0.96550767828667,4.13135699751496));
#26524=CARTESIAN_POINT('Ctrl Pts',(-35.1130869567833,-1.12553319628343,
4.09065896180682));
#26525=CARTESIAN_POINT('Ctrl Pts',(-34.9941779577884,-2.94306753139286,
3.05592362852992));
#26526=CARTESIAN_POINT('Ctrl Pts',(-34.8905447491693,-3.90381478483326,
1.5069203921675));
#26527=CARTESIAN_POINT('Ctrl Pts',(-34.8265478735485,-4.06998382532337,
0.415364422931012));
#26528=CARTESIAN_POINT('Ctrl Pts',(-34.8021873309261,-4.07022604729797,
-6.65076760328689E-5));
#26529=CARTESIAN_POINT('Origin',(-55.3478126690739,0.,0.));
#26530=CARTESIAN_POINT('',(-38.0978126690739,-4.07046019877506,-0.000104814226016249));
#26531=CARTESIAN_POINT('',(-37.8021873309261,-4.07022625973033,6.65930553865601E-5));
#26532=CARTESIAN_POINT('',(-55.3478126690739,-4.0705,-3.42898509504556E-13));
#26533=CARTESIAN_POINT('Ctrl Pts',(-38.0978126690739,-4.07046019877506,
-0.000104814226015906));
#26534=CARTESIAN_POINT('Ctrl Pts',(-38.0879091535875,-4.07062966286641,
-0.168965898851486));
#26535=CARTESIAN_POINT('Ctrl Pts',(-38.0383693051028,-4.01905313428485,
-1.01354823242553));
#26536=CARTESIAN_POINT('Ctrl Pts',(-37.9491931236197,-3.44676120350641,
-2.47389430094654));
#26537=CARTESIAN_POINT('Ctrl Pts',(-37.8302841246248,-1.8460886395937,-3.81998331873136));
#26538=CARTESIAN_POINT('Ctrl Pts',(-37.7113751256298,0.203186699106992,
-4.23780969080775));
#26539=CARTESIAN_POINT('Ctrl Pts',(-37.5924661266349,2.20308731396286,-3.6258408821712));
#26540=CARTESIAN_POINT('Ctrl Pts',(-37.4735571276399,3.6676338500072,-2.13278638305928));
#26541=CARTESIAN_POINT('Ctrl Pts',(-37.3546481286449,4.24093893214488,-0.121461055132279));
#26542=CARTESIAN_POINT('Ctrl Pts',(-37.23573912965,3.78368842049889,1.91937952232278));
#26543=CARTESIAN_POINT('Ctrl Pts',(-37.116830130655,2.40699499087144,3.49380751156464));
#26544=CARTESIAN_POINT('Ctrl Pts',(-36.9979211316601,0.445397559627416,
4.219234151831));
#26545=CARTESIAN_POINT('Ctrl Pts',(-36.8790121326651,-1.62443225926818,
3.91937949796381));
#26546=CARTESIAN_POINT('Ctrl Pts',(-36.7601031336701,-3.2995221919603,2.66710875646485));
#26547=CARTESIAN_POINT('Ctrl Pts',(-36.6663699791397,-3.98792415159873,
1.16908185946355));
#26548=CARTESIAN_POINT('Ctrl Pts',(-36.6122731576076,-4.07041885023385,
0.246672371313648));
#26549=CARTESIAN_POINT('Ctrl Pts',(-36.5978126690739,-4.07025299976624,
7.60445323443742E-5));
#26550=CARTESIAN_POINT('Ctrl Pts',(-37.8021873309261,-4.07022625973033,
6.65930553865948E-5));
#26551=CARTESIAN_POINT('Ctrl Pts',(-37.7778198655082,-4.06998364140991,
-0.415482332889415));
#26552=CARTESIAN_POINT('Ctrl Pts',(-37.7138160670921,-3.90374786422602,
-1.5071565272805));
#26553=CARTESIAN_POINT('Ctrl Pts',(-37.6101759356775,-2.94280167197283,
-3.05617964738425));
#26554=CARTESIAN_POINT('Ctrl Pts',(-37.4912669366826,-1.12517732754963,
-4.09075686143469));
#26555=CARTESIAN_POINT('Ctrl Pts',(-37.3723579376876,0.965867079610468,
-4.13127298810448));
#26556=CARTESIAN_POINT('Ctrl Pts',(-37.2534489386927,2.82220409351303,-3.1678825376449));
#26557=CARTESIAN_POINT('Ctrl Pts',(-37.1345399396977,3.99274056611069,-1.43469107806466));
#26558=CARTESIAN_POINT('Ctrl Pts',(-37.0156309407027,4.19303408291871,0.647132828117663));
#26559=CARTESIAN_POINT('Ctrl Pts',(-36.8967219417077,3.37441296829128,2.57170232281563));
#26560=CARTESIAN_POINT('Ctrl Pts',(-36.7778129427128,1.73580358791025,3.87134364555039));
#26561=CARTESIAN_POINT('Ctrl Pts',(-36.6589039437178,-0.324609106740258,
4.23024167696931));
#26562=CARTESIAN_POINT('Ctrl Pts',(-36.5399949447229,-2.3061412194985,3.56118356638298));
#26563=CARTESIAN_POINT('Ctrl Pts',(-36.4210894071256,-3.7272356051144,2.02679627410343));
#26564=CARTESIAN_POINT('Ctrl Pts',(-36.3418202025267,-4.07084757762592,
0.675578845480269));
#26565=CARTESIAN_POINT('Ctrl Pts',(-36.3021873309261,-4.07084820044996,
-6.23604713442248E-8));
#26566=CARTESIAN_POINT('Origin',(-55.3478126690739,0.,0.));
#26567=CARTESIAN_POINT('',(-39.5978126690739,-4.07069839459796,9.13927329241537E-5));
#26568=CARTESIAN_POINT('',(-39.3021873309261,-4.07050320376008,-0.000104740849479479));
#26569=CARTESIAN_POINT('',(-55.3478126690739,-4.0705,-3.42898509504556E-13));
#26570=CARTESIAN_POINT('Ctrl Pts',(-39.5978126690739,-4.07069839459796,
9.13927329241997E-5));
#26571=CARTESIAN_POINT('Ctrl Pts',(-39.5635451495673,-4.07016736041225,
-0.584091196748413));
#26572=CARTESIAN_POINT('Ctrl Pts',(-39.4896412970624,-3.79600154444092,
-1.84449221170457));
#26573=CARTESIAN_POINT('Ctrl Pts',(-39.3761011115593,-2.54082596720782,
-3.39771596970325));
#26574=CARTESIAN_POINT('Ctrl Pts',(-39.2571921125643,-0.608870808304631,
-4.19876432921494));
#26575=CARTESIAN_POINT('Ctrl Pts',(-39.1382831135694,1.47103966436091,-3.97949033645411));
#26576=CARTESIAN_POINT('Ctrl Pts',(-39.0193741145744,3.19348560173252,-2.79320086500867));
#26577=CARTESIAN_POINT('Ctrl Pts',(-38.9004651155794,4.13990859901063,-0.928154854760866));
#26578=CARTESIAN_POINT('Ctrl Pts',(-38.7815561165844,4.08032672171768,1.16243249115508));
#26579=CARTESIAN_POINT('Ctrl Pts',(-38.6626471175895,3.02921821353002,2.97054766692245));
#26580=CARTESIAN_POINT('Ctrl Pts',(-38.5437381185945,1.24200441301907,4.05681407060795));
#26581=CARTESIAN_POINT('Ctrl Pts',(-38.4248291195996,-0.84701865830611,
4.15726778637903));
#26582=CARTESIAN_POINT('Ctrl Pts',(-38.3059201206046,-2.73021470026535,
3.2474980222978));
#26583=CARTESIAN_POINT('Ctrl Pts',(-38.196914637096,-3.84837514583954,1.69007750908748));
#26584=CARTESIAN_POINT('Ctrl Pts',(-38.1275454865858,-4.06995142540971,
0.506858174919875));
#26585=CARTESIAN_POINT('Ctrl Pts',(-38.0978126690739,-4.07046019877506,
-0.000104814226015906));
#26586=CARTESIAN_POINT('Ctrl Pts',(-39.3021873309261,-4.07050320376008,
-0.000104740849479045));
#26587=CARTESIAN_POINT('Ctrl Pts',(-39.2930921944864,-4.07066186300007,
-0.155177721080473));
#26588=CARTESIAN_POINT('Ctrl Pts',(-39.2443607250484,-4.02408852320218,
-0.985959385916872));
#26589=CARTESIAN_POINT('Ctrl Pts',(-39.155992922612,-3.47171371609164,-2.43875382264022));
#26590=CARTESIAN_POINT('Ctrl Pts',(-39.0370839236171,-1.88479759517879,
-3.80103318737441));
#26591=CARTESIAN_POINT('Ctrl Pts',(-38.9181749246221,0.160127626810078,
-4.23965506894654));
#26592=CARTESIAN_POINT('Ctrl Pts',(-38.7992659256272,2.16614156389975,-3.64803321565397));
#26593=CARTESIAN_POINT('Ctrl Pts',(-38.6803569266322,3.6457792997346,-2.16993295812935));
#26594=CARTESIAN_POINT('Ctrl Pts',(-38.5614479276372,4.23948627792256,-0.164535157769628));
#26595=CARTESIAN_POINT('Ctrl Pts',(-38.4425389286423,3.80299065872691,1.88084495893092));
#26596=CARTESIAN_POINT('Ctrl Pts',(-38.3236299296473,2.44236164439116,3.46917646169672));
#26597=CARTESIAN_POINT('Ctrl Pts',(-38.2047209306524,0.488234469363121,
4.21449199984978));
#26598=CARTESIAN_POINT('Ctrl Pts',(-38.0858119316573,-1.58453453732273,
3.93567859708109));
#26599=CARTESIAN_POINT('Ctrl Pts',(-37.9669029326625,-3.27225887423897,
2.70048839604023));
#26600=CARTESIAN_POINT('Ctrl Pts',(-37.8723613990853,-3.98191048253192,
1.19667333400869));
#26601=CARTESIAN_POINT('Ctrl Pts',(-37.8174561985065,-4.07037828649813,
0.260453195216987));
#26602=CARTESIAN_POINT('Ctrl Pts',(-37.8021873309261,-4.07022625973033,
6.65930553865948E-5));
#26603=CARTESIAN_POINT('Origin',(-55.3478126690739,0.,0.));
#26604=CARTESIAN_POINT('',(-41.0978126690738,-4.06894916332632,0.00540720055342753));
#26605=CARTESIAN_POINT('',(-40.8021873309261,-4.07070024200598,-0.000481747532086602));
#26606=CARTESIAN_POINT('',(-55.3478126690739,-4.0705,-3.42898509504556E-13));
#26607=CARTESIAN_POINT('Ctrl Pts',(-41.0978126690739,-4.06894916332632,
0.00540720055342749));
#26608=CARTESIAN_POINT('Ctrl Pts',(-41.0391811455472,-4.05939879775064,
-0.995808352670484));
#26609=CARTESIAN_POINT('Ctrl Pts',(-40.9012769560238,-3.18277581994412,
-3.36894444071793));
#26610=CARTESIAN_POINT('Ctrl Pts',(-40.7237364335021,0.0468138156189731,
-4.48441463662212));
#26611=CARTESIAN_POINT('Ctrl Pts',(-40.5651911015089,2.60148923263442,-3.34401588370882));
#26612=CARTESIAN_POINT('Ctrl Pts',(-40.4462821025139,3.88717861421759,-1.70434784922236));
#26613=CARTESIAN_POINT('Ctrl Pts',(-40.327373103519,4.22697739474136,0.364600408636661));
#26614=CARTESIAN_POINT('Ctrl Pts',(-40.208464104524,3.54029037696192,2.33730890925922));
#26615=CARTESIAN_POINT('Ctrl Pts',(-40.0895551055291,1.99296520133986,3.74588177308733));
#26616=CARTESIAN_POINT('Ctrl Pts',(-39.9706461065341,-0.0384827646914282,
4.24227672531885));
#26617=CARTESIAN_POINT('Ctrl Pts',(-39.8517371075391,-2.06066518446267,
3.70875428242689));
#26618=CARTESIAN_POINT('Ctrl Pts',(-39.7328281085442,-3.58205933615999,
2.27351529266644));
#26619=CARTESIAN_POINT('Ctrl Pts',(-39.6481866290558,-4.04543032394026,
0.858803192571973));
#26620=CARTESIAN_POINT('Ctrl Pts',(-39.6031814825656,-4.0707815936022,0.0916173453910432));
#26621=CARTESIAN_POINT('Ctrl Pts',(-39.5978126690739,-4.07069839459796,
9.13927329241997E-5));
#26622=CARTESIAN_POINT('Ctrl Pts',(-40.8021873309261,-4.07070024200598,
-0.000481747532086515));
#26623=CARTESIAN_POINT('Ctrl Pts',(-40.7687281904663,-4.07015465516028,
-0.570964956116361));
#26624=CARTESIAN_POINT('Ctrl Pts',(-40.695632717008,-3.80565769799185,-1.81613807110307));
#26625=CARTESIAN_POINT('Ctrl Pts',(-40.5829009105516,-2.57524274258496,
-3.37219103126866));
#26626=CARTESIAN_POINT('Ctrl Pts',(-40.4639919115566,-0.651474730133847,
-4.1921317137068));
#26627=CARTESIAN_POINT('Ctrl Pts',(-40.3450829125617,1.43053090860402,-3.99434390257198));
#26628=CARTESIAN_POINT('Ctrl Pts',(-40.2261739135667,3.1649510603171,-2.82543882253934));
#26629=CARTESIAN_POINT('Ctrl Pts',(-40.1072649145718,4.13026449432683,-0.970190141382548));
#26630=CARTESIAN_POINT('Ctrl Pts',(-39.9883559155767,4.09192547196896,1.12093825548876));
#26631=CARTESIAN_POINT('Ctrl Pts',(-39.8694469165819,3.0592368484789,2.93961562653621));
#26632=CARTESIAN_POINT('Ctrl Pts',(-39.7505379175868,1.28315058440506,4.04399186048308));
#26633=CARTESIAN_POINT('Ctrl Pts',(-39.6316289185919,-0.804744661503545,
4.16565563790974));
#26634=CARTESIAN_POINT('Ctrl Pts',(-39.5127199195969,-2.69708497226697,
3.27506548731581));
#26635=CARTESIAN_POINT('Ctrl Pts',(-39.4029060570417,-3.83941754526237,
1.7176176530298));
#26636=CARTESIAN_POINT('Ctrl Pts',(-39.3327285274847,-4.0699704307702,0.520625695858415));
#26637=CARTESIAN_POINT('Ctrl Pts',(-39.3021873309261,-4.07050320376008,
-0.000104740849479045));
#26638=CARTESIAN_POINT('Origin',(-55.3478126690739,0.,0.));
#26639=CARTESIAN_POINT('',(-42.5978126690739,-4.07077051219227,-5.79810753342639E-5));
#26640=CARTESIAN_POINT('',(-42.3021873309261,-4.0702562437931,0.000377661753542397));
#26641=CARTESIAN_POINT('',(-55.3478126690739,-4.0705,-3.42898509504556E-13));
#26642=CARTESIAN_POINT('Ctrl Pts',(-42.5978126690739,-4.07077051219227,
-5.79810753340362E-5));
#26643=CARTESIAN_POINT('Ctrl Pts',(-42.5940898075237,-4.07081705779188,
-0.0635213374655559));
#26644=CARTESIAN_POINT('Ctrl Pts',(-42.5507306129751,-4.05388726315202,
-0.802638451157566));
#26645=CARTESIAN_POINT('Ctrl Pts',(-42.4677350854283,-3.62830976367934,
-2.19902748573468));
#26646=CARTESIAN_POINT('Ctrl Pts',(-42.3488260864333,-2.13693866142688,
-3.66517585267858));
#26647=CARTESIAN_POINT('Ctrl Pts',(-42.2299170874383,-0.126195704091931,
-4.24090485322945));
#26648=CARTESIAN_POINT('Ctrl Pts',(-42.1110080884434,1.91502942438633,-3.78563799657268));
#26649=CARTESIAN_POINT('Ctrl Pts',(-41.9920990894484,3.49126541284734,-2.41134949120931));
#26650=CARTESIAN_POINT('Ctrl Pts',(-41.8731900904535,4.21838674592901,-0.449312978092323));
#26651=CARTESIAN_POINT('Ctrl Pts',(-41.7542810914585,3.92189134396604,1.61834472216421));
#26652=CARTESIAN_POINT('Ctrl Pts',(-41.6353720924635,2.66945995165433,3.29983980467131));
#26653=CARTESIAN_POINT('Ctrl Pts',(-41.5164630934686,0.77413855912781,4.16544090694865));
#26654=CARTESIAN_POINT('Ctrl Pts',(-41.3579177614753,-2.01888556396995,
4.00453083969612));
#26655=CARTESIAN_POINT('Ctrl Pts',(-41.2183676200104,-3.8707199036833,2.05940273537045));
#26656=CARTESIAN_POINT('Ctrl Pts',(-41.1184538115438,-4.07231135561863,
0.35788367795225));
#26657=CARTESIAN_POINT('Ctrl Pts',(-41.0978126690739,-4.06894916332632,
0.00540720055342749));
#26658=CARTESIAN_POINT('Ctrl Pts',(-42.3021873309261,-4.0702562437931,0.000377661753542743));
#26659=CARTESIAN_POINT('Ctrl Pts',(-42.2840005194444,-4.070361788608,-0.309619941943036));
#26660=CARTESIAN_POINT('Ctrl Pts',(-42.2261773749644,-3.95913933202493,
-1.29545265190419));
#26661=CARTESIAN_POINT('Ctrl Pts',(-42.1287178974861,-3.17025358567157,
-2.82214018180611));
#26662=CARTESIAN_POINT('Ctrl Pts',(-42.0098088984911,-1.44080606975949,
-3.98424622002752));
#26663=CARTESIAN_POINT('Ctrl Pts',(-41.8512635664978,1.34123824569469,-4.27940453375867));
#26664=CARTESIAN_POINT('Ctrl Pts',(-41.6530819015062,4.38508519896316,-1.98115288915087));
#26665=CARTESIAN_POINT('Ctrl Pts',(-41.4152639035164,4.03738586191726,2.61791030678041));
#26666=CARTESIAN_POINT('Ctrl Pts',(-41.2170822385246,0.682605700869055,
4.43241160683543));
#26667=CARTESIAN_POINT('Ctrl Pts',(-41.0585369065315,-2.02344112387514,
3.7223414795892));
#26668=CARTESIAN_POINT('Ctrl Pts',(-40.9396279075364,-3.55851407251,2.3134304828493));
#26669=CARTESIAN_POINT('Ctrl Pts',(-40.8541780490014,-4.04108036770983,
0.886096610966636));
#26670=CARTESIAN_POINT('Ctrl Pts',(-40.8083645234646,-4.07080096769546,
0.1048402831881));
#26671=CARTESIAN_POINT('Ctrl Pts',(-40.8021873309261,-4.07070024200598,
-0.000481747532086515));
#26672=CARTESIAN_POINT('Origin',(-55.3478126690739,0.,0.));
#26673=CARTESIAN_POINT('',(-44.0978126690739,-4.0703765947929,9.98552879098336E-5));
#26674=CARTESIAN_POINT('',(-43.8021873309261,-4.07079741683127,-5.00544118864354E-5));
#26675=CARTESIAN_POINT('',(-55.3478126690739,-4.0705,-3.42898509504556E-13));
#26676=CARTESIAN_POINT('Ctrl Pts',(-44.0978126690739,-4.0703765947929,9.98552879100285E-5));
#26677=CARTESIAN_POINT('Ctrl Pts',(-44.0697258035035,-4.06993441861034,
-0.478826892483599));
#26678=CARTESIAN_POINT('Ctrl Pts',(-44.0020026049348,-3.86611252863601,
-1.63398403157745));
#26679=CARTESIAN_POINT('Ctrl Pts',(-43.8946430733678,-2.79679600676983,
-3.19033664959511));
#26680=CARTESIAN_POINT('Ctrl Pts',(-43.7757340743728,-0.932818792342456,
-4.1388603280403));
#26681=CARTESIAN_POINT('Ctrl Pts',(-43.6568250753779,1.15783504670461,-4.0816337488567));
#26682=CARTESIAN_POINT('Ctrl Pts',(-43.5379160763829,2.96713289393957,-3.03256290209179));
#26683=CARTESIAN_POINT('Ctrl Pts',(-43.4190070773879,4.05541233929616,-1.24657417947145));
#26684=CARTESIAN_POINT('Ctrl Pts',(-43.300098078393,4.15821929464979,0.842334701919917));
#26685=CARTESIAN_POINT('Ctrl Pts',(-43.181189079398,3.25057203925852,2.72655387993142));
#26686=CARTESIAN_POINT('Ctrl Pts',(-43.0622800804031,1.55302935037421,3.94821747091449));
#26687=CARTESIAN_POINT('Ctrl Pts',(-42.9433710814082,-0.521900734955894,
4.21045373503939));
#26688=CARTESIAN_POINT('Ctrl Pts',(-42.824462082413,-2.47001093572135,3.44954946781609));
#26689=CARTESIAN_POINT('Ctrl Pts',(-42.7092759449685,-3.7756980222501,1.90045190076457));
#26690=CARTESIAN_POINT('Ctrl Pts',(-42.633726140522,-4.07032149896954,0.612156415560098));
#26691=CARTESIAN_POINT('Ctrl Pts',(-42.5978126690739,-4.07077051219227,
-5.79810753340362E-5));
#26692=CARTESIAN_POINT('Ctrl Pts',(-43.8021873309261,-4.07079741683127,
-5.00544118866002E-5));
#26693=CARTESIAN_POINT('Ctrl Pts',(-43.7992728484226,-4.07082805237793,
-0.0497319009987912));
#26694=CARTESIAN_POINT('Ctrl Pts',(-43.7567220329207,-4.057824297978,-0.775060067942204));
#26695=CARTESIAN_POINT('Ctrl Pts',(-43.6745348844206,-3.65047141713449,
-2.16202982679776));
#26696=CARTESIAN_POINT('Ctrl Pts',(-43.5556258854256,-2.17403874853064,
-3.64333320102936));
#26697=CARTESIAN_POINT('Ctrl Pts',(-43.4367168864307,-0.169311716792706,
-4.23929645182126));
#26698=CARTESIAN_POINT('Ctrl Pts',(-43.3178078874356,1.87656008092686,-3.80511075431245));
#26699=CARTESIAN_POINT('Ctrl Pts',(-43.1988988884407,3.46642105478168,-2.44626147372541));
#26700=CARTESIAN_POINT('Ctrl Pts',(-43.0799898894457,4.21394248881074,-0.492996289805673));
#26701=CARTESIAN_POINT('Ctrl Pts',(-42.9610808904508,3.9374548435202,1.58012754509629));
#26702=CARTESIAN_POINT('Ctrl Pts',(-42.8421718914559,2.70418603569597,3.26915855205306));
#26703=CARTESIAN_POINT('Ctrl Pts',(-42.7232628924609,0.813740892457039,
4.16401580837881));
#26704=CARTESIAN_POINT('Ctrl Pts',(-42.6043538934659,-1.2743362201606,4.04653615170507));
#26705=CARTESIAN_POINT('Ctrl Pts',(-42.485444894471,-3.05296381848078,2.94668618241789));
#26706=CARTESIAN_POINT('Ctrl Pts',(-42.3847227069577,-3.93078173750272,
1.40692650742191));
#26707=CARTESIAN_POINT('Ctrl Pts',(-42.3236368524427,-4.07013176426131,
0.365988768312008));
#26708=CARTESIAN_POINT('Ctrl Pts',(-42.3021873309261,-4.0702562437931,0.000377661753542743));
#26709=CARTESIAN_POINT('Origin',(-55.3478126690739,0.,0.));
#26710=CARTESIAN_POINT('',(-45.5978126690739,-4.07031822057863,-9.16775258372991E-5));
#26711=CARTESIAN_POINT('',(-45.3021873309261,-4.07033855687931,9.50420136142105E-5));
#26712=CARTESIAN_POINT('',(-55.3478126690739,-4.0705,-3.42898509504556E-13));
#26713=CARTESIAN_POINT('Ctrl Pts',(-45.5978126690739,-4.07031822057863,
-9.16775258373928E-5));
#26714=CARTESIAN_POINT('Ctrl Pts',(-45.5849981324817,-4.07049943661512,
-0.218609364827659));
#26715=CARTESIAN_POINT('Ctrl Pts',(-45.5325472628912,-3.99970860043998,
-1.11290258178099));
#26716=CARTESIAN_POINT('Ctrl Pts',(-45.4404600603022,-3.35397801744653,
-2.59829699467222));
#26717=CARTESIAN_POINT('Ctrl Pts',(-45.3215510613074,-1.70514605769533,
-3.88494436716616));
#26718=CARTESIAN_POINT('Ctrl Pts',(-45.2026420623123,0.358039382745663,
-4.22754344914553));
#26719=CARTESIAN_POINT('Ctrl Pts',(-45.0837330633174,2.33422062563635,-3.54284206322451));
#26720=CARTESIAN_POINT('Ctrl Pts',(-44.9648240643225,3.74318216521078,-1.997223846241));
#26721=CARTESIAN_POINT('Ctrl Pts',(-44.8459150653275,4.24254387784786,0.0337232659310005));
#26722=CARTESIAN_POINT('Ctrl Pts',(-44.7270060663325,3.71095999205786,2.05647556548625));
#26723=CARTESIAN_POINT('Ctrl Pts',(-44.6080970673375,2.27760632395248,3.57950069794286));
#26724=CARTESIAN_POINT('Ctrl Pts',(-44.4891880683426,0.290790326898236,
4.23270088732366));
#26725=CARTESIAN_POINT('Ctrl Pts',(-44.3702790693477,-1.76668822890541,
3.85734734137919));
#26726=CARTESIAN_POINT('Ctrl Pts',(-44.2513700703527,-3.39485844927514,
2.54465163234734));
#26727=CARTESIAN_POINT('Ctrl Pts',(-44.1605479369281,-4.00834926416774,
1.06972434003999));
#26728=CARTESIAN_POINT('Ctrl Pts',(-44.1093621365018,-4.07055841997397,
0.197037062820157));
#26729=CARTESIAN_POINT('Ctrl Pts',(-44.0978126690739,-4.0703765947929,9.98552879100285E-5));
#26730=CARTESIAN_POINT('Ctrl Pts',(-45.3021873309261,-4.07033855687931,
9.5042013614384E-5));
#26731=CARTESIAN_POINT('Ctrl Pts',(-45.2749088444024,-4.06993566613643,
-0.465059999241131));
#26732=CARTESIAN_POINT('Ctrl Pts',(-45.2079940248804,-3.87457928875426,
-1.6064268825154));
#26733=CARTESIAN_POINT('Ctrl Pts',(-45.1014428723601,-2.82905982713036,
-3.16176156781322));
#26734=CARTESIAN_POINT('Ctrl Pts',(-44.9825338733652,-0.974814091813329,
-4.12917100710215));
#26735=CARTESIAN_POINT('Ctrl Pts',(-44.8636248743702,1.11631317618967,-4.09318465336435));
#26736=CARTESIAN_POINT('Ctrl Pts',(-44.7447158753752,2.93617438620888,-3.06254725647695));
#26737=CARTESIAN_POINT('Ctrl Pts',(-44.6258068763803,4.04254007317222,-1.28770550464645));
#26738=CARTESIAN_POINT('Ctrl Pts',(-44.5068978773853,4.16656143857104,0.800050934283993));
#26739=CARTESIAN_POINT('Ctrl Pts',(-44.3879888783903,3.27810106806685,2.69339360894175));
#26740=CARTESIAN_POINT('Ctrl Pts',(-44.2690798793954,1.59305639924211,3.93223688581989));
#26741=CARTESIAN_POINT('Ctrl Pts',(-44.1501708804004,-0.479103780509667,
4.21553976710139));
#26742=CARTESIAN_POINT('Ctrl Pts',(-44.0312618814054,-2.4348408745219,3.47445897688703));
#26743=CARTESIAN_POINT('Ctrl Pts',(-43.915267364914,-3.76547388867547,1.92793677744289));
#26744=CARTESIAN_POINT('Ctrl Pts',(-43.8389091814209,-4.07041141555569,
0.625930489462706));
#26745=CARTESIAN_POINT('Ctrl Pts',(-43.8021873309261,-4.07079741683127,
-5.00544118866002E-5));
#26746=CARTESIAN_POINT('Origin',(-55.3478126690739,0.,0.));
#26747=CARTESIAN_POINT('',(-47.0978126690739,-4.07081123287269,4.27420414081398E-5));
#26748=CARTESIAN_POINT('',(-46.8021873309261,-4.07035480316255,-9.73195009795758E-5));
#26749=CARTESIAN_POINT('',(-55.3478126690739,-4.0705,-3.42898509504556E-13));
#26750=CARTESIAN_POINT('Ctrl Pts',(-47.0978126690739,-4.07081123287269,
4.27420414080091E-5));
#26751=CARTESIAN_POINT('Ctrl Pts',(-47.0606341284615,-4.07046881201322,
-0.633716584336426));
#26752=CARTESIAN_POINT('Ctrl Pts',(-46.9838192548509,-3.7596214042551,-1.94345587087894));
#26753=CARTESIAN_POINT('Ctrl Pts',(-46.8673680482418,-2.41486120468549,
-3.4883751484243));
#26754=CARTESIAN_POINT('Ctrl Pts',(-46.748459049247,-0.454903300248022,
-4.21821986167895));
#26755=CARTESIAN_POINT('Ctrl Pts',(-46.6295500502518,1.61559690347559,-3.92302975511522));
#26756=CARTESIAN_POINT('Ctrl Pts',(-46.510641051257,3.29350422793804,-2.67453654201874));
#26757=CARTESIAN_POINT('Ctrl Pts',(-46.391732052262,4.17108425236453,-0.776126261452312));
#26758=CARTESIAN_POINT('Ctrl Pts',(-46.2728230532671,4.03508349265237,1.3108840609923));
#26759=CARTESIAN_POINT('Ctrl Pts',(-46.153914054272,2.91855037178518,3.0793472589807));
#26760=CARTESIAN_POINT('Ctrl Pts',(-46.0350050552771,1.09280439512275,4.09952367575057));
#26761=CARTESIAN_POINT('Ctrl Pts',(-45.9160960562821,-0.998494964953347,
4.123508653926));
#26762=CARTESIAN_POINT('Ctrl Pts',(-45.7971870572872,-2.84715829844654,
3.14547380177063));
#26763=CARTESIAN_POINT('Ctrl Pts',(-45.6910925948844,-3.87929174472671,
1.59085653253142));
#26764=CARTESIAN_POINT('Ctrl Pts',(-45.62463446548,-4.06993892167843,0.457282405241305));
#26765=CARTESIAN_POINT('Ctrl Pts',(-45.5978126690739,-4.07031822057863,
-9.16775258373928E-5));
#26766=CARTESIAN_POINT('Ctrl Pts',(-46.8021873309261,-4.07035480316255,
-9.73195009796278E-5));
#26767=CARTESIAN_POINT('Ctrl Pts',(-46.7901811733806,-4.07053748381602,
-0.204824980679389));
#26768=CARTESIAN_POINT('Ctrl Pts',(-46.7385386828367,-4.00527158843597,
-1.08531156100483));
#26769=CARTESIAN_POINT('Ctrl Pts',(-46.6472598592946,-3.38019901859953,
-2.5640924929505));
#26770=CARTESIAN_POINT('Ctrl Pts',(-46.5283508602997,-1.74452217827771,
-3.8674226672609));
#26771=CARTESIAN_POINT('Ctrl Pts',(-46.4094418613047,0.315076609054344,
-4.23096235485186));
#26772=CARTESIAN_POINT('Ctrl Pts',(-46.2905328623097,2.29811122813968,-3.56637077444897));
#26773=CARTESIAN_POINT('Ctrl Pts',(-46.1716238633148,3.72270079080243,-2.03514484494512));
#26774=CARTESIAN_POINT('Ctrl Pts',(-46.0527148643198,4.2426675363842,-0.00937515104479359));
#26775=CARTESIAN_POINT('Ctrl Pts',(-45.9338058653248,3.7316586343443,2.01867272098968));
#26776=CARTESIAN_POINT('Ctrl Pts',(-45.8148968663299,2.31385014354139,3.5561795836249));
#26777=CARTESIAN_POINT('Ctrl Pts',(-45.6959878673349,0.333772012288686,
4.22952857438387));
#26778=CARTESIAN_POINT('Ctrl Pts',(-45.57707886834,-1.7274133029682,3.87509470833104));
#26779=CARTESIAN_POINT('Ctrl Pts',(-45.458169869345,-3.36883415789558,2.57900603610148));
#26780=CARTESIAN_POINT('Ctrl Pts',(-45.3665393568737,-4.00286950955251,
1.09731510772082));
#26781=CARTESIAN_POINT('Ctrl Pts',(-45.3145451774007,-4.07052107660754,
0.21082207709823));
#26782=CARTESIAN_POINT('Ctrl Pts',(-45.3021873309261,-4.07033855687931,
9.5042013614384E-5));
#26783=CARTESIAN_POINT('Origin',(-55.3478126690739,0.,0.));
#26784=CARTESIAN_POINT('',(-48.5978126690739,-4.07016989220343,3.24954791586653E-5));
#26785=CARTESIAN_POINT('',(-48.3021873309261,-4.07078561771882,5.53476569591441E-5));
#26786=CARTESIAN_POINT('',(-55.3478126690739,-4.0705,-3.42898509504556E-13));
#26787=CARTESIAN_POINT('Ctrl Pts',(-48.5978126690739,-4.07016989220343,
3.24954791586923E-5));
#26788=CARTESIAN_POINT('Ctrl Pts',(-48.5759064574397,-4.0700653077914,-0.373558418857458));
#26789=CARTESIAN_POINT('Ctrl Pts',(-48.5143639128072,-3.92681617951824,
-1.42319027041692));
#26790=CARTESIAN_POINT('Ctrl Pts',(-48.4131850351763,-3.03590383707744,
-2.96371451156447));
#26791=CARTESIAN_POINT('Ctrl Pts',(-48.2942760361814,-1.2511421580073,-4.05400531752194));
#26792=CARTESIAN_POINT('Ctrl Pts',(-48.1753670371864,0.837649258381883,
-4.15916572571611));
#26793=CARTESIAN_POINT('Ctrl Pts',(-48.0564580381915,2.72289043680534,-3.25364157263724));
#26794=CARTESIAN_POINT('Ctrl Pts',(-47.9375490391965,3.94646446657405,-1.55747681462926));
#26795=CARTESIAN_POINT('Ctrl Pts',(-47.8186400402015,4.21104071385062,0.517157539180999));
#26796=CARTESIAN_POINT('Ctrl Pts',(-47.6997310412066,3.45232668681426,2.46612170452907));
#26797=CARTESIAN_POINT('Ctrl Pts',(-47.5808220422116,1.85469122386101,3.81581397321361));
#26798=CARTESIAN_POINT('Ctrl Pts',(-47.4619130432167,-0.193637457276558,
4.23825675828857));
#26799=CARTESIAN_POINT('Ctrl Pts',(-47.3430040442216,-2.19491189690037,
3.6307957225496));
#26800=CARTESIAN_POINT('Ctrl Pts',(-47.2240950452268,-3.66281889847391,
2.14104496240076));
#26801=CARTESIAN_POINT('Ctrl Pts',(-47.1423645868441,-4.05998621113554,
0.759479672593957));
#26802=CARTESIAN_POINT('Ctrl Pts',(-47.1002704614598,-4.0708338695703,0.0419391914783086));
#26803=CARTESIAN_POINT('Ctrl Pts',(-47.0978126690739,-4.07081123287269,
4.27420414080091E-5));
#26804=CARTESIAN_POINT('Ctrl Pts',(-48.3021873309261,-4.07078561771882,
5.53476569592308E-5));
#26805=CARTESIAN_POINT('Ctrl Pts',(-48.2658171693605,-4.07036989113885,
-0.6199353689415));
#26806=CARTESIAN_POINT('Ctrl Pts',(-48.1898106747964,-3.76994384664287,
-1.91598331380283));
#26807=CARTESIAN_POINT('Ctrl Pts',(-48.0741678472342,-2.45017226913454,
-3.46366447123714));
#26808=CARTESIAN_POINT('Ctrl Pts',(-47.9552588482392,-0.497729416154917,
-4.21338120113056));
#26809=CARTESIAN_POINT('Ctrl Pts',(-47.8363498492442,1.57566255733915,-3.93923891419978));
#26810=CARTESIAN_POINT('Ctrl Pts',(-47.7174408502492,3.26616576767762,-2.70785466666829));
#26811=CARTESIAN_POINT('Ctrl Pts',(-47.5985318512543,4.16298497174054,-0.818456988979114));
#26812=CARTESIAN_POINT('Ctrl Pts',(-47.4796228522594,4.04819153105236,1.26982717157192));
#26813=CARTESIAN_POINT('Ctrl Pts',(-47.3607138532644,2.94968045290301,3.04954110375778));
#26814=CARTESIAN_POINT('Ctrl Pts',(-47.2418048542694,1.13439185468392,4.08821120268671));
#26815=CARTESIAN_POINT('Ctrl Pts',(-47.1228958552744,-0.956555952514039,
4.13343881380338));
#26816=CARTESIAN_POINT('Ctrl Pts',(-47.0039868562795,-2.81505898666,3.17423354833433));
#26817=CARTESIAN_POINT('Ctrl Pts',(-46.8970840148301,-3.8709155012229,1.61841633454085));
#26818=CARTESIAN_POINT('Ctrl Pts',(-46.8298175063789,-4.06993439401099,
0.471049354774862));
#26819=CARTESIAN_POINT('Ctrl Pts',(-46.8021873309261,-4.07035480316255,
-9.73195009796278E-5));
#26820=CARTESIAN_POINT('Origin',(-55.3478126690739,0.,0.));
#26821=CARTESIAN_POINT('',(-50.0978126690739,-4.07063454056454,-9.39916809451252E-5));
#26822=CARTESIAN_POINT('',(-49.8021873309261,-4.07016024360026,2.01151063877747E-5));
#26823=CARTESIAN_POINT('',(-55.3478126690739,-4.0705,-3.42898509504556E-13));
#26824=CARTESIAN_POINT('Ctrl Pts',(-50.0978126690739,-4.07063454056454,
-9.39916809453677E-5));
#26825=CARTESIAN_POINT('Ctrl Pts',(-50.0911787864178,-4.07074638038891,
-0.113191851380465));
#26826=CARTESIAN_POINT('Ctrl Pts',(-50.0449085707635,-4.03852758336781,
-0.901966869774806));
#26827=CARTESIAN_POINT('Ctrl Pts',(-49.9590020221109,-3.54546957514818,
-2.33022773676946));
#26828=CARTESIAN_POINT('Ctrl Pts',(-49.8400930231158,-2.00143969166412,
-3.74092969395146));
#26829=CARTESIAN_POINT('Ctrl Pts',(-49.721184024121,0.0289435448964663,
-4.2425791784024));
#26830=CARTESIAN_POINT('Ctrl Pts',(-49.6022750251259,2.05229344931449,-3.71327448649327));
#26831=CARTESIAN_POINT('Ctrl Pts',(-49.4833660261311,3.57693244841941,-2.28163758591345));
#26832=CARTESIAN_POINT('Ctrl Pts',(-49.364457027136,4.23237059313566,-0.295558752875362));
#26833=CARTESIAN_POINT('Ctrl Pts',(-49.2455480281411,3.85933526548734,1.76234137516302));
#26834=CARTESIAN_POINT('Ctrl Pts',(-49.1266390291461,2.54847470392539,3.39198946010828));
#26835=CARTESIAN_POINT('Ctrl Pts',(-49.0077300301511,0.618330322503512,
4.19737816098522));
#26836=CARTESIAN_POINT('Ctrl Pts',(-48.8888210311563,-1.46206941105725,
3.98279661184051));
#26837=CARTESIAN_POINT('Ctrl Pts',(-48.7699120321612,-3.18718371510779,
2.80038850522416));
#26838=CARTESIAN_POINT('Ctrl Pts',(-48.6729092448004,-3.96267664484684,
1.28067835687247));
#26839=CARTESIAN_POINT('Ctrl Pts',(-48.615542790438,-4.0702545391679,0.302403912424053));
#26840=CARTESIAN_POINT('Ctrl Pts',(-48.5978126690739,-4.07016989220343,
3.24954791586923E-5));
#26841=CARTESIAN_POINT('Ctrl Pts',(-49.8021873309261,-4.07016024360026,
2.01151063877747E-5));
#26842=CARTESIAN_POINT('Ctrl Pts',(-49.7810894983386,-4.07009807335129,
-0.359787051715212));
#26843=CARTESIAN_POINT('Ctrl Pts',(-49.7203553327528,-3.93407799572834,
-1.39560723718365));
#26844=CARTESIAN_POINT('Ctrl Pts',(-49.6199848341687,-3.06585324049081,
-2.93272222099405));
#26845=CARTESIAN_POINT('Ctrl Pts',(-49.5010758351736,-1.29225906223574,
-4.04108676395591));
#26846=CARTESIAN_POINT('Ctrl Pts',(-49.3821668361788,0.795356333133346,
-4.167460140312));
#26847=CARTESIAN_POINT('Ctrl Pts',(-49.2632578371837,2.68969874550031,-3.28113339811124));
#26848=CARTESIAN_POINT('Ctrl Pts',(-49.1443488381888,3.93043964837605,-1.59748548920479));
#26849=CARTESIAN_POINT('Ctrl Pts',(-49.0254398391938,4.216076827669,0.474354193550262));
#26850=CARTESIAN_POINT('Ctrl Pts',(-48.9065308401989,3.47719994816421,2.43092497585451));
#26851=CARTESIAN_POINT('Ctrl Pts',(-48.7876218412039,1.89335738663818,3.79677672825371));
#26852=CARTESIAN_POINT('Ctrl Pts',(-48.6687128422089,-0.150574338398622,
4.24000508093589));
#26853=CARTESIAN_POINT('Ctrl Pts',(-48.549803843214,-2.15791623528735,3.65290476733649));
#26854=CARTESIAN_POINT('Ctrl Pts',(-48.430894844219,-3.64088070474142,2.17814219269265));
#26855=CARTESIAN_POINT('Ctrl Pts',(-48.3483560067898,-4.0561286694033,0.787058534453424));
#26856=CARTESIAN_POINT('Ctrl Pts',(-48.3054535023588,-4.07082295146222,
0.0557327458286881));
#26857=CARTESIAN_POINT('Ctrl Pts',(-48.3021873309261,-4.07078561771882,
5.53476569592308E-5));
#26858=CARTESIAN_POINT('Origin',(-55.3478126690739,0.,0.));
#26859=CARTESIAN_POINT('',(-51.5978126690739,-4.07052776695671,0.0001044975750702));
#26860=CARTESIAN_POINT('',(-51.3021873309261,-4.07067545460402,-8.7070919803367E-5));
#26861=CARTESIAN_POINT('',(-55.3478126690739,-4.0705,-3.42898509504556E-13));
#26862=CARTESIAN_POINT('Ctrl Pts',(-51.5978126690739,-4.07052776695671,
0.00010449757507032));
#26863=CARTESIAN_POINT('Ctrl Pts',(-51.5668147823977,-4.0699845460846,-0.528403488877145));
#26864=CARTESIAN_POINT('Ctrl Pts',(-51.4961805627232,-3.83428485658603,
-1.73317487318012));
#26865=CARTESIAN_POINT('Ctrl Pts',(-51.3859100100504,-2.67824533662262,
-3.29048853499884));
#26866=CARTESIAN_POINT('Ctrl Pts',(-51.2670010110555,-0.78082496558402,
-4.17020743213141));
#26867=CARTESIAN_POINT('Ctrl Pts',(-51.1480920120604,1.30633725885353,-4.03655767907646));
#26868=CARTESIAN_POINT('Ctrl Pts',(-51.0291830130655,3.07605723061235,-2.9220178035111));
#26869=CARTESIAN_POINT('Ctrl Pts',(-50.9102740140706,4.09828990837908,-1.0974222453584));
#26870=CARTESIAN_POINT('Ctrl Pts',(-50.7913650150755,4.12463095289654,0.993848724235651));
#26871=CARTESIAN_POINT('Ctrl Pts',(-50.6724560160807,3.14867944761336,2.84361277085736));
#26872=CARTESIAN_POINT('Ctrl Pts',(-50.5535470170857,1.40759331717813,4.00237390050092));
#26873=CARTESIAN_POINT('Ctrl Pts',(-50.4346380180907,-0.675540456184353,
4.18855117202478));
#26874=CARTESIAN_POINT('Ctrl Pts',(-50.3157290190957,-2.59451671479358,
3.35690315989496));
#26875=CARTESIAN_POINT('Ctrl Pts',(-50.2034539027568,-3.81113576375281,
1.80142850771877));
#26876=CARTESIAN_POINT('Ctrl Pts',(-50.1308151194162,-4.07007815625064,
0.56254883637138));
#26877=CARTESIAN_POINT('Ctrl Pts',(-50.0978126690739,-4.07063454056454,
-9.39916809453677E-5));
#26878=CARTESIAN_POINT('Ctrl Pts',(-51.3021873309261,-4.07067545460402,
-8.70709198036793E-5));
#26879=CARTESIAN_POINT('Ctrl Pts',(-51.2963618273168,-4.07076913219396,
-0.0994003816391395));
#26880=CARTESIAN_POINT('Ctrl Pts',(-51.2508999907091,-4.04297867155526,
-0.874382431947933));
#26881=CARTESIAN_POINT('Ctrl Pts',(-51.1658018211031,-3.56895759144185,
-2.29409186145612));
#26882=CARTESIAN_POINT('Ctrl Pts',(-51.0468928221082,-2.03933759109846,
-3.72040560679174));
#26883=CARTESIAN_POINT('Ctrl Pts',(-50.9279838231133,-0.0141549843878351,
-4.24265428344519));
#26884=CARTESIAN_POINT('Ctrl Pts',(-50.8090748241182,2.01446730968869,-3.73393052561418));
#26885=CARTESIAN_POINT('Ctrl Pts',(-50.6901658251233,3.55357051600268,-2.31785510914493));
#26886=CARTESIAN_POINT('Ctrl Pts',(-50.5712568261283,4.22914985879238,-0.338536836715756));
#26887=CARTESIAN_POINT('Ctrl Pts',(-50.4523478271334,3.87703837313768,1.72304647947545));
#26888=CARTESIAN_POINT('Ctrl Pts',(-50.3334388281384,2.58279976746683,3.36592648157085));
#26889=CARTESIAN_POINT('Ctrl Pts',(-50.2145298291435,0.660936291289855,
4.19088044882765));
#26890=CARTESIAN_POINT('Ctrl Pts',(-50.0956208301485,-1.42153586209668,
3.99744312162439));
#26891=CARTESIAN_POINT('Ctrl Pts',(-49.9767118311536,-3.15857230942583,
2.83262010934112));
#26892=CARTESIAN_POINT('Ctrl Pts',(-49.8789006647461,-3.9560537057885,1.30826769936161));
#26893=CARTESIAN_POINT('Ctrl Pts',(-49.8207258313369,-4.07021487211157,
0.316179857216054));
#26894=CARTESIAN_POINT('Ctrl Pts',(-49.8021873309261,-4.07016024360026,
2.01151063877747E-5));
#26895=CARTESIAN_POINT('Origin',(41.25,0.,0.));
#26896=CARTESIAN_POINT('',(30.4838415259036,-4.92503358063389,0.00012643715616531));
#26897=CARTESIAN_POINT('',(30.2661584740964,-4.92498881568011,8.60120194096941E-5));
#26898=CARTESIAN_POINT('',(41.25,-4.925,-6.03138548580071E-16));
#26899=CARTESIAN_POINT('',(30.,2.16839587231054,4.42195480991683));
#26900=CARTESIAN_POINT('Ctrl Pts',(30.4838415259036,-4.92503358063389,0.00012643715616531));
#26901=CARTESIAN_POINT('Ctrl Pts',(30.4752030795814,-4.92521674395344,0.178328850711965));
#26902=CARTESIAN_POINT('Ctrl Pts',(30.4665646332593,-4.91573150459355,0.356511818192306));
#26903=CARTESIAN_POINT('Ctrl Pts',(30.4579261869371,-4.89642930393968,0.533624834627407));
#26904=CARTESIAN_POINT('Ctrl Pts',(30.4182898539388,-4.80786378831494,1.34628375915699));
#26905=CARTESIAN_POINT('Ctrl Pts',(30.3786535209405,-4.51262099257391,2.1364169177937));
#26906=CARTESIAN_POINT('Ctrl Pts',(30.3390171879422,-4.04657309347359,2.80802694357323));
#26907=CARTESIAN_POINT('Ctrl Pts',(30.2993808549439,-3.58052519437327,3.47963696935275));
#26908=CARTESIAN_POINT('Ctrl Pts',(30.2597445219455,-2.94367219191368,4.0327238622751));
#26909=CARTESIAN_POINT('Ctrl Pts',(30.2201081889472,-2.21339244687115,4.40007809567974));
#26910=CARTESIAN_POINT('Ctrl Pts',(30.1804718559489,-1.48311270182864,4.76743232908437));
#26911=CARTESIAN_POINT('Ctrl Pts',(30.1408355229506,-0.659406214203193,
4.94905390297128));
#26912=CARTESIAN_POINT('Ctrl Pts',(30.1011991899523,0.157646280266308,4.92289355924806));
#26913=CARTESIAN_POINT('Ctrl Pts',(30.0674661266348,0.853010393055609,4.90062942771858));
#26914=CARTESIAN_POINT('Ctrl Pts',(30.0337330633174,1.54355495045357,4.72786672521511));
#26915=CARTESIAN_POINT('Ctrl Pts',(30.,2.16858287139683,4.42210505377544));
#26916=CARTESIAN_POINT('',(30.,-2.1683958723106,4.4219548099168));
#26917=CARTESIAN_POINT('Origin',(30.,0.,0.));
#26918=CARTESIAN_POINT('Ctrl Pts',(30.,-2.16839587231058,4.42195480991681));
#26919=CARTESIAN_POINT('Ctrl Pts',(30.0396363329983,-2.90256543874867,4.06193976546855));
#26920=CARTESIAN_POINT('Ctrl Pts',(30.0792726659967,-3.54497553128948,3.51573257344795));
#26921=CARTESIAN_POINT('Ctrl Pts',(30.118908998995,-4.01781928837785,2.8490123239199));
#26922=CARTESIAN_POINT('Ctrl Pts',(30.1585453319933,-4.49066304546624,2.18229207439182));
#26923=CARTESIAN_POINT('Ctrl Pts',(30.1981816649916,-4.79394046710217,1.39505876735627));
#26924=CARTESIAN_POINT('Ctrl Pts',(30.2378179979899,-4.89076229523027,0.583305050522158));
#26925=CARTESIAN_POINT('Ctrl Pts',(30.2472648233587,-4.91383856977503,0.38983368157004));
#26926=CARTESIAN_POINT('Ctrl Pts',(30.2567116487276,-4.92518718095595,0.194969436276938));
#26927=CARTESIAN_POINT('Ctrl Pts',(30.2661584740964,-4.92498881568011,8.60120194096941E-5));
#26928=CARTESIAN_POINT('Origin',(41.25,0.,0.));
#26929=CARTESIAN_POINT('',(31.9838415259036,-4.92516276786698,-0.000113722890940915));
#26930=CARTESIAN_POINT('',(31.7661584740964,-4.9252122991162,-0.000105349299657425));
#26931=CARTESIAN_POINT('',(41.25,-4.925,-6.03138548580071E-16));
#26932=CARTESIAN_POINT('Ctrl Pts',(31.9838415259036,-4.92516276786698,-0.000113722890940915));
#26933=CARTESIAN_POINT('Ctrl Pts',(31.9508390755613,-4.92448958453899,0.680641938350505));
#26934=CARTESIAN_POINT('Ctrl Pts',(31.917836625219,-4.78214555510203,1.36167034280227));
#26935=CARTESIAN_POINT('Ctrl Pts',(31.8848341748767,-4.50788725221071,1.9846227453206));
#26936=CARTESIAN_POINT('Ctrl Pts',(31.8451978418784,-4.17849978830403,2.73279594495346));
#26937=CARTESIAN_POINT('Ctrl Pts',(31.80556150888,-3.65883529870816,3.39719861223649));
#26938=CARTESIAN_POINT('Ctrl Pts',(31.7659251758817,-3.012033474306,3.8971052419689));
#26939=CARTESIAN_POINT('Ctrl Pts',(31.7262888428834,-2.36523164990384,4.39701187170132));
#26940=CARTESIAN_POINT('Ctrl Pts',(31.6866525098851,-1.59129249069541,4.73242246388312));
#26941=CARTESIAN_POINT('Ctrl Pts',(31.6470161768868,-0.784250282821528,
4.86258433535561));
#26942=CARTESIAN_POINT('Ctrl Pts',(31.6073798438885,0.0227919250523556,
4.99274620682809));
#26943=CARTESIAN_POINT('Ctrl Pts',(31.5677435108901,0.862937181591687,4.91765935759125));
#26944=CARTESIAN_POINT('Ctrl Pts',(31.5281071778918,1.63410710193199,4.64644691014962));
#26945=CARTESIAN_POINT('Ctrl Pts',(31.4884708448935,2.40527702227229,4.37523446270799));
#26946=CARTESIAN_POINT('Ctrl Pts',(31.4488345118952,3.10747160641356,3.90789641706156));
#26947=CARTESIAN_POINT('Ctrl Pts',(31.4091981788969,3.65537359683798,3.301214746304));
#26948=CARTESIAN_POINT('Ctrl Pts',(31.3695618458985,4.2032755872624,2.69453307554644));
#26949=CARTESIAN_POINT('Ctrl Pts',(31.3299255129002,4.59688498396996,1.94850777967776));
#26950=CARTESIAN_POINT('Ctrl Pts',(31.2902891799019,4.78837790063976,1.15378160391619));
#26951=CARTESIAN_POINT('Ctrl Pts',(31.2506528469036,4.97987081730956,0.35905542815461));
#26952=CARTESIAN_POINT('Ctrl Pts',(31.2110165139052,4.9692472539416,-0.484371627499863));
#26953=CARTESIAN_POINT('Ctrl Pts',(31.1713801809069,4.75779798214507,-1.27402247248995));
#26954=CARTESIAN_POINT('Ctrl Pts',(31.1317438479086,4.54634871034855,-2.06367331748002));
#26955=CARTESIAN_POINT('Ctrl Pts',(31.0921075149103,4.13407373012347,-2.79954795180571));
#26956=CARTESIAN_POINT('Ctrl Pts',(31.052471181912,3.57106481416884,-3.39223689097617));
#26957=CARTESIAN_POINT('Ctrl Pts',(31.0128348489136,3.00805589821421,-3.98492583014663));
#26958=CARTESIAN_POINT('Ctrl Pts',(30.9731985159153,2.29431304653003,-4.43442907416186));
#26959=CARTESIAN_POINT('Ctrl Pts',(30.933562182917,1.516556638511,-4.68613172760538));
#26960=CARTESIAN_POINT('Ctrl Pts',(30.8939258499187,0.738800230491954,-4.9378343810489));
#26961=CARTESIAN_POINT('Ctrl Pts',(30.8542895169203,-0.102969733861949,
-4.99173644392069));
#26962=CARTESIAN_POINT('Ctrl Pts',(30.814653183922,-0.906477461021434,-4.84128848378581));
#26963=CARTESIAN_POINT('Ctrl Pts',(30.7750168509237,-1.70998518818092,-4.69084052365093));
#26964=CARTESIAN_POINT('Ctrl Pts',(30.7353805179254,-2.47523067814598,-4.33604254050938));
#26965=CARTESIAN_POINT('Ctrl Pts',(30.6957441849271,-3.10923594354023,-3.82000336783515));
#26966=CARTESIAN_POINT('Ctrl Pts',(30.6561078519288,-3.74324120893447,-3.30396419516092));
#26967=CARTESIAN_POINT('Ctrl Pts',(30.6164715189305,-4.24600624975789,-2.62668383295402));
#26968=CARTESIAN_POINT('Ctrl Pts',(30.5768351859321,-4.55644465241538,-1.87045130663933));
#26969=CARTESIAN_POINT('Ctrl Pts',(30.5458372992559,-4.799225295769,-1.27903407960837));
#26970=CARTESIAN_POINT('Ctrl Pts',(30.5148394125798,-4.92437632403811,-0.639328623954206));
#26971=CARTESIAN_POINT('Ctrl Pts',(30.4838415259036,-4.92503358063389,0.00012643715616531));
#26972=CARTESIAN_POINT('Ctrl Pts',(30.2661584740964,-4.92498881568011,8.60120194096941E-5));
#26973=CARTESIAN_POINT('Ctrl Pts',(30.2963479817259,-4.92435489372491,-0.622708884020471));
#26974=CARTESIAN_POINT('Ctrl Pts',(30.3265374893554,-4.80579524376599,-1.24569964894004));
#26975=CARTESIAN_POINT('Ctrl Pts',(30.3567269969849,-4.57520694706496,-1.82405290111985));
#26976=CARTESIAN_POINT('Ctrl Pts',(30.3963633299832,-4.27246353615129,-2.58338300929506));
#26977=CARTESIAN_POINT('Ctrl Pts',(30.4359996629815,-3.77661047970369,-3.26576909901281));
#26978=CARTESIAN_POINT('Ctrl Pts',(30.4756359959799,-3.14788147849495,-3.78823036846191));
#26979=CARTESIAN_POINT('Ctrl Pts',(30.5152723289782,-2.51915247728621,-4.31069163791102));
#26980=CARTESIAN_POINT('Ctrl Pts',(30.5549086619765,-1.75754753131633,-4.6732280870915));
#26981=CARTESIAN_POINT('Ctrl Pts',(30.5945449949748,-0.955608781264278,
-4.83182630983855));
#26982=CARTESIAN_POINT('Ctrl Pts',(30.6341813279731,-0.153670031212227,
-4.99042453258561));
#26983=CARTESIAN_POINT('Ctrl Pts',(30.6738176609715,0.688602522921993,-4.94508452889924));
#26984=CARTESIAN_POINT('Ctrl Pts',(30.7134539939698,1.46887527262288,-4.70129757355756));
#26985=CARTESIAN_POINT('Ctrl Pts',(30.7530903269681,2.24914802232376,-4.45751061821589));
#26986=CARTESIAN_POINT('Ctrl Pts',(30.7927266599664,2.96742096759131,-4.01527671121891));
#26987=CARTESIAN_POINT('Ctrl Pts',(30.8323629929647,3.53642168974787,-3.4283364671891));
#26988=CARTESIAN_POINT('Ctrl Pts',(30.871999325963,4.10542241190442,-2.84139622315928));
#26989=CARTESIAN_POINT('Ctrl Pts',(30.9116356589614,4.52515091094998,-2.10974964209663));
#26990=CARTESIAN_POINT('Ctrl Pts',(30.9512719919597,4.74461062149402,-1.32228801091272));
#26991=CARTESIAN_POINT('Ctrl Pts',(30.990908324958,4.96407033203805,-0.534826379728812));
#26992=CARTESIAN_POINT('Ctrl Pts',(31.0305446579563,4.98326125408056,0.308450301576346));
#26993=CARTESIAN_POINT('Ctrl Pts',(31.0701809909546,4.79985126528465,1.10508096512556));
#26994=CARTESIAN_POINT('Ctrl Pts',(31.109817323953,4.61644127648874,1.90171162867477));
#26995=CARTESIAN_POINT('Ctrl Pts',(31.1494536569513,4.23043037685442,2.65169627446803));
#26996=CARTESIAN_POINT('Ctrl Pts',(31.1890899899496,3.68871943369624,3.26391221939412));
#26997=CARTESIAN_POINT('Ctrl Pts',(31.2287263229479,3.14700849053805,3.87612816432021));
#26998=CARTESIAN_POINT('Ctrl Pts',(31.2683626559463,2.44959750385601,4.35057540837914));
#26999=CARTESIAN_POINT('Ctrl Pts',(31.3079989889446,1.68122241712191,4.62960764002769));
#27000=CARTESIAN_POINT('Ctrl Pts',(31.3476353219429,0.912847330387817,4.90863987167623));
#27001=CARTESIAN_POINT('Ctrl Pts',(31.3872716549412,0.0735081436016706,
4.99225709091441));
#27002=CARTESIAN_POINT('Ctrl Pts',(31.4269079879395,-0.734814645052458,
4.87030001077229));
#27003=CARTESIAN_POINT('Ctrl Pts',(31.4665443209378,-1.54313743370658,4.74834293063017));
#27004=CARTESIAN_POINT('Ctrl Pts',(31.5061806539362,-2.32044382422869,4.42081155110776));
#27005=CARTESIAN_POINT('Ctrl Pts',(31.5458169869345,-2.97229043473293,3.9275010823073));
#27006=CARTESIAN_POINT('Ctrl Pts',(31.5854533199328,-3.62413704523717,3.43419061350684));
#27007=CARTESIAN_POINT('Ctrl Pts',(31.6250896529311,-4.15052387572353,2.77510105542834));
#27008=CARTESIAN_POINT('Ctrl Pts',(31.6647259859294,-4.48749445206432,2.03031243692023));
#27009=CARTESIAN_POINT('Ctrl Pts',(31.6985368153184,-4.774939172701,1.39498825311397));
#27010=CARTESIAN_POINT('Ctrl Pts',(31.7323476447074,-4.92455446478589,0.697304835250864));
#27011=CARTESIAN_POINT('Ctrl Pts',(31.7661584740964,-4.9252122991162,-0.000105349299657425));
#27012=CARTESIAN_POINT('Origin',(41.25,0.,0.));
#27013=CARTESIAN_POINT('',(33.4838415259036,-4.9246005781677,3.93170949294919E-5));
#27014=CARTESIAN_POINT('',(33.2661584740964,-4.9245889324042,2.43377721320041E-5));
#27015=CARTESIAN_POINT('',(41.25,-4.925,-6.03138548580071E-16));
#27016=CARTESIAN_POINT('Ctrl Pts',(33.4838415259036,-4.9246005781677,3.93170949294919E-5));
#27017=CARTESIAN_POINT('Ctrl Pts',(33.4661114045395,-4.92470299465183,0.365886073899998));
#27018=CARTESIAN_POINT('Ctrl Pts',(33.4483812831753,-4.88447436734275,0.731710654126898));
#27019=CARTESIAN_POINT('Ctrl Pts',(33.4306511618112,-4.80367402952791,1.08834311566542));
#27020=CARTESIAN_POINT('Ctrl Pts',(33.3910148288129,-4.62304192722966,1.88560799125441));
#27021=CARTESIAN_POINT('Ctrl Pts',(33.3513784958145,-4.23964769810467,2.63693412006481));
#27022=CARTESIAN_POINT('Ctrl Pts',(33.3117421628162,-3.70007407698625,3.25103471900744));
#27023=CARTESIAN_POINT('Ctrl Pts',(33.2721058298179,-3.16050045586783,3.86513531795008));
#27024=CARTESIAN_POINT('Ctrl Pts',(33.2324694968196,-2.46474744275599,4.34201038702495));
#27025=CARTESIAN_POINT('Ctrl Pts',(33.1928331638213,-1.69734963847986,4.62371918742141));
#27026=CARTESIAN_POINT('Ctrl Pts',(33.153196830823,-0.92995183420373,4.90542798781788));
#27027=CARTESIAN_POINT('Ctrl Pts',(33.1135604978246,-0.0909092387633235,
4.99197051953595));
#27028=CARTESIAN_POINT('Ctrl Pts',(33.0739241648263,0.717833737184807,4.87283178912815));
#27029=CARTESIAN_POINT('Ctrl Pts',(33.034287831828,1.52657671313293,4.75369305872036));
#27030=CARTESIAN_POINT('Ctrl Pts',(32.9946514988297,2.30502006958878,4.4288730661867));
#27031=CARTESIAN_POINT('Ctrl Pts',(32.9550151658313,2.95858225653972,3.93783772528318));
#27032=CARTESIAN_POINT('Ctrl Pts',(32.915378832833,3.61214444349066,3.44680238437967));
#27033=CARTESIAN_POINT('Ctrl Pts',(32.8757424998347,4.14082546093669,2.78955169510629));
#27034=CARTESIAN_POINT('Ctrl Pts',(32.8361061668364,4.48039010193867,2.04594219220132));
#27035=CARTESIAN_POINT('Ctrl Pts',(32.7964698338381,4.81995474294064,1.30233268929635));
#27036=CARTESIAN_POINT('Ctrl Pts',(32.7568335008397,4.97040300749856,0.472364372759784));
#27037=CARTESIAN_POINT('Ctrl Pts',(32.7171971678414,4.91345529962058,-0.34312087958652));
#27038=CARTESIAN_POINT('Ctrl Pts',(32.6775608348431,4.8565075917426,-1.15860613193281));
#27039=CARTESIAN_POINT('Ctrl Pts',(32.6379245018448,4.59216391142874,-1.95960832008884));
#27040=CARTESIAN_POINT('Ctrl Pts',(32.5982881688465,4.15254224749944,-2.64880497622958));
#27041=CARTESIAN_POINT('Ctrl Pts',(32.5586518358482,3.71292058357014,-3.33800163237032));
#27042=CARTESIAN_POINT('Ctrl Pts',(32.5190155028498,3.09802093602541,-3.91539275649576));
#27043=CARTESIAN_POINT('Ctrl Pts',(32.4793791698515,2.38255415092096,-4.3108248209992));
#27044=CARTESIAN_POINT('Ctrl Pts',(32.4397428368532,1.66708736581652,-4.70625688550265));
#27045=CARTESIAN_POINT('Ctrl Pts',(32.4001065038549,0.851053443152359,-4.9197298903841));
#27046=CARTESIAN_POINT('Ctrl Pts',(32.3604701708566,0.0336012196779929,
-4.9253066785054));
#27047=CARTESIAN_POINT('Ctrl Pts',(32.3208338378582,-0.783851003796368,
-4.93088346662671));
#27048=CARTESIAN_POINT('Ctrl Pts',(32.2811975048599,-1.60272152808094,-4.72856403798788));
#27049=CARTESIAN_POINT('Ctrl Pts',(32.2415611718616,-2.32351686684147,-4.34293038040315));
#27050=CARTESIAN_POINT('Ctrl Pts',(32.2019248388633,-3.04431220560201,-3.95729672281842));
#27051=CARTESIAN_POINT('Ctrl Pts',(32.1622885058649,-3.66703235883851,-3.3883488362878));
#27052=CARTESIAN_POINT('Ctrl Pts',(32.1226521728666,-4.11601628220298,-2.7052143877759));
#27053=CARTESIAN_POINT('Ctrl Pts',(32.0830158398683,-4.56500020556745,-2.022079939264));
#27054=CARTESIAN_POINT('Ctrl Pts',(32.04337950687,-4.84024789905989,-1.22475892877083));
#27055=CARTESIAN_POINT('Ctrl Pts',(32.0037431738716,-4.90831652669737,-0.410126557532889));
#27056=CARTESIAN_POINT('Ctrl Pts',(31.9971092912156,-4.91970908635527,-0.273782573370168));
#27057=CARTESIAN_POINT('Ctrl Pts',(31.9904754085596,-4.92529808567392,-0.136953658327863));
#27058=CARTESIAN_POINT('Ctrl Pts',(31.9838415259036,-4.92516276786698,-0.000113722890940915));
#27059=CARTESIAN_POINT('Ctrl Pts',(31.7661584740964,-4.9252122991162,-0.000105349299657425));
#27060=CARTESIAN_POINT('Ctrl Pts',(31.7719839777057,-4.92532564198105,-0.12026701408908));
#27061=CARTESIAN_POINT('Ctrl Pts',(31.7778094813151,-4.92101699689922,-0.24042056760678));
#27062=CARTESIAN_POINT('Ctrl Pts',(31.7836349849244,-4.91222944566371,-0.360245654138465));
#27063=CARTESIAN_POINT('Ctrl Pts',(31.8232713179227,-4.85243954072709,-1.17552744775133));
#27064=CARTESIAN_POINT('Ctrl Pts',(31.862907650921,-4.58530540865863,-1.97560335603935));
#27065=CARTESIAN_POINT('Ctrl Pts',(31.9025439839194,-4.14328407736884,-2.66326343741845));
#27066=CARTESIAN_POINT('Ctrl Pts',(31.9421803169177,-3.70126274607906,-3.35092351879755));
#27067=CARTESIAN_POINT('Ctrl Pts',(31.981816649916,-3.08435421556795,-3.92616777326773));
#27068=CARTESIAN_POINT('Ctrl Pts',(32.0214529829144,-2.36751341455751,-4.31910352858822));
#27069=CARTESIAN_POINT('Ctrl Pts',(32.0610893159127,-1.65067261354707,-4.7120392839087));
#27070=CARTESIAN_POINT('Ctrl Pts',(32.100725648911,-0.833899542037295,-4.9226665400795));
#27071=CARTESIAN_POINT('Ctrl Pts',(32.1403619819093,-0.0164328431961262,
-4.92539389647684));
#27072=CARTESIAN_POINT('Ctrl Pts',(32.1799983149076,0.801033855645048,-4.92812125287418));
#27073=CARTESIAN_POINT('Ctrl Pts',(32.2196346479059,1.61919418181762,-4.72294870949805));
#27074=CARTESIAN_POINT('Ctrl Pts',(32.2592709809043,2.33864093827332,-4.33480491238653));
#27075=CARTESIAN_POINT('Ctrl Pts',(32.2989073139026,3.05808769472903,-3.946661115275));
#27076=CARTESIAN_POINT('Ctrl Pts',(32.3385436469009,3.67882088146788,-3.37554606442807));
#27077=CARTESIAN_POINT('Ctrl Pts',(32.3781799798992,4.1254208725147,-2.69085073792278));
#27078=CARTESIAN_POINT('Ctrl Pts',(32.4178163128976,4.57202086356151,-2.0061554114175));
#27079=CARTESIAN_POINT('Ctrl Pts',(32.4574526458959,4.84448765891629,-1.20787980925385));
#27080=CARTESIAN_POINT('Ctrl Pts',(32.4970889788942,4.90971630405955,-0.39301511723372));
#27081=CARTESIAN_POINT('Ctrl Pts',(32.5367253118925,4.9749449492028,0.421849574786424));
#27082=CARTESIAN_POINT('Ctrl Pts',(32.5763616448908,4.83293544413453,1.25330335666306));
#27083=CARTESIAN_POINT('Ctrl Pts',(32.6159979778891,4.50094206822459,2.00032386551657));
#27084=CARTESIAN_POINT('Ctrl Pts',(32.6556343108875,4.16894869231465,2.74734437437008));
#27085=CARTESIAN_POINT('Ctrl Pts',(32.6952706438858,3.64697144556304,3.40993161020045));
#27086=CARTESIAN_POINT('Ctrl Pts',(32.7349069768841,2.99843102086877,3.90758064304421));
#27087=CARTESIAN_POINT('Ctrl Pts',(32.7745433098824,2.34989059617449,4.40522967588796));
#27088=CARTESIAN_POINT('Ctrl Pts',(32.8141796428808,1.57478699353755,4.73794050574509));
#27089=CARTESIAN_POINT('Ctrl Pts',(32.8538159758791,0.767295979967659,4.86528847528057));
#27090=CARTESIAN_POINT('Ctrl Pts',(32.8934523088774,-0.0401950336022416,
4.99263644481604));
#27091=CARTESIAN_POINT('Ctrl Pts',(32.9330886418757,-0.880073458105095,
4.91462155402985));
#27092=CARTESIAN_POINT('Ctrl Pts',(32.972724974874,-1.65029332892724,4.64072268048729));
#27093=CARTESIAN_POINT('Ctrl Pts',(33.0123613078724,-2.42051319974939,4.36682380694472));
#27094=CARTESIAN_POINT('Ctrl Pts',(33.0519976408707,-3.12107451689084,3.89704095064578));
#27095=CARTESIAN_POINT('Ctrl Pts',(33.091633973869,-3.66685846636575,3.28845314035125));
#27096=CARTESIAN_POINT('Ctrl Pts',(33.1312703068673,-4.21264241584066,2.67986533005673));
#27097=CARTESIAN_POINT('Ctrl Pts',(33.1709066398656,-4.60364899764904,1.93247256576663));
#27098=CARTESIAN_POINT('Ctrl Pts',(33.210542972864,-4.79237056943692,1.13708372332491));
#27099=CARTESIAN_POINT('Ctrl Pts',(33.2290814732748,-4.8806384456874,0.765068572907586));
#27100=CARTESIAN_POINT('Ctrl Pts',(33.2476199736856,-4.92465502880973,0.382553937021347));
#27101=CARTESIAN_POINT('Ctrl Pts',(33.2661584740964,-4.9245889324042,2.43377721320041E-5));
#27102=CARTESIAN_POINT('Origin',(41.25,0.,0.));
#27103=CARTESIAN_POINT('',(34.9838415259036,-4.92537655231972,5.17146673368989E-5));
#27104=CARTESIAN_POINT('',(34.7661584740964,-4.92534558823064,6.69665182562415E-5));
#27105=CARTESIAN_POINT('',(41.25,-4.925,-6.03138548580071E-16));
#27106=CARTESIAN_POINT('Ctrl Pts',(34.9838415259036,-4.92537655231972,5.17146673368989E-5));
#27107=CARTESIAN_POINT('Ctrl Pts',(34.9813837335176,-4.92540394102758,0.0507432790454098));
#27108=CARTESIAN_POINT('Ctrl Pts',(34.9789259411317,-4.9246376068758,0.101434013757565));
#27109=CARTESIAN_POINT('Ctrl Pts',(34.9764681487457,-4.92307226133183,0.15210006272951));
#27110=CARTESIAN_POINT('Ctrl Pts',(34.9368318157474,-4.89782824251546,0.969181440404085));
#27111=CARTESIAN_POINT('Ctrl Pts',(34.8971954827491,-4.66478232121914,1.77984270463634));
#27112=CARTESIAN_POINT('Ctrl Pts',(34.8575591497507,-4.25224978111449,2.48558780138401));
#27113=CARTESIAN_POINT('Ctrl Pts',(34.8179228167524,-3.83971724100984,3.19133289813169));
#27114=CARTESIAN_POINT('Ctrl Pts',(34.7782864837541,-3.24769808209686,3.7921618273948));
#27115=CARTESIAN_POINT('Ctrl Pts',(34.7386501507558,-2.54812315101044,4.21507334772028));
#27116=CARTESIAN_POINT('Ctrl Pts',(34.6990138177575,-1.84854821992401,4.63798486804578));
#27117=CARTESIAN_POINT('Ctrl Pts',(34.6593774847591,-1.04141751666414,4.88297897943365));
#27118=CARTESIAN_POINT('Ctrl Pts',(34.6197411517608,-0.224798129020873,
4.92028868264515));
#27119=CARTESIAN_POINT('Ctrl Pts',(34.5801048187625,0.591821258622399,4.95759838585665));
#27120=CARTESIAN_POINT('Ctrl Pts',(34.5404684857642,1.41792933064908,4.78722368089177));
#27121=CARTESIAN_POINT('Ctrl Pts',(34.5008321527659,2.15315323233279,4.42986524371477));
#27122=CARTESIAN_POINT('Ctrl Pts',(34.4611958197675,2.88837713401649,4.07250680653778));
#27123=CARTESIAN_POINT('Ctrl Pts',(34.4215594867692,3.53271686535722,3.52816463714868));
#27124=CARTESIAN_POINT('Ctrl Pts',(34.3819231537709,4.00788458431802,2.8629767861726));
#27125=CARTESIAN_POINT('Ctrl Pts',(34.3422868207726,4.48305230327882,2.19778893519652));
#27126=CARTESIAN_POINT('Ctrl Pts',(34.3026504877742,4.78904800985969,1.41175540263347));
#27127=CARTESIAN_POINT('Ctrl Pts',(34.2630141547759,4.88869295754603,0.600379951544906));
#27128=CARTESIAN_POINT('Ctrl Pts',(34.2233778217776,4.98833790523238,-0.210995499543657));
#27129=CARTESIAN_POINT('Ctrl Pts',(34.1837414887793,4.8816320940242,-1.04771286915773));
#27130=CARTESIAN_POINT('Ctrl Pts',(34.144105155781,4.58154037349691,-1.80811026361641));
#27131=CARTESIAN_POINT('Ctrl Pts',(34.1044688227826,4.28144865296962,-2.5685076580751));
#27132=CARTESIAN_POINT('Ctrl Pts',(34.0648324897843,3.78797102312322,-3.2525850773784));
#27133=CARTESIAN_POINT('Ctrl Pts',(34.025196156786,3.16106544845231,-3.77722651557704));
#27134=CARTESIAN_POINT('Ctrl Pts',(33.9855598237877,2.5341598737814,-4.30186795377567));
#27135=CARTESIAN_POINT('Ctrl Pts',(33.9459234907894,1.77382635428599,-4.66707341086963));
#27136=CARTESIAN_POINT('Ctrl Pts',(33.906287157791,0.972446078917145,-4.82847010376744));
#27137=CARTESIAN_POINT('Ctrl Pts',(33.8666508247927,0.171065803548301,-4.98986679666524));
#27138=CARTESIAN_POINT('Ctrl Pts',(33.8270144917944,-0.671361227693977,
-4.94745472536688));
#27139=CARTESIAN_POINT('Ctrl Pts',(33.7873781587961,-1.4524793922372,-4.70638699370371));
#27140=CARTESIAN_POINT('Ctrl Pts',(33.7477418257978,-2.23359755678042,-4.46531926204055));
#27141=CARTESIAN_POINT('Ctrl Pts',(33.7081054927994,-2.95340685462458,-4.02559587001259));
#27142=CARTESIAN_POINT('Ctrl Pts',(33.6684691598011,-3.5244498252634,-3.44064359511096));
#27143=CARTESIAN_POINT('Ctrl Pts',(33.6288328268028,-4.09549279590221,-2.85569132020933));
#27144=CARTESIAN_POINT('Ctrl Pts',(33.5891964938045,-4.51776943933568,-2.12551016243403));
#27145=CARTESIAN_POINT('Ctrl Pts',(33.5495601608062,-4.73997277331667,-1.33881777236259));
#27146=CARTESIAN_POINT('Ctrl Pts',(33.527653949172,-4.86278012939111,-0.904028560438227));
#27147=CARTESIAN_POINT('Ctrl Pts',(33.5057477375378,-4.92447403886602,-0.451977694839747));
#27148=CARTESIAN_POINT('Ctrl Pts',(33.4838415259036,-4.9246005781677,3.93170949294919E-5));
#27149=CARTESIAN_POINT('Ctrl Pts',(33.2661584740964,-4.9245889324042,2.43377721320041E-5));
#27150=CARTESIAN_POINT('Ctrl Pts',(33.2872563066839,-4.92451371106118,-0.435315375035468));
#27151=CARTESIAN_POINT('Ctrl Pts',(33.3083541392714,-4.86734396438128,-0.870674467928753));
#27152=CARTESIAN_POINT('Ctrl Pts',(33.3294519718589,-4.7533282243701,-1.29059903148261));
#27153=CARTESIAN_POINT('Ctrl Pts',(33.3690883048572,-4.53912774574801,-2.07950802325508));
#27154=CARTESIAN_POINT('Ctrl Pts',(33.4087246378556,-4.12429022673645,-2.81394108620665));
#27155=CARTESIAN_POINT('Ctrl Pts',(33.4483609708539,-3.55921878944626,-3.40466395955689));
#27156=CARTESIAN_POINT('Ctrl Pts',(33.4879973038522,-2.99414735215609,-3.99538683290712));
#27157=CARTESIAN_POINT('Ctrl Pts',(33.5276336368506,-2.2788419965873,-4.44239951665602));
#27158=CARTESIAN_POINT('Ctrl Pts',(33.5672699698489,-1.50021295031243,-4.69138957797913));
#27159=CARTESIAN_POINT('Ctrl Pts',(33.6069063028472,-0.721583904037545,
-4.94037963930225));
#27160=CARTESIAN_POINT('Ctrl Pts',(33.6465426358455,0.120368832943431,-4.99134707819958));
#27161=CARTESIAN_POINT('Ctrl Pts',(33.6861789688438,0.923347265226319,-4.83809930617939));
#27162=CARTESIAN_POINT('Ctrl Pts',(33.7258153018421,1.72632569750921,-4.6848515341592));
#27163=CARTESIAN_POINT('Ctrl Pts',(33.7654516348405,2.49032982509401,-4.32738855122149));
#27164=CARTESIAN_POINT('Ctrl Pts',(33.8050879678388,3.12253247693004,-3.80914242306223));
#27165=CARTESIAN_POINT('Ctrl Pts',(33.8447243008371,3.75473512876605,-3.29089629490298));
#27166=CARTESIAN_POINT('Ctrl Pts',(33.8843606338354,4.25513630485329,-2.61186702152217));
#27167=CARTESIAN_POINT('Ctrl Pts',(33.9239969668337,4.56293682376128,-1.85455725471561));
#27168=CARTESIAN_POINT('Ctrl Pts',(33.963633299832,4.87073734266926,-1.09724748790906));
#27169=CARTESIAN_POINT('Ctrl Pts',(34.0032696328304,4.985937204398,-0.261657227676774));
#27170=CARTESIAN_POINT('Ctrl Pts',(34.0429059658287,4.89453952478992,0.550688577078092));
#27171=CARTESIAN_POINT('Ctrl Pts',(34.082542298827,4.80314184518184,1.36303438183296));
#27172=CARTESIAN_POINT('Ctrl Pts',(34.1221786318253,4.50514662423694,2.1521357311104));
#27173=CARTESIAN_POINT('Ctrl Pts',(34.1618149648236,4.03676054245367,2.82211611942957));
#27174=CARTESIAN_POINT('Ctrl Pts',(34.201451297822,3.5683744606704,3.49209650774873));
#27175=CARTESIAN_POINT('Ctrl Pts',(34.2410876308203,2.92959751804876,4.04295593510963));
#27176=CARTESIAN_POINT('Ctrl Pts',(34.2807239638186,2.19804167292129,4.40776449833205));
#27177=CARTESIAN_POINT('Ctrl Pts',(34.3203602968169,1.4664858277938,4.77257306155448));
#27178=CARTESIAN_POINT('Ctrl Pts',(34.3599966298152,0.64215108016047,4.95133076063843));
#27179=CARTESIAN_POINT('Ctrl Pts',(34.3996329628136,-0.174805175720185,
4.92231837848757));
#27180=CARTESIAN_POINT('Ctrl Pts',(34.4392692958119,-0.991761431600829,
4.8933059963367));
#27181=CARTESIAN_POINT('Ctrl Pts',(34.4789056288102,-1.80133919572881,4.65652353295103));
#27182=CARTESIAN_POINT('Ctrl Pts',(34.5185419618085,-2.50517406027409,4.24074026514061));
#27183=CARTESIAN_POINT('Ctrl Pts',(34.5581782948069,-3.20900892481938,3.82495699733019));
#27184=CARTESIAN_POINT('Ctrl Pts',(34.5978146278052,-3.80710088978197,3.23017292509503));
#27185=CARTESIAN_POINT('Ctrl Pts',(34.6374509608035,-4.22678125726992,2.52865483446174));
#27186=CARTESIAN_POINT('Ctrl Pts',(34.6770872938018,-4.64646162475788,1.82713674382845));
#27187=CARTESIAN_POINT('Ctrl Pts',(34.7167236268002,-4.88773039477119,1.01888463479704));
#27188=CARTESIAN_POINT('Ctrl Pts',(34.7563599597985,-4.92127320031289,0.202101846941553));
#27189=CARTESIAN_POINT('Ctrl Pts',(34.7596261312311,-4.92403724393003,0.134796109842093));
#27190=CARTESIAN_POINT('Ctrl Pts',(34.7628923026638,-4.92539075926287,0.0674324466003896));
#27191=CARTESIAN_POINT('Ctrl Pts',(34.7661584740964,-4.92534558823064,6.69665182562415E-5));
#27192=CARTESIAN_POINT('Origin',(41.25,0.,0.));
#27193=CARTESIAN_POINT('',(36.4838415259036,-4.92478004438697,-0.000110922936420454));
#27194=CARTESIAN_POINT('',(36.2661584740964,-4.92482433489693,-0.000117749303896287));
#27195=CARTESIAN_POINT('',(41.25,-4.925,-6.03138548580071E-16));
#27196=CARTESIAN_POINT('Ctrl Pts',(36.4838415259036,-4.92478004438697,-0.000110922936420454));
#27197=CARTESIAN_POINT('Ctrl Pts',(36.4570197294975,-4.92432112113983,0.553277444647099));
#27198=CARTESIAN_POINT('Ctrl Pts',(36.4301979330913,-4.83122563981592,1.10681634663209));
#27199=CARTESIAN_POINT('Ctrl Pts',(36.4033761366852,-4.64828496666694,1.62887132335118));
#27200=CARTESIAN_POINT('Ctrl Pts',(36.3637398036869,-4.37794149935855,2.40034630539035));
#27201=CARTESIAN_POINT('Ctrl Pts',(36.3241034706886,-3.91139484670805,3.10306695234755));
#27202=CARTESIAN_POINT('Ctrl Pts',(36.2844671376903,-3.3053308358794,3.65165208977549));
#27203=CARTESIAN_POINT('Ctrl Pts',(36.244830804692,-2.69926682505073,4.20023722720345));
#27204=CARTESIAN_POINT('Ctrl Pts',(36.2051944716936,-1.95368545604391,4.59468685510214));
#27205=CARTESIAN_POINT('Ctrl Pts',(36.1655581386953,-1.15917551859725,4.78707499799849));
#27206=CARTESIAN_POINT('Ctrl Pts',(36.125921805697,-0.364665581150601,4.97946314089483));
#27207=CARTESIAN_POINT('Ctrl Pts',(36.0862854726987,0.478772924735871,4.96978979878885));
#27208=CARTESIAN_POINT('Ctrl Pts',(36.0466491397003,1.26866148143396,4.75923029122388));
#27209=CARTESIAN_POINT('Ctrl Pts',(36.007012806702,2.05855003813205,4.54867078365892));
#27210=CARTESIAN_POINT('Ctrl Pts',(35.9673764737037,2.79488864564176,4.13722511063498));
#27211=CARTESIAN_POINT('Ctrl Pts',(35.9277401407054,3.38821151784667,3.57488428200248));
#27212=CARTESIAN_POINT('Ctrl Pts',(35.8881038077071,3.98153439005161,3.01254345336996));
#27213=CARTESIAN_POINT('Ctrl Pts',(35.8484674747088,4.43184152695175,2.29930746912889));
#27214=CARTESIAN_POINT('Ctrl Pts',(35.8088311417104,4.6844202167787,1.52183512642213));
#27215=CARTESIAN_POINT('Ctrl Pts',(35.7691948087121,4.93699890660564,0.744362783715409));
#27216=CARTESIAN_POINT('Ctrl Pts',(35.7295584757138,4.99184914935941,-0.0973459174569996));
#27217=CARTESIAN_POINT('Ctrl Pts',(35.6899221427155,4.8423065924764,-0.901022632255597));
#27218=CARTESIAN_POINT('Ctrl Pts',(35.6502858097171,4.69276403559339,-1.7046993470542));
#27219=CARTESIAN_POINT('Ctrl Pts',(35.6106494767188,4.33882867907361,-2.470344075479));
#27220=CARTESIAN_POINT('Ctrl Pts',(35.5710131437205,3.82350397891201,-3.10493031203944));
#27221=CARTESIAN_POINT('Ctrl Pts',(35.5313768107222,3.3081792787504,-3.73951654859988));
#27222=CARTESIAN_POINT('Ctrl Pts',(35.4917404777239,2.63146523494698,-4.24304429329594));
#27223=CARTESIAN_POINT('Ctrl Pts',(35.4521041447255,1.87558319687476,-4.55433448387119));
#27224=CARTESIAN_POINT('Ctrl Pts',(35.4124678117272,1.11970115880254,-4.86562467444645));
#27225=CARTESIAN_POINT('Ctrl Pts',(35.3728314787289,0.28465112646151,-4.98467731090088));
#27226=CARTESIAN_POINT('Ctrl Pts',(35.3331951457306,-0.528107589407301,
-4.89702739357129));
#27227=CARTESIAN_POINT('Ctrl Pts',(35.2935588127323,-1.34086630527611,-4.8093774762417));
#27228=CARTESIAN_POINT('Ctrl Pts',(35.2539224797339,-2.13133370467271,-4.5150250051281));
#27229=CARTESIAN_POINT('Ctrl Pts',(35.2142861467356,-2.80346730582963,-4.04973406343202));
#27230=CARTESIAN_POINT('Ctrl Pts',(35.1746498137373,-3.47560090698655,-3.58444312173594));
#27231=CARTESIAN_POINT('Ctrl Pts',(35.135013480739,-4.0294007099038,-2.9482137094574));
#27232=CARTESIAN_POINT('Ctrl Pts',(35.0953771477407,-4.39757955319421,-2.21834825775968));
#27233=CARTESIAN_POINT('Ctrl Pts',(35.0581986071283,-4.74292815238131,-1.53374072005811));
#27234=CARTESIAN_POINT('Ctrl Pts',(35.0210200665159,-4.9249622487385,-0.766749580550754));
#27235=CARTESIAN_POINT('Ctrl Pts',(34.9838415259036,-4.92537655231972,5.17146673368989E-5));
#27236=CARTESIAN_POINT('Ctrl Pts',(34.7661584740964,-4.92534558823064,6.69665182562415E-5));
#27237=CARTESIAN_POINT('Ctrl Pts',(34.8025286356621,-4.92484259021781,-0.750075346909099));
#27238=CARTESIAN_POINT('Ctrl Pts',(34.8388987972277,-4.75090614755571,-1.50044294378959));
#27239=CARTESIAN_POINT('Ctrl Pts',(34.8752689587934,-4.41988712998175,-2.17356224361685));
#27240=CARTESIAN_POINT('Ctrl Pts',(34.9149052917917,-4.05914141303884,-2.90713007964017));
#27241=CARTESIAN_POINT('Ctrl Pts',(34.9545416247901,-3.51183313808295,-3.54895228500724));
#27242=CARTESIAN_POINT('Ctrl Pts',(34.9941779577884,-2.84446074016496,-4.02104689929317));
#27243=CARTESIAN_POINT('Ctrl Pts',(35.0338142907867,-2.17708834224698,-4.4931415135791));
#27244=CARTESIAN_POINT('Ctrl Pts',(35.073450623785,-1.3896518213669,-4.7955085367839));
#27245=CARTESIAN_POINT('Ctrl Pts',(35.1130869567833,-0.577825404896259,
-4.89141011060323));
#27246=CARTESIAN_POINT('Ctrl Pts',(35.1527232897817,0.234001011574379,-4.98731168442256));
#27247=CARTESIAN_POINT('Ctrl Pts',(35.19235962278,1.07021732363557,-4.87674780885642));
#27248=CARTESIAN_POINT('Ctrl Pts',(35.2319959557783,1.82922251653823,-4.57315209168081));
#27249=CARTESIAN_POINT('Ctrl Pts',(35.2716322887766,2.5882277094409,-4.26955637450519));
#27250=CARTESIAN_POINT('Ctrl Pts',(35.3112686217749,3.27002178318504,-3.77292881572008));
#27251=CARTESIAN_POINT('Ctrl Pts',(35.3509049547733,3.79176616030783,-3.14361009894666));
#27252=CARTESIAN_POINT('Ctrl Pts',(35.3905412877716,4.31351053743063,-2.51429138217323));
#27253=CARTESIAN_POINT('Ctrl Pts',(35.4301776207699,4.67520521793209,-1.75228150741147));
#27254=CARTESIAN_POINT('Ctrl Pts',(35.4698139537682,4.83290398115343,-0.950165342246432));
#27255=CARTESIAN_POINT('Ctrl Pts',(35.5094502867666,4.99060274437478,-0.148049177081417));
#27256=CARTESIAN_POINT('Ctrl Pts',(35.5490866197649,4.94430559031603,0.694173278486871));
#27257=CARTESIAN_POINT('Ctrl Pts',(35.5887229527632,4.6996376637687,1.47417125800964));
#27258=CARTESIAN_POINT('Ctrl Pts',(35.6283592857615,4.45496973722136,2.25416923753242));
#27259=CARTESIAN_POINT('Ctrl Pts',(35.6679956187598,4.01193103818541,2.97194274100968));
#27260=CARTESIAN_POINT('Ctrl Pts',(35.7076319517581,3.42435115685893,3.54028165873479));
#27261=CARTESIAN_POINT('Ctrl Pts',(35.7472682847565,2.83677127553244,4.1086205764599));
#27262=CARTESIAN_POINT('Ctrl Pts',(35.7869046177548,2.10465021191539,4.52752490843288));
#27263=CARTESIAN_POINT('Ctrl Pts',(35.8265409507531,1.31694131684514,4.74609741120441));
#27264=CARTESIAN_POINT('Ctrl Pts',(35.8661772837514,0.529232421774926,4.96466991397594));
#27265=CARTESIAN_POINT('Ctrl Pts',(35.9058136167498,-0.314064304748486,
4.98291058754604));
#27266=CARTESIAN_POINT('Ctrl Pts',(35.9454499497481,-1.1104875714138,4.7986031740904));
#27267=CARTESIAN_POINT('Ctrl Pts',(35.9850862827464,-1.90691083807915,4.61429576063476));
#27268=CARTESIAN_POINT('Ctrl Pts',(36.0247226157447,-2.65646064488639,4.22744026015335));
#27269=CARTESIAN_POINT('Ctrl Pts',(36.064358948743,-3.26806603342656,3.68503995498266));
#27270=CARTESIAN_POINT('Ctrl Pts',(36.1039952817413,-3.8796714219667,3.142639649812));
#27271=CARTESIAN_POINT('Ctrl Pts',(36.1436316147397,-4.35333239223978,2.44469453995207));
#27272=CARTESIAN_POINT('Ctrl Pts',(36.183267947738,-4.63149872125605,1.67600556790799));
#27273=CARTESIAN_POINT('Ctrl Pts',(36.2108981231908,-4.82540627764142,1.14015854171839));
#27274=CARTESIAN_POINT('Ctrl Pts',(36.2385282986436,-4.92431567132321,0.569934425257451));
#27275=CARTESIAN_POINT('Ctrl Pts',(36.2661584740964,-4.92482433489693,-0.000117749303896287));
#27276=CARTESIAN_POINT('Origin',(41.25,0.,0.));
#27277=CARTESIAN_POINT('',(37.9838415259036,-4.92485067281264,0.000120817417613023));
#27278=CARTESIAN_POINT('',(37.7661584740964,-4.92480467811149,0.000114993715880741));
#27279=CARTESIAN_POINT('',(41.25,-4.925,-6.03138548580071E-16));
#27280=CARTESIAN_POINT('Ctrl Pts',(37.9838415259036,-4.92485067281264,0.000120817417613023));
#27281=CARTESIAN_POINT('Ctrl Pts',(37.9722920584757,-4.92507066765589,0.238400081367369));
#27282=CARTESIAN_POINT('Ctrl Pts',(37.9607425910477,-4.9080872440668,0.476648253950855));
#27283=CARTESIAN_POINT('Ctrl Pts',(37.9491931236198,-4.87363741638938,0.712343491708345));
#27284=CARTESIAN_POINT('Ctrl Pts',(37.9095567906214,-4.75540990069872,1.52122017698863));
#27285=CARTESIAN_POINT('Ctrl Pts',(37.8699204576231,-4.43146711813237,2.30002898645485));
#27286=CARTESIAN_POINT('Ctrl Pts',(37.8302841246248,-3.94116839977733,2.9541439650625));
#27287=CARTESIAN_POINT('Ctrl Pts',(37.7906477916264,-3.45086968142229,3.60825894367013));
#27288=CARTESIAN_POINT('Ctrl Pts',(37.7510114586281,-2.79421502727857,4.13768009141919));
#27289=CARTESIAN_POINT('Ctrl Pts',(37.7113751256298,-2.05098855374135,4.47808227597847));
#27290=CARTESIAN_POINT('Ctrl Pts',(37.6717387926315,-1.30776208020412,4.81848446053774));
#27291=CARTESIAN_POINT('Ctrl Pts',(37.6321024596332,-0.477963787273387,
4.96986768190722));
#27292=CARTESIAN_POINT('Ctrl Pts',(37.5924661266349,0.337585105473864,4.9138387454774));
#27293=CARTESIAN_POINT('Ctrl Pts',(37.5528297936365,1.15313399822113,4.85780980904757));
#27294=CARTESIAN_POINT('Ctrl Pts',(37.5131934606382,1.95443349078488,4.59436871481845));
#27295=CARTESIAN_POINT('Ctrl Pts',(37.4735571276399,2.6441249924731,4.15552378688388));
#27296=CARTESIAN_POINT('Ctrl Pts',(37.4339207946416,3.33381649416131,3.71667885894933));
#27297=CARTESIAN_POINT('Ctrl Pts',(37.3942844616432,3.91190000497398,3.10243009730932));
#27298=CARTESIAN_POINT('Ctrl Pts',(37.3546481286449,4.30813787178923,2.38740926467432));
#27299=CARTESIAN_POINT('Ctrl Pts',(37.3150117956466,4.7043757386045,1.6723884320393));
#27300=CARTESIAN_POINT('Ctrl Pts',(37.2753754626483,4.91876796142238,0.856595528409254));
#27301=CARTESIAN_POINT('Ctrl Pts',(37.23573912965,4.92526569725575,0.0391501065792324));
#27302=CARTESIAN_POINT('Ctrl Pts',(37.1961027966516,4.93176343308912,-0.778295315250795));
#27303=CARTESIAN_POINT('Ctrl Pts',(37.1564664636533,4.730366681938,-1.59739325528078));
#27304=CARTESIAN_POINT('Ctrl Pts',(37.116830130655,4.34554532557911,-2.31862259599992));
#27305=CARTESIAN_POINT('Ctrl Pts',(37.0771937976567,3.96072396922023,-3.03985193671904));
#27306=CARTESIAN_POINT('Ctrl Pts',(37.0375574646584,3.39247800765361,-3.6632126781273));
#27307=CARTESIAN_POINT('Ctrl Pts',(36.99792113166,2.70984982319539,-4.11296594383257));
#27308=CARTESIAN_POINT('Ctrl Pts',(36.9582847986617,2.02722163873717,-4.56271920953783));
#27309=CARTESIAN_POINT('Ctrl Pts',(36.9186484656634,1.23021123138735,-4.8388649995401));
#27310=CARTESIAN_POINT('Ctrl Pts',(36.8790121326651,0.415656064117347,-4.90785135835727));
#27311=CARTESIAN_POINT('Ctrl Pts',(36.8393757996667,-0.398899103152658,
-4.97683771717445));
#27312=CARTESIAN_POINT('Ctrl Pts',(36.7997394666684,-1.23099903034286,-4.83866464480654));
#27313=CARTESIAN_POINT('Ctrl Pts',(36.7601031336701,-1.97954284707522,-4.51012029063243));
#27314=CARTESIAN_POINT('Ctrl Pts',(36.7204668006718,-2.7280866638076,-4.18157593645832));
#27315=CARTESIAN_POINT('Ctrl Pts',(36.6808304676735,-3.39307437008213,-3.662660300478));
#27316=CARTESIAN_POINT('Ctrl Pts',(36.6411941346751,-3.89370937681127,-3.01642208722661));
#27317=CARTESIAN_POINT('Ctrl Pts',(36.6015578016768,-4.39434438354041,-2.37018387397521));
#27318=CARTESIAN_POINT('Ctrl Pts',(36.5619214686785,-4.73062669072415,-1.59662308345274));
#27319=CARTESIAN_POINT('Ctrl Pts',(36.5222851356802,-4.86169770333288,-0.789728029630932));
#27320=CARTESIAN_POINT('Ctrl Pts',(36.509470599088,-4.90407332590429,-0.528856616685018));
#27321=CARTESIAN_POINT('Ctrl Pts',(36.4966560624958,-4.924999302212,-0.264500950312836));
#27322=CARTESIAN_POINT('Ctrl Pts',(36.4838415259036,-4.92478004438697,-0.000110922936420454));
#27323=CARTESIAN_POINT('Ctrl Pts',(36.2661584740964,-4.92482433489693,-0.000117749303896287));
#27324=CARTESIAN_POINT('Ctrl Pts',(36.2781646316419,-4.92504536480005,-0.247822879828381));
#27325=CARTESIAN_POINT('Ctrl Pts',(36.2901707891874,-4.90668667699816,-0.49549554482184));
#27326=CARTESIAN_POINT('Ctrl Pts',(36.3021769467329,-4.86946910202077,-0.740301109765489));
#27327=CARTESIAN_POINT('Ctrl Pts',(36.3418132797313,-4.74660146600976,-1.54848598116662));
#27328=CARTESIAN_POINT('Ctrl Pts',(36.3814496127296,-4.41819450622829,-2.32542288974066));
#27329=CARTESIAN_POINT('Ctrl Pts',(36.4210859457279,-3.92414995609534,-2.97671332021275));
#27330=CARTESIAN_POINT('Ctrl Pts',(36.4607222787263,-3.43010540596239,-3.62800375068483));
#27331=CARTESIAN_POINT('Ctrl Pts',(36.5003586117246,-2.77042326547796,-4.15364770305498));
#27332=CARTESIAN_POINT('Ctrl Pts',(36.5399949447229,-2.02525549283558,-4.48977897645243));
#27333=CARTESIAN_POINT('Ctrl Pts',(36.5796312777212,-1.28008772019321,-4.82591024984988));
#27334=CARTESIAN_POINT('Ctrl Pts',(36.6192676107195,-0.449434315392872,
-4.97252884427464));
#27335=CARTESIAN_POINT('Ctrl Pts',(36.6589039437178,0.365779604923634,-4.91182047201209));
#27336=CARTESIAN_POINT('Ctrl Pts',(36.6985402767162,1.18099352524016,-4.85111209974954));
#27337=CARTESIAN_POINT('Ctrl Pts',(36.7381766097145,1.98076796107286,-4.5830767607997));
#27338=CARTESIAN_POINT('Ctrl Pts',(36.7778129427128,2.66792961757094,-4.14028098374283));
#27339=CARTESIAN_POINT('Ctrl Pts',(36.8174492757111,3.35509127406902,-3.69748520668596));
#27340=CARTESIAN_POINT('Ctrl Pts',(36.8570856087094,3.92964015123248,-3.0799289915221));
#27341=CARTESIAN_POINT('Ctrl Pts',(36.8967219417078,4.32176805696933,-2.36264595960017));
#27342=CARTESIAN_POINT('Ctrl Pts',(36.9363582747061,4.71389596270618,-1.64536292767826));
#27343=CARTESIAN_POINT('Ctrl Pts',(36.9759946077044,4.92360289701643,-0.828353078998293));
#27344=CARTESIAN_POINT('Ctrl Pts',(37.0156309407027,4.92540928360095,-0.0108838261772031));
#27345=CARTESIAN_POINT('Ctrl Pts',(37.0552672737011,4.92721567018547,0.80658542664391));
#27346=CARTESIAN_POINT('Ctrl Pts',(37.0949036066994,4.72112150904426,1.62451408360616));
#27347=CARTESIAN_POINT('Ctrl Pts',(37.1345399396977,4.33216742137014,2.34352309608281));
#27348=CARTESIAN_POINT('Ctrl Pts',(37.174176272696,3.94321333369602,3.06253210855944));
#27349=CARTESIAN_POINT('Ctrl Pts',(37.2138126056943,3.37139931948902,3.68262147655047));
#27350=CARTESIAN_POINT('Ctrl Pts',(37.2534489386926,2.68620128259561,4.12844979841592));
#27351=CARTESIAN_POINT('Ctrl Pts',(37.293085271691,2.0010032457022,4.57427812028138));
#27352=CARTESIAN_POINT('Ctrl Pts',(37.3327216046893,1.20242118612239,4.84584539602124));
#27353=CARTESIAN_POINT('Ctrl Pts',(37.3723579376876,0.387483523946268,4.91015596364463));
#27354=CARTESIAN_POINT('Ctrl Pts',(37.4119942706859,-0.427454138229844,
4.97446653126802));
#27355=CARTESIAN_POINT('Ctrl Pts',(37.4516306036843,-1.25874740300227,4.83152039077494));
#27356=CARTESIAN_POINT('Ctrl Pts',(37.4912669366826,-2.0053934101798,4.49868562349977));
#27357=CARTESIAN_POINT('Ctrl Pts',(37.5309032696809,-2.75203941735733,4.1658508562246));
#27358=CARTESIAN_POINT('Ctrl Pts',(37.5705396026792,-3.41403816693998,3.64312746216736));
#27359=CARTESIAN_POINT('Ctrl Pts',(37.6101759356775,-3.9109562307027,2.99402679182231));
#27360=CARTESIAN_POINT('Ctrl Pts',(37.6498122686759,-4.40787429446542,2.34492612147726));
#27361=CARTESIAN_POINT('Ctrl Pts',(37.6894486016742,-4.73971167240821,1.56944817484441));
#27362=CARTESIAN_POINT('Ctrl Pts',(37.7290849346725,-4.86614983229095,0.761814202008249));
#27363=CARTESIAN_POINT('Ctrl Pts',(37.7414427811471,-4.90557081930387,0.510009459010666));
#27364=CARTESIAN_POINT('Ctrl Pts',(37.7538006276218,-4.92502551330707,0.255078917155293));
#27365=CARTESIAN_POINT('Ctrl Pts',(37.7661584740964,-4.92480467811149,0.000114993715880741));
#27366=CARTESIAN_POINT('Origin',(41.25,0.,0.));
#27367=CARTESIAN_POINT('',(39.4838415259036,-4.92532729210881,-7.01284572532379E-5));
#27368=CARTESIAN_POINT('',(39.2661584740964,-4.92535986435928,-6.05616521270463E-5));
#27369=CARTESIAN_POINT('',(41.25,-4.925,-6.03138548580071E-16));
#27370=CARTESIAN_POINT('Ctrl Pts',(39.4838415259036,-4.92532729210881,-7.01284572532379E-5));
#27371=CARTESIAN_POINT('Ctrl Pts',(39.4479280544555,-4.92478402189283,0.740663422453838));
#27372=CARTESIAN_POINT('Ctrl Pts',(39.4120145830074,-4.75533077391977,1.48162891276357));
#27373=CARTESIAN_POINT('Ctrl Pts',(39.3761011115593,-4.43228737044207,2.14815909981045));
#27374=CARTESIAN_POINT('Ctrl Pts',(39.3364647785609,-4.07575664821281,2.88378312561361));
#27375=CARTESIAN_POINT('Ctrl Pts',(39.2968284455626,-3.53214240127592,3.52873975902211));
#27376=CARTESIAN_POINT('Ctrl Pts',(39.2571921125643,-2.86749071492952,4.00465759431309));
#27377=CARTESIAN_POINT('Ctrl Pts',(39.217555779566,-2.20283902858313,4.48057542960406));
#27378=CARTESIAN_POINT('Ctrl Pts',(39.1779194465677,-1.41714990282724,4.7874544667775));
#27379=CARTESIAN_POINT('Ctrl Pts',(39.1382831135693,-0.605887020789073,
4.8880129502341));
#27380=CARTESIAN_POINT('Ctrl Pts',(39.098646780571,0.205375861249093,4.98857143369071));
#27381=CARTESIAN_POINT('Ctrl Pts',(39.0590104475727,1.04221249956953,4.88280936343047));
#27382=CARTESIAN_POINT('Ctrl Pts',(39.0193741145744,1.80294739451225,4.5835747596906));
#27383=CARTESIAN_POINT('Ctrl Pts',(38.9797377815761,2.56368228945497,4.28434015595073));
#27384=CARTESIAN_POINT('Ctrl Pts',(38.9401014485778,3.24831544101998,3.79163301873121));
#27385=CARTESIAN_POINT('Ctrl Pts',(38.9004651155794,3.77366287747338,3.16531878190195));
#27386=CARTESIAN_POINT('Ctrl Pts',(38.8608287825811,4.29901031392678,2.53900454507269));
#27387=CARTESIAN_POINT('Ctrl Pts',(38.8211924495828,4.66507203526857,1.77908320863369));
#27388=CARTESIAN_POINT('Ctrl Pts',(38.7815561165845,4.82737144406183,0.97788533702132));
#27389=CARTESIAN_POINT('Ctrl Pts',(38.7419197835861,4.98967085285509,0.176687465408939));
#27390=CARTESIAN_POINT('Ctrl Pts',(38.7022834505878,4.94820794909981,-0.665786941376808));
#27391=CARTESIAN_POINT('Ctrl Pts',(38.6626471175895,4.70802040038411,-1.44717623190548));
#27392=CARTESIAN_POINT('Ctrl Pts',(38.6230107845912,4.46783285166841,-2.22856552243415));
#27393=CARTESIAN_POINT('Ctrl Pts',(38.5833744515928,4.02892065799228,-2.94886969670574));
#27394=CARTESIAN_POINT('Ctrl Pts',(38.5437381185945,3.44461209146379,-3.52057130300519));
#27395=CARTESIAN_POINT('Ctrl Pts',(38.5041017855962,2.86030352493532,-4.09227290930463));
#27396=CARTESIAN_POINT('Ctrl Pts',(38.4644654525979,2.13059858555448,-4.51537194763194));
#27397=CARTESIAN_POINT('Ctrl Pts',(38.4248291195996,1.34415703490748,-4.73846144550029));
#27398=CARTESIAN_POINT('Ctrl Pts',(38.3851927866013,0.557715484260454,-4.96155094336865));
#27399=CARTESIAN_POINT('Ctrl Pts',(38.3455564536029,-0.285462677652743,
-4.98463090077803));
#27400=CARTESIAN_POINT('Ctrl Pts',(38.3059201206046,-1.0829305511676,-4.80489711703856));
#27401=CARTESIAN_POINT('Ctrl Pts',(38.2662837876063,-1.88039842468243,-4.6251633332991));
#27402=CARTESIAN_POINT('Ctrl Pts',(38.226647454608,-2.63215600979892,-4.2426158084108));
#27403=CARTESIAN_POINT('Ctrl Pts',(38.1870111216097,-3.24686410815625,-3.70373438467301));
#27404=CARTESIAN_POINT('Ctrl Pts',(38.1473747886113,-3.8615722065136,-3.16485296093521));
#27405=CARTESIAN_POINT('Ctrl Pts',(38.107738455613,-4.33923081811179,-2.46963763834791));
#27406=CARTESIAN_POINT('Ctrl Pts',(38.0681021226147,-4.62180399950339,-1.70255769650709));
#27407=CARTESIAN_POINT('Ctrl Pts',(38.0400152570443,-4.82203934821423,-1.15899401191694));
#27408=CARTESIAN_POINT('Ctrl Pts',(38.011928391474,-4.92431567276809,-0.579344659801372));
#27409=CARTESIAN_POINT('Ctrl Pts',(37.9838415259036,-4.92485067281264,0.000120817417613023));
#27410=CARTESIAN_POINT('Ctrl Pts',(37.7661584740964,-4.92480467811149,0.000114993715880741));
#27411=CARTESIAN_POINT('Ctrl Pts',(37.7934369606201,-4.92431721049982,-0.5626877538214));
#27412=CARTESIAN_POINT('Ctrl Pts',(37.8207154471438,-4.82796004188169,-1.12565315428906));
#27413=CARTESIAN_POINT('Ctrl Pts',(37.8479939336675,-4.63886049554297,-1.65552057418984));
#27414=CARTESIAN_POINT('Ctrl Pts',(37.8876302666658,-4.36409405708955,-2.4254313785122));
#27415=CARTESIAN_POINT('Ctrl Pts',(37.9272665996641,-3.89352223836002,-3.12546298811743));
#27416=CARTESIAN_POINT('Ctrl Pts',(37.9669029326624,-3.28431992769162,-3.6705609490957));
#27417=CARTESIAN_POINT('Ctrl Pts',(38.0065392656607,-2.67511761702323,-4.21565891007397));
#27418=CARTESIAN_POINT('Ctrl Pts',(38.0461755986591,-1.92728481441597,-4.6058232224253));
#27419=CARTESIAN_POINT('Ctrl Pts',(38.0858119316574,-1.13168386082912,-4.79364857998611));
#27420=CARTESIAN_POINT('Ctrl Pts',(38.1254482646557,-0.336082907242237,
-4.98147393754693));
#27421=CARTESIAN_POINT('Ctrl Pts',(38.165084597654,0.507286197324216,-4.96696034031723));
#27422=CARTESIAN_POINT('Ctrl Pts',(38.2047209306523,1.29595336769371,-4.75187120364867));
#27423=CARTESIAN_POINT('Ctrl Pts',(38.2443572636507,2.08462053806321,-4.53678206698012));
#27424=CARTESIAN_POINT('Ctrl Pts',(38.283993596649,2.81858577423572,-4.1211173908727));
#27425=CARTESIAN_POINT('Ctrl Pts',(38.3236299296473,3.40867165653206,-3.55538079661358));
#27426=CARTESIAN_POINT('Ctrl Pts',(38.3632662626456,3.99875753882839,-2.98964420235446));
#27427=CARTESIAN_POINT('Ctrl Pts',(38.402902595644,4.44496406724855,-2.27383568994364));
#27428=CARTESIAN_POINT('Ctrl Pts',(38.4425389286423,4.69307675806728,-1.49492662321651));
#27429=CARTESIAN_POINT('Ctrl Pts',(38.4821752616406,4.94118944888601,-0.716017556489387));
#27430=CARTESIAN_POINT('Ctrl Pts',(38.5218115946389,4.9912083021033,0.125992064554042));
#27431=CARTESIAN_POINT('Ctrl Pts',(38.5614479276372,4.83705598218242,0.928797337566571));
#27432=CARTESIAN_POINT('Ctrl Pts',(38.6010842606355,4.68290366226154,1.73160261057911));
#27433=CARTESIAN_POINT('Ctrl Pts',(38.6407205936339,4.32458016920247,2.49520353556076));
#27434=CARTESIAN_POINT('Ctrl Pts',(38.6803569266322,3.80562212350232,3.12682192191077));
#27435=CARTESIAN_POINT('Ctrl Pts',(38.7199932596305,3.28666407780217,3.75844030826078));
#27436=CARTESIAN_POINT('Ctrl Pts',(38.7596295926288,2.60707147946093,4.25807615597916));
#27437=CARTESIAN_POINT('Ctrl Pts',(38.7992659256271,1.8494154206263,4.56502328970031));
#27438=CARTESIAN_POINT('Ctrl Pts',(38.8389022586255,1.09175936179166,4.87197042342147));
#27439=CARTESIAN_POINT('Ctrl Pts',(38.8785385916238,0.256039842463638,4.9862288431454));
#27440=CARTESIAN_POINT('Ctrl Pts',(38.9181749246221,-0.556202475131627,
4.8939160148322));
#27441=CARTESIAN_POINT('Ctrl Pts',(38.9578112576204,-1.36844479272689,4.80160318651899));
#27442=CARTESIAN_POINT('Ctrl Pts',(38.9974475906187,-2.15720990858938,4.50271911016864));
#27443=CARTESIAN_POINT('Ctrl Pts',(39.0370839236171,-2.82666218631365,4.03357853464529));
#27444=CARTESIAN_POINT('Ctrl Pts',(39.0767202566154,-3.49611446403792,3.56443795912194));
#27445=CARTESIAN_POINT('Ctrl Pts',(39.1163565896137,-4.04625390362397,2.92504088442559));
#27446=CARTESIAN_POINT('Ctrl Pts',(39.1559929226121,-4.41023804827196,2.19307447250255));
#27447=CARTESIAN_POINT('Ctrl Pts',(39.1927147731068,-4.74745822812066,1.51492997444862));
#27448=CARTESIAN_POINT('Ctrl Pts',(39.2294366236016,-4.92489283176939,0.757328994148836));
#27449=CARTESIAN_POINT('Ctrl Pts',(39.2661584740964,-4.92535986435928,-6.05616521270463E-5));
#27450=CARTESIAN_POINT('Origin',(41.25,0.,0.));
#27451=CARTESIAN_POINT('',(40.9838415259036,-4.92312335471689,0.00654147285873569));
#27452=CARTESIAN_POINT('',(40.7661584740964,-4.92470501206087,0.000456272822055327));
#27453=CARTESIAN_POINT('',(41.25,-4.925,-6.03138548580071E-16));
#27454=CARTESIAN_POINT('Ctrl Pts',(40.9838415259036,-4.92312335471689,0.00654147285873569));
#27455=CARTESIAN_POINT('Ctrl Pts',(40.9632003834336,-4.92719130640019,0.433011391936502));
#27456=CARTESIAN_POINT('Ctrl Pts',(40.9425592409637,-4.87680194143325,0.858319305362528));
#27457=CARTESIAN_POINT('Ctrl Pts',(40.9219180984937,-4.76835699241177,1.26767821358287));
#27458=CARTESIAN_POINT('Ctrl Pts',(40.8426454324971,-4.35187228303479,2.83982820728391));
#27459=CARTESIAN_POINT('Ctrl Pts',(40.7633727665005,-3.07909246396308,4.17673717491474));
#27460=CARTESIAN_POINT('Ctrl Pts',(40.6841001005039,-1.5283810325561,4.68726372815487));
#27461=CARTESIAN_POINT('Ctrl Pts',(40.6444637675055,-0.753025316852604,
4.94252700477493));
#27462=CARTESIAN_POINT('Ctrl Pts',(40.6048274345072,0.0918133019347075,
4.9911946777973));
#27463=CARTESIAN_POINT('Ctrl Pts',(40.5651911015089,0.89643139271475,4.84097909079969));
#27464=CARTESIAN_POINT('Ctrl Pts',(40.5255547685106,1.70104948349479,4.69076350380207));
#27465=CARTESIAN_POINT('Ctrl Pts',(40.4859184355122,2.46544704626757,4.34166465678447));
#27466=CARTESIAN_POINT('Ctrl Pts',(40.4462821025139,3.10020438041818,3.82803285295568));
#27467=CARTESIAN_POINT('Ctrl Pts',(40.4066457695156,3.73496171456878,3.3144010491269));
#27468=CARTESIAN_POINT('Ctrl Pts',(40.3670094365173,4.24007882009722,2.63623628848694));
#27469=CARTESIAN_POINT('Ctrl Pts',(40.327373103519,4.55242656245004,1.88020324123194));
#27470=CARTESIAN_POINT('Ctrl Pts',(40.2877367705206,4.86477430480286,1.12417019397695));
#27471=CARTESIAN_POINT('Ctrl Pts',(40.2481004375223,4.98435268398005,0.290268860106923));
#27472=CARTESIAN_POINT('Ctrl Pts',(40.208464104524,4.8975150328889,-0.522335340103032));
#27473=CARTESIAN_POINT('Ctrl Pts',(40.1688277715257,4.81067738179775,-1.33493954031299));
#27474=CARTESIAN_POINT('Ctrl Pts',(40.1291914385274,4.51742370043825,-2.12624660686287));
#27475=CARTESIAN_POINT('Ctrl Pts',(40.089555105529,4.05294216033234,-2.7990307722324));
#27476=CARTESIAN_POINT('Ctrl Pts',(40.0499187725307,3.58846062022643,-3.47181493760193));
#27477=CARTESIAN_POINT('Ctrl Pts',(40.0102824395324,2.9527512213741,-4.0260762017911));
#27478=CARTESIAN_POINT('Ctrl Pts',(39.9706461065341,2.22327502076688,-4.39501351572401));
#27479=CARTESIAN_POINT('Ctrl Pts',(39.9310097735357,1.49379882015967,-4.76395082965692));
#27480=CARTESIAN_POINT('Ctrl Pts',(39.8913734405374,0.670555817797568,-4.94756419333357));
#27481=CARTESIAN_POINT('Ctrl Pts',(39.8517371075391,-0.146540443155989,
-4.92327259531741));
#27482=CARTESIAN_POINT('Ctrl Pts',(39.8121007745408,-0.963636704109558,
-4.89898099730126));
#27483=CARTESIAN_POINT('Ctrl Pts',(39.7724644415425,-1.77458622365459,-4.6667844375923));
#27484=CARTESIAN_POINT('Ctrl Pts',(39.7328281085442,-2.48080217325227,-4.25503128141026));
#27485=CARTESIAN_POINT('Ctrl Pts',(39.6931917755458,-3.18701812284995,-3.84327812522822));
#27486=CARTESIAN_POINT('Ctrl Pts',(39.6535554425475,-3.78850050250029,-3.2519683725731));
#27487=CARTESIAN_POINT('Ctrl Pts',(39.6139191095492,-4.21219662658612,-2.55287835332392));
#27488=CARTESIAN_POINT('Ctrl Pts',(39.5742827765509,-4.63589275067194,-1.85378833407475));
#27489=CARTESIAN_POINT('Ctrl Pts',(39.5346464435525,-4.88180261919324,-1.04691804823153));
#27490=CARTESIAN_POINT('Ctrl Pts',(39.4950101105542,-4.92003395469309,-0.230337196211024));
#27491=CARTESIAN_POINT('Ctrl Pts',(39.491287249004,-4.92362485118071,-0.15363944879941));
#27492=CARTESIAN_POINT('Ctrl Pts',(39.4875643874538,-4.92538360857494,-0.0768560348162278));
#27493=CARTESIAN_POINT('Ctrl Pts',(39.4838415259036,-4.92532729210881,-7.01284572532379E-5));
#27494=CARTESIAN_POINT('Ctrl Pts',(39.2661584740964,-4.92535986435928,-6.05616521270463E-5));
#27495=CARTESIAN_POINT('Ctrl Pts',(39.2690729565999,-4.92539693107279,-0.0601718735549025));
#27496=CARTESIAN_POINT('Ctrl Pts',(39.2719874391034,-4.92431927345987,-0.120281853688074));
#27497=CARTESIAN_POINT('Ctrl Pts',(39.274901921607,-4.9221183016965,-0.180350673538913));
#27498=CARTESIAN_POINT('Ctrl Pts',(39.3145382546053,-4.89218556076315,-0.997273658507651));
#27499=CARTESIAN_POINT('Ctrl Pts',(39.3541745876036,-4.65449122918653,-1.80658387929538));
#27500=CARTESIAN_POINT('Ctrl Pts',(39.393810920602,-4.23791524610868,-2.50995000407357));
#27501=CARTESIAN_POINT('Ctrl Pts',(39.4334472536003,-3.82133926303084,-3.21331612885174));
#27502=CARTESIAN_POINT('Ctrl Pts',(39.4730835865986,-3.22588162845177,-3.81073815762037));
#27503=CARTESIAN_POINT('Ctrl Pts',(39.5127199195969,-2.52389122711134,-4.22962765446655));
#27504=CARTESIAN_POINT('Ctrl Pts',(39.5523562525952,-1.8219008257709,-4.64851715131273));
#27505=CARTESIAN_POINT('Ctrl Pts',(39.5919925855935,-1.01337765766909,-4.88887411623647));
#27506=CARTESIAN_POINT('Ctrl Pts',(39.6316289185919,-0.1965574769085,-4.92149723378835));
#27507=CARTESIAN_POINT('Ctrl Pts',(39.6712652515902,0.620262703852086,-4.95412035134023));
#27508=CARTESIAN_POINT('Ctrl Pts',(39.7109015845885,1.44537989727145,-4.77900962152026));
#27509=CARTESIAN_POINT('Ctrl Pts',(39.7505379175869,2.17854060488518,-4.41743662914066));
#27510=CARTESIAN_POINT('Ctrl Pts',(39.7901742505852,2.91170131249894,-4.05586363676105));
#27511=CARTESIAN_POINT('Ctrl Pts',(39.8298105835835,3.55290553430707,-3.50782838182181));
#27512=CARTESIAN_POINT('Ctrl Pts',(39.8694469165818,4.02424846332451,-2.83992665169721));
#27513=CARTESIAN_POINT('Ctrl Pts',(39.9090832495801,4.49559139234193,-2.17202492157262));
#27514=CARTESIAN_POINT('Ctrl Pts',(39.9487195825785,4.79707302856867,-1.38425671626268));
#27515=CARTESIAN_POINT('Ctrl Pts',(39.9883559155768,4.89205896281718,-0.572318557806623));
#27516=CARTESIAN_POINT('Ctrl Pts',(40.0279922485751,4.98704489706568,0.23961960064943));
#27517=CARTESIAN_POINT('Ctrl Pts',(40.0676285815734,4.87553512933595,1.07572771225159));
#27518=CARTESIAN_POINT('Ctrl Pts',(40.1072649145717,4.57108642730011,1.83438198185512));
#27519=CARTESIAN_POINT('Ctrl Pts',(40.14690124757,4.26663772526427,2.59303625145865));
#27520=CARTESIAN_POINT('Ctrl Pts',(40.1865375805684,3.76925008892232,3.27423667906355));
#27521=CARTESIAN_POINT('Ctrl Pts',(40.2261739135667,3.13934012392578,3.79528850237715));
#27522=CARTESIAN_POINT('Ctrl Pts',(40.265810246565,2.50943015892925,4.31634032569076));
#27523=CARTESIAN_POINT('Ctrl Pts',(40.3054465795633,1.74699786527812,4.67724354471308));
#27524=CARTESIAN_POINT('Ctrl Pts',(40.3450829125616,0.944712214563968,4.83400506215193));
#27525=CARTESIAN_POINT('Ctrl Pts',(40.3847192455599,0.142426563849815,4.99076657959077));
#27526=CARTESIAN_POINT('Ctrl Pts',(40.4243555785583,-0.699712443927367,
4.94338639544614));
#27527=CARTESIAN_POINT('Ctrl Pts',(40.4639919115566,-1.47944958844674,4.69790665725705));
#27528=CARTESIAN_POINT('Ctrl Pts',(40.5036282445549,-2.25918673296613,4.45242691906795));
#27529=CARTESIAN_POINT('Ctrl Pts',(40.5432645775532,-2.9765220142277,4.00884762683438));
#27530=CARTESIAN_POINT('Ctrl Pts',(40.5829009105516,-3.54416805574804,3.42049456712443));
#27531=CARTESIAN_POINT('Ctrl Pts',(40.6225372435499,-4.11181409726837,2.8321415074145));
#27532=CARTESIAN_POINT('Ctrl Pts',(40.6621735765482,-4.52977089904747,2.0990146802282));
#27533=CARTESIAN_POINT('Ctrl Pts',(40.7018099095466,-4.74751677154496,1.31132578004485));
#27534=CARTESIAN_POINT('Ctrl Pts',(40.7232594310632,-4.86535170792741,0.885061574079994));
#27535=CARTESIAN_POINT('Ctrl Pts',(40.7447089525798,-4.92455446162076,0.442818752745147));
#27536=CARTESIAN_POINT('Ctrl Pts',(40.7661584740964,-4.92470501206087,0.000456272822055327));
#27537=CARTESIAN_POINT('Origin',(41.25,0.,0.));
#27538=CARTESIAN_POINT('',(42.4838415259036,-4.92524003303928,0.000110626574143721));
#27539=CARTESIAN_POINT('',(42.2661584740964,-4.92524231653586,-0.000581745865239311));
#27540=CARTESIAN_POINT('',(41.25,-4.925,-6.03138548580071E-16));
#27541=CARTESIAN_POINT('Ctrl Pts',(42.4838415259036,-4.92524003303928,0.000110626574143721));
#27542=CARTESIAN_POINT('Ctrl Pts',(42.4784727124118,-4.92534069746969,0.110850170218861));
#27543=CARTESIAN_POINT('Ctrl Pts',(42.4731038989201,-4.92168159671247,0.221582690680517));
#27544=CARTESIAN_POINT('Ctrl Pts',(42.4677350854283,-4.91421672981629,0.332057585799473));
#27545=CARTESIAN_POINT('Ctrl Pts',(42.42809875243,-4.85910586583519,1.14766046297098));
#27546=CARTESIAN_POINT('Ctrl Pts',(42.3884624194316,-4.59656460406497,1.94922166617571));
#27547=CARTESIAN_POINT('Ctrl Pts',(42.3488260864333,-4.158498505033,2.63942433349232));
#27548=CARTESIAN_POINT('Ctrl Pts',(42.309189753435,-3.72043240600104,3.32962700080891));
#27549=CARTESIAN_POINT('Ctrl Pts',(42.2695534204367,-3.10684146970732,3.90847113223737));
#27550=CARTESIAN_POINT('Ctrl Pts',(42.2299170874384,-2.39226443364707,4.30547999981316));
#27551=CARTESIAN_POINT('Ctrl Pts',(42.19028075444,-1.67768739758682,4.70248886738895));
#27552=CARTESIAN_POINT('Ctrl Pts',(42.1506444214417,-0.862124261760032,
4.91766247111206));
#27553=CARTESIAN_POINT('Ctrl Pts',(42.1110080884434,-0.044692789168467,
4.92514955874023));
#27554=CARTESIAN_POINT('Ctrl Pts',(42.0713717554451,0.77273868342311,4.93263664636839));
#27555=CARTESIAN_POINT('Ctrl Pts',(42.0317354224467,1.59203849277947,4.7324372179016));
#27556=CARTESIAN_POINT('Ctrl Pts',(41.9920990894484,2.31371310296222,4.34829220454241));
#27557=CARTESIAN_POINT('Ctrl Pts',(41.9524627564501,3.03538771314496,3.96414719118321));
#27558=CARTESIAN_POINT('Ctrl Pts',(41.9128264234518,3.6594371241541,3.39605659293162));
#27559=CARTESIAN_POINT('Ctrl Pts',(41.8731900904534,4.10993491693973,2.71420756085693));
#27560=CARTESIAN_POINT('Ctrl Pts',(41.8335537574551,4.56043270972535,2.03235852878226));
#27561=CARTESIAN_POINT('Ctrl Pts',(41.7939174244568,4.83737888428748,1.2367510628845));
#27562=CARTESIAN_POINT('Ctrl Pts',(41.7542810914585,4.90733051716129,0.421733363841795));
#27563=CARTESIAN_POINT('Ctrl Pts',(41.7146447584602,4.9772821500351,-0.393284335200907));
#27564=CARTESIAN_POINT('Ctrl Pts',(41.6750084254618,4.8402392412206,-1.22771226738855));
#27565=CARTESIAN_POINT('Ctrl Pts',(41.6353720924635,4.51245254963717,-1.97556946497589));
#27566=CARTESIAN_POINT('Ctrl Pts',(41.5957357594652,4.18466585805374,-2.72342666256322));
#27567=CARTESIAN_POINT('Ctrl Pts',(41.5560994264669,3.66613538370139,-3.38471312555024));
#27568=CARTESIAN_POINT('Ctrl Pts',(41.5164630934686,3.02049996896988,-3.88783329591911));
#27569=CARTESIAN_POINT('Ctrl Pts',(41.4768267604703,2.37486455423836,-4.39095346628799));
#27570=CARTESIAN_POINT('Ctrl Pts',(41.4371904274719,1.60212419912768,-4.73590734403872));
#27571=CARTESIAN_POINT('Ctrl Pts',(41.3975540944736,0.796173003049936,-4.86543917721391));
#27572=CARTESIAN_POINT('Ctrl Pts',(41.318281428477,-0.815729389105595,-5.12450284356429));
#27573=CARTESIAN_POINT('Ctrl Pts',(41.2390087624804,-2.56047514512941,-4.52187833161248));
#27574=CARTESIAN_POINT('Ctrl Pts',(41.1597360964837,-3.6527532233002,-3.31687056575093));
#27575=CARTESIAN_POINT('Ctrl Pts',(41.101104572957,-4.46062220351945,-2.42562463267031));
#27576=CARTESIAN_POINT('Ctrl Pts',(41.0424730494303,-4.91156826733875,-1.20485373601841));
#27577=CARTESIAN_POINT('Ctrl Pts',(40.9838415259036,-4.92312335471689,0.00654147285873569));
#27578=CARTESIAN_POINT('Ctrl Pts',(40.7661584740964,-4.92470501206087,0.000456272822055327));
#27579=CARTESIAN_POINT('Ctrl Pts',(40.7843452855781,-4.92483266210987,-0.374617969403003));
#27580=CARTESIAN_POINT('Ctrl Pts',(40.8025320970598,-4.88250676151333,-0.749778236054864));
#27581=CARTESIAN_POINT('Ctrl Pts',(40.8207189085415,-4.79747128229509,-1.11535753233566));
#27582=CARTESIAN_POINT('Ctrl Pts',(40.8603552415398,-4.61214497733185,-1.91210097135244));
#27583=CARTESIAN_POINT('Ctrl Pts',(40.8999915745381,-4.22395742418951,-2.66333687620561));
#27584=CARTESIAN_POINT('Ctrl Pts',(40.9396279075364,-3.68111313624165,-3.2733004318091));
#27585=CARTESIAN_POINT('Ctrl Pts',(40.9792642405348,-3.13826884829379,-3.88326398741259));
#27586=CARTESIAN_POINT('Ctrl Pts',(41.0189005735331,-2.44076782554041,-4.35195519376641));
#27587=CARTESIAN_POINT('Ctrl Pts',(41.0585369065314,-1.67125931107344,-4.63093894008567));
#27588=CARTESIAN_POINT('Ctrl Pts',(41.0981732395297,-0.901750796606443,
-4.90992268640494));
#27589=CARTESIAN_POINT('Ctrl Pts',(41.1378095725281,-0.0602347904258443,
-4.99919897268965));
#27590=CARTESIAN_POINT('Ctrl Pts',(41.1774459055264,0.746297725178827,-4.87333646147363));
#27591=CARTESIAN_POINT('Ctrl Pts',(41.256718571523,2.35936275638813,-4.62161143904159));
#27592=CARTESIAN_POINT('Ctrl Pts',(41.3359912375197,3.83249382529375,-3.50933122660671));
#27593=CARTESIAN_POINT('Ctrl Pts',(41.4152639035163,4.49894422300268,-2.02576932080728));
#27594=CARTESIAN_POINT('Ctrl Pts',(41.4945365695129,5.16539462071163,-0.542207415007845));
#27595=CARTESIAN_POINT('Ctrl Pts',(41.5738092355096,5.0251643472239,1.31263618415612));
#27596=CARTESIAN_POINT('Ctrl Pts',(41.6530819015062,4.14324285485124,2.6791377546773));
#27597=CARTESIAN_POINT('Ctrl Pts',(41.7323545675028,3.26132136247858,4.0456393251985));
#27598=CARTESIAN_POINT('Ctrl Pts',(41.8116272334995,1.63770865122098,4.92379886707688));
#27599=CARTESIAN_POINT('Ctrl Pts',(41.8908998994961,0.00513277477895049,
4.9301462671972));
#27600=CARTESIAN_POINT('Ctrl Pts',(41.9305362324945,-0.811155163442051,
4.93331996725735));
#27601=CARTESIAN_POINT('Ctrl Pts',(41.9701725654928,-1.62968389295916,4.718540631878));
#27602=CARTESIAN_POINT('Ctrl Pts',(42.0098088984911,-2.34850201279282,4.32703610425884));
#27603=CARTESIAN_POINT('Ctrl Pts',(42.0494452314894,-3.06732013262647,3.93553157663968));
#27604=CARTESIAN_POINT('Ctrl Pts',(42.0890815644878,-3.68642764277668,3.36730185678069));
#27605=CARTESIAN_POINT('Ctrl Pts',(42.1287178974861,-4.13139670740965,2.68265742962034));
#27606=CARTESIAN_POINT('Ctrl Pts',(42.1683542304844,-4.57636577204261,1.99801300245999));
#27607=CARTESIAN_POINT('Ctrl Pts',(42.2079905634827,-4.84719639115833,1.19695386799826));
#27608=CARTESIAN_POINT('Ctrl Pts',(42.247626896481,-4.91062973406511,0.381403650086907));
#27609=CARTESIAN_POINT('Ctrl Pts',(42.2538040890195,-4.92051561257233,0.254302822645805));
#27610=CARTESIAN_POINT('Ctrl Pts',(42.2599812815579,-4.92536418444955,0.126850032864256));
#27611=CARTESIAN_POINT('Ctrl Pts',(42.2661584740964,-4.92524231653586,-0.000581745865239312));
#27612=CARTESIAN_POINT('Origin',(41.25,0.,0.));
#27613=CARTESIAN_POINT('',(43.9838415259036,-4.92495182736585,-0.000126817358605258));
#27614=CARTESIAN_POINT('',(43.7661584740964,-4.92500388850328,-0.000126728605493087));
#27615=CARTESIAN_POINT('',(41.25,-4.925,-6.03138548580071E-16));
#27616=CARTESIAN_POINT('Ctrl Pts',(43.9838415259036,-4.92495182736585,-0.000126817358605258));
#27617=CARTESIAN_POINT('Ctrl Pts',(43.9541087083917,-4.92433624971945,0.613260411095392));
#27618=CARTESIAN_POINT('Ctrl Pts',(43.9243758908798,-4.80942794181503,1.22687181317958));
#27619=CARTESIAN_POINT('Ctrl Pts',(43.8946430733678,-4.58560281726217,1.79778244828448));
#27620=CARTESIAN_POINT('Ctrl Pts',(43.8550067403695,-4.2872252024731,2.558854083565));
#27621=CARTESIAN_POINT('Ctrl Pts',(43.8153704073711,-3.79529020284407,3.24404167227217));
#27622=CARTESIAN_POINT('Ctrl Pts',(43.7757340743728,-3.16956835360222,3.77009434044043));
#27623=CARTESIAN_POINT('Ctrl Pts',(43.7360977413745,-2.54384650436036,4.29614700860869));
#27624=CARTESIAN_POINT('Ctrl Pts',(43.6964614083762,-1.78433780550569,4.66306475623804));
#27625=CARTESIAN_POINT('Ctrl Pts',(43.6568250753779,-0.983323226255741,
4.82626671845745));
#27626=CARTESIAN_POINT('Ctrl Pts',(43.6171887423796,-0.182308647005795,
4.98946868067685));
#27627=CARTESIAN_POINT('Ctrl Pts',(43.5775524093812,0.660211812639427,4.94895485748631));
#27628=CARTESIAN_POINT('Ctrl Pts',(43.5379160763829,1.44187117188668,4.70964778766782));
#27629=CARTESIAN_POINT('Ctrl Pts',(43.4982797433846,2.22353053113393,4.47034071784932));
#27630=CARTESIAN_POINT('Ctrl Pts',(43.4586434103863,2.94432878998322,4.03224040140287));
#27631=CARTESIAN_POINT('Ctrl Pts',(43.4190070773879,3.5166883414399,3.44857626359137));
#27632=CARTESIAN_POINT('Ctrl Pts',(43.3793707443896,4.08904789289657,2.86491212577987));
#27633=CARTESIAN_POINT('Ctrl Pts',(43.3397344113913,4.51296873696065,2.13568416660331));
#27634=CARTESIAN_POINT('Ctrl Pts',(43.300098078393,4.73694409335704,1.34949451562975));
#27635=CARTESIAN_POINT('Ctrl Pts',(43.2604617453947,4.96091944975344,0.563304864656144));
#27636=CARTESIAN_POINT('Ctrl Pts',(43.2208254123963,4.98494931848214,-0.279846478114447));
#27637=CARTESIAN_POINT('Ctrl Pts',(43.181189079398,4.8061141017137,-1.07751647096024));
#27638=CARTESIAN_POINT('Ctrl Pts',(43.1415527463997,4.62727888494526,-1.87518646380601));
#27639=CARTESIAN_POINT('Ctrl Pts',(43.1019164134014,4.24557858267969,-2.62737510672696));
#27640=CARTESIAN_POINT('Ctrl Pts',(43.0622800804031,3.7073900118728,-3.2426896528834));
#27641=CARTESIAN_POINT('Ctrl Pts',(43.0226437474048,3.16920144106591,-3.85800419903984));
#27642=CARTESIAN_POINT('Ctrl Pts',(42.9830074144064,2.4745246017177,-4.33644464843178));
#27643=CARTESIAN_POINT('Ctrl Pts',(42.9433710814081,1.70776354660135,-4.61988239596167));
#27644=CARTESIAN_POINT('Ctrl Pts',(42.9037347484098,0.941002491484994,-4.90332014349156));
#27645=CARTESIAN_POINT('Ctrl Pts',(42.8640984154114,0.102157220600491,-4.9917551891594));
#27646=CARTESIAN_POINT('Ctrl Pts',(42.8244620824131,-0.706852245384476,
-4.87443795232758));
#27647=CARTESIAN_POINT('Ctrl Pts',(42.7848257494148,-1.51586171136944,-4.75712071549575));
#27648=CARTESIAN_POINT('Ctrl Pts',(42.7451894164165,-2.29503537245488,-4.43405119616424));
#27649=CARTESIAN_POINT('Ctrl Pts',(42.7055530834182,-2.94970211843778,-3.94449188930112));
#27650=CARTESIAN_POINT('Ctrl Pts',(42.6659167504199,-3.60436886442068,-3.454932582438));
#27651=CARTESIAN_POINT('Ctrl Pts',(42.6262804174215,-4.13452869530104,-2.79888348804327));
#27652=CARTESIAN_POINT('Ctrl Pts',(42.5866440844232,-4.47576837764522,-2.05603666527677));
#27653=CARTESIAN_POINT('Ctrl Pts',(42.5523765649167,-4.77078652353756,-1.41380979755406));
#27654=CARTESIAN_POINT('Ctrl Pts',(42.5181090454101,-4.92459752229869,-0.706706527309889));
#27655=CARTESIAN_POINT('Ctrl Pts',(42.4838415259036,-4.92524003303928,0.000110626574143721));
#27656=CARTESIAN_POINT('Ctrl Pts',(42.2661584740964,-4.92524231653586,-0.000581745865239312));
#27657=CARTESIAN_POINT('Ctrl Pts',(42.2996176145563,-4.92458221154214,-0.690823754191429));
#27658=CARTESIAN_POINT('Ctrl Pts',(42.3330767550162,-4.77809370979876,-1.38044931645573));
#27659=CARTESIAN_POINT('Ctrl Pts',(42.366535895476,-4.49640310266108,-2.01018654256035));
#27660=CARTESIAN_POINT('Ctrl Pts',(42.4061722284743,-4.16270706165249,-2.75618521593511));
#27661=CARTESIAN_POINT('Ctrl Pts',(42.4458085614727,-3.63927891293753,-3.41814126132365));
#27662=CARTESIAN_POINT('Ctrl Pts',(42.485444894471,-2.9896289807233,-3.91446405638524));
#27663=CARTESIAN_POINT('Ctrl Pts',(42.5250812274693,-2.33997904850905,-4.41078685144686));
#27664=CARTESIAN_POINT('Ctrl Pts',(42.5647175604676,-1.56410733279554,-4.7414763961815));
#27665=CARTESIAN_POINT('Ctrl Pts',(42.6043538934659,-0.756326335255354,
-4.86693625596787));
#27666=CARTESIAN_POINT('Ctrl Pts',(42.6439902264642,0.0514546622848183,
-4.99239611575423));
#27667=CARTESIAN_POINT('Ctrl Pts',(42.6836265594626,0.891144941651684,-4.91262629059232));
#27668=CARTESIAN_POINT('Ctrl Pts',(42.7232628924609,1.66074315118674,-4.63702688099208));
#27669=CARTESIAN_POINT('Ctrl Pts',(42.7628992254592,2.43034136072179,-4.36142747139185));
#27670=CARTESIAN_POINT('Ctrl Pts',(42.8025355584575,3.12984750042507,-3.88999847735328));
#27671=CARTESIAN_POINT('Ctrl Pts',(42.8421718914558,3.67426005949087,-3.28016527711588));
#27672=CARTESIAN_POINT('Ctrl Pts',(42.8818082244541,4.21867261855668,-2.67033207687847));
#27673=CARTESIAN_POINT('Ctrl Pts',(42.9214445574525,4.60799159698502,-1.92209467044223));
#27674=CARTESIAN_POINT('Ctrl Pts',(42.9610808904508,4.79491986130557,-1.12629121671947));
#27675=CARTESIAN_POINT('Ctrl Pts',(43.0007172234491,4.98184812562611,-0.330487762996699));
#27676=CARTESIAN_POINT('Ctrl Pts',(43.0403535564475,4.96638567583886,0.512881738012616));
#27677=CARTESIAN_POINT('Ctrl Pts',(43.0799898894458,4.7504084749811,1.30131039653013));
#27678=CARTESIAN_POINT('Ctrl Pts',(43.1196262224441,4.53443127412335,2.08973905504764));
#27679=CARTESIAN_POINT('Ctrl Pts',(43.1592625554424,4.11793932219513,2.82322687107334));
#27680=CARTESIAN_POINT('Ctrl Pts',(43.1988988884407,3.55153812862758,3.41267285313056));
#27681=CARTESIAN_POINT('Ctrl Pts',(43.2385352214391,2.98513693506004,4.00211883518778));
#27682=CARTESIAN_POINT('Ctrl Pts',(43.2781715544374,2.26882649985319,4.44752298327648));
#27683=CARTESIAN_POINT('Ctrl Pts',(43.3178078874357,1.48963848090206,4.69475907111567));
#27684=CARTESIAN_POINT('Ctrl Pts',(43.357444220434,0.710450461950941,4.94199515895486));
#27685=CARTESIAN_POINT('Ctrl Pts',(43.3970805534323,-0.131615140744488,
4.99106318654455));
#27686=CARTESIAN_POINT('Ctrl Pts',(43.4367168864306,-0.934246273828332,
4.83600597226192));
#27687=CARTESIAN_POINT('Ctrl Pts',(43.476353219429,-1.73687740691221,4.68094875797928));
#27688=CARTESIAN_POINT('Ctrl Pts',(43.5159895524273,-2.50007407038453,4.32176630182432));
#27689=CARTESIAN_POINT('Ctrl Pts',(43.5556258854256,-3.13110737352768,3.80209726824003));
#27690=CARTESIAN_POINT('Ctrl Pts',(43.5952622184239,-3.76214067667083,3.28242823465576));
#27691=CARTESIAN_POINT('Ctrl Pts',(43.6348985514223,-4.26101061948481,2.60227262364216));
#27692=CARTESIAN_POINT('Ctrl Pts',(43.6745348844206,-4.56710398015465,1.84427110008394));
#27693=CARTESIAN_POINT('Ctrl Pts',(43.7050760809792,-4.80295974143054,1.26020411478287));
#27694=CARTESIAN_POINT('Ctrl Pts',(43.7356172775378,-4.92435927308213,0.62991808387772));
#27695=CARTESIAN_POINT('Ctrl Pts',(43.7661584740964,-4.92500388850328,-0.000126728605493087));
#27696=CARTESIAN_POINT('Origin',(41.25,0.,0.));
#27697=CARTESIAN_POINT('',(45.4838415259036,-4.92470113209118,9.20081859334676E-5));
#27698=CARTESIAN_POINT('',(45.2661584740964,-4.92466880697525,8.05726078428837E-5));
#27699=CARTESIAN_POINT('',(41.25,-4.925,-6.03138548580071E-16));
#27700=CARTESIAN_POINT('Ctrl Pts',(45.4838415259036,-4.92470113209118,9.20081859334676E-5));
#27701=CARTESIAN_POINT('Ctrl Pts',(45.4693810373698,-4.92490179872926,0.298455085306509));
#27702=CARTESIAN_POINT('Ctrl Pts',(45.4549205488361,-4.89822119016455,0.59678269783049));
#27703=CARTESIAN_POINT('Ctrl Pts',(45.4404600603023,-4.84432450427108,0.890109553198539));
#27704=CARTESIAN_POINT('Ctrl Pts',(45.400823727304,-4.69659318906749,1.69412118043862));
#27705=CARTESIAN_POINT('Ctrl Pts',(45.3611873943056,-4.34438389857107,2.46056146020548));
#27706=CARTESIAN_POINT('Ctrl Pts',(45.3215510613073,-3.83049037024208,3.09630722682097));
#27707=CARTESIAN_POINT('Ctrl Pts',(45.281914728309,-3.3165968419131,3.73205299343644));
#27708=CARTESIAN_POINT('Ctrl Pts',(45.2422783953107,-2.64101907575149,4.23710424690058));
#27709=CARTESIAN_POINT('Ctrl Pts',(45.2026420623124,-1.88584036240152,4.55009681731105));
#27710=CARTESIAN_POINT('Ctrl Pts',(45.1630057293141,-1.1306616490515,4.86308938772155));
#27711=CARTESIAN_POINT('Ctrl Pts',(45.1233693963157,-0.29588198851312,4.9840232750784));
#27712=CARTESIAN_POINT('Ctrl Pts',(45.0837330633174,0.517072158884537,4.8982049060758));
#27713=CARTESIAN_POINT('Ctrl Pts',(45.0440967303191,1.33002630628219,4.8123865370732));
#27714=CARTESIAN_POINT('Ctrl Pts',(45.0044603973208,2.12115494053905,4.51981591171113));
#27715=CARTESIAN_POINT('Ctrl Pts',(44.9648240643225,2.79433523927099,4.05604061738936));
#27716=CARTESIAN_POINT('Ctrl Pts',(44.9251877313242,3.46751553800291,3.59226532306761));
#27717=CARTESIAN_POINT('Ctrl Pts',(44.8855513983258,4.02274750120992,2.95728535978618));
#27718=CARTESIAN_POINT('Ctrl Pts',(44.8459150653275,4.39256995877785,2.22825134952313));
#27719=CARTESIAN_POINT('Ctrl Pts',(44.8062787323291,4.76239241634577,1.49921733926011));
#27720=CARTESIAN_POINT('Ctrl Pts',(44.7666423993308,4.94680536827464,0.67612928201546));
#27721=CARTESIAN_POINT('Ctrl Pts',(44.7270060663325,4.92340247928476,-0.141006901853086));
#27722=CARTESIAN_POINT('Ctrl Pts',(44.6873697333342,4.89999959029487,-0.958143085721712));
#27723=CARTESIAN_POINT('Ctrl Pts',(44.6477334003359,4.66878086038622,-1.76932739621425));
#27724=CARTESIAN_POINT('Ctrl Pts',(44.6080970673376,4.25783956788869,-2.47600022885704));
#27725=CARTESIAN_POINT('Ctrl Pts',(44.5684607343393,3.84689827539119,-3.18267306149978));
#27726=CARTESIAN_POINT('Ctrl Pts',(44.5288244013409,3.25623442030485,-3.78483441629277));
#27727=CARTESIAN_POINT('Ctrl Pts',(44.4891880683426,2.55761417863557,-4.20932116061901));
#27728=CARTESIAN_POINT('Ctrl Pts',(44.4495517353443,1.85899393696629,-4.63380790494526));
#27729=CARTESIAN_POINT('Ctrl Pts',(44.409915402346,1.05241730871404,-4.88062003880476));
#27730=CARTESIAN_POINT('Ctrl Pts',(44.3702790693477,0.235884061122376,-4.91976967222236));
#27731=CARTESIAN_POINT('Ctrl Pts',(44.3306427363493,-0.580649186469257,
-4.95891930563996));
#27732=CARTESIAN_POINT('Ctrl Pts',(44.291006403351,-1.40713905340033,-4.79040643861569));
#27733=CARTESIAN_POINT('Ctrl Pts',(44.2513700703527,-2.14316629663364,-4.43470553100115));
#27734=CARTESIAN_POINT('Ctrl Pts',(44.2117337373544,-2.87919353986696,-4.0790046233866));
#27735=CARTESIAN_POINT('Ctrl Pts',(44.172097404356,-3.52475815940249,-3.53611567518177));
#27736=CARTESIAN_POINT('Ctrl Pts',(44.1324610713577,-4.00142348800549,-2.8720001717005));
#27737=CARTESIAN_POINT('Ctrl Pts',(44.0928247383594,-4.47808881660849,-2.20788466821924));
#27738=CARTESIAN_POINT('Ctrl Pts',(44.0531884053611,-4.78585485427895,-1.42254260946154));
#27739=CARTESIAN_POINT('Ctrl Pts',(44.0135520723628,-4.88732775813964,-0.61139373915575));
#27740=CARTESIAN_POINT('Ctrl Pts',(44.0036485568764,-4.91268173008443,-0.408720464633004));
#27741=CARTESIAN_POINT('Ctrl Pts',(43.99374504139,-4.92515686621733,-0.204436076436149));
#27742=CARTESIAN_POINT('Ctrl Pts',(43.9838415259036,-4.92495182736585,-0.000126817358605258));
#27743=CARTESIAN_POINT('Ctrl Pts',(43.7661584740964,-4.92500388850328,-0.000126728605493087));
#27744=CARTESIAN_POINT('Ctrl Pts',(43.7752536105361,-4.9251958543025,-0.18775341578092));
#27745=CARTESIAN_POINT('Ctrl Pts',(43.7843487469758,-4.91467876478723,-0.375358710689233));
#27746=CARTESIAN_POINT('Ctrl Pts',(43.7934438834155,-4.89328627121904,-0.561715594621382));
#27747=CARTESIAN_POINT('Ctrl Pts',(43.8330802164138,-4.8000584230879,-1.37385332966565));
#27748=CARTESIAN_POINT('Ctrl Pts',(43.8727165494122,-4.50028594829992,-2.16228136365135));
#27749=CARTESIAN_POINT('Ctrl Pts',(43.9123528824105,-4.03039144350975,-2.8312047076203));
#27750=CARTESIAN_POINT('Ctrl Pts',(43.9519892154088,-3.56049693871958,-3.50012805158925));
#27751=CARTESIAN_POINT('Ctrl Pts',(43.9916255484071,-2.92048040392721,-4.04954670554145));
#27752=CARTESIAN_POINT('Ctrl Pts',(44.0312618814054,-2.18810441989724,-4.41270596780624));
#27753=CARTESIAN_POINT('Ctrl Pts',(44.0708982144038,-1.45572843586724,-4.77586523007105));
#27754=CARTESIAN_POINT('Ctrl Pts',(44.1105345474021,-0.630993002599663,
-4.95276510064842));
#27755=CARTESIAN_POINT('Ctrl Pts',(44.1501708804004,0.185895807452519,-4.92191201692444));
#27756=CARTESIAN_POINT('Ctrl Pts',(44.1898072133987,1.00278461750467,-4.89105893320045));
#27757=CARTESIAN_POINT('Ctrl Pts',(44.2294435463971,1.8118268043414,-4.65245289517512));
#27758=CARTESIAN_POINT('Ctrl Pts',(44.2690798793954,2.51472303050596,-4.23508478231541));
#27759=CARTESIAN_POINT('Ctrl Pts',(44.3087162123937,3.21761925667052,-3.8177166694557));
#27760=CARTESIAN_POINT('Ctrl Pts',(44.348352545392,3.81436952216293,-3.2215864817616));
#27761=CARTESIAN_POINT('Ctrl Pts',(44.3879888783903,4.23246814812435,-2.51912454105487));
#27762=CARTESIAN_POINT('Ctrl Pts',(44.4276252113887,4.65056677408577,-1.81666260034813));
#27763=CARTESIAN_POINT('Ctrl Pts',(44.467261544387,4.89001376051621,-1.00786890662875));
#27764=CARTESIAN_POINT('Ctrl Pts',(44.5068978773853,4.92171608803313,-0.19101261171286));
#27765=CARTESIAN_POINT('Ctrl Pts',(44.5465342103836,4.95341841555005,0.625843683203033));
#27766=CARTESIAN_POINT('Ctrl Pts',(44.5861705433819,4.77737608415345,1.45076257931545));
#27767=CARTESIAN_POINT('Ctrl Pts',(44.6258068763803,4.4149783917305,2.18351571243843));
#27768=CARTESIAN_POINT('Ctrl Pts',(44.6654432093786,4.05258069930754,2.91626884556144));
#27769=CARTESIAN_POINT('Ctrl Pts',(44.7050795423769,3.50382764585821,3.55685621569501));
#27770=CARTESIAN_POINT('Ctrl Pts',(44.7447158753752,2.83539320811387,4.02744589365957));
#27771=CARTESIAN_POINT('Ctrl Pts',(44.7843522083735,2.16695877036953,4.49803557162413));
#27772=CARTESIAN_POINT('Ctrl Pts',(44.8239885413719,1.37884294833018,4.79862755741967));
#27773=CARTESIAN_POINT('Ctrl Pts',(44.8636248743702,0.566802505140043,4.89269966250424));
#27774=CARTESIAN_POINT('Ctrl Pts',(44.9032612073685,-0.245237938050057,
4.98677176758881));
#27775=CARTESIAN_POINT('Ctrl Pts',(44.9428975403668,-1.08120300239091,4.87432399196243));
#27776=CARTESIAN_POINT('Ctrl Pts',(44.9825338733651,-1.83952219999503,4.56901883832726));
#27777=CARTESIAN_POINT('Ctrl Pts',(45.0221702063635,-2.59784139759917,4.26371368469208));
#27778=CARTESIAN_POINT('Ctrl Pts',(45.0618065393618,-3.27851472846656,3.76555115304811));
#27779=CARTESIAN_POINT('Ctrl Pts',(45.1014428723601,-3.79883978635438,3.1350584278558));
#27780=CARTESIAN_POINT('Ctrl Pts',(45.1410792053584,-4.31916484424219,2.50456570266349));
#27781=CARTESIAN_POINT('Ctrl Pts',(45.1807155383568,-4.67914162915044,1.74174278392284));
#27782=CARTESIAN_POINT('Ctrl Pts',(45.2203518713551,-4.83503264625132,0.93927332462865));
#27783=CARTESIAN_POINT('Ctrl Pts',(45.2356207389355,-4.89508561071691,0.63014281268565));
#27784=CARTESIAN_POINT('Ctrl Pts',(45.250889606516,-4.92485274797344,0.315128851399062));
#27785=CARTESIAN_POINT('Ctrl Pts',(45.2661584740964,-4.92466880697525,8.05726078428837E-5));
#27786=CARTESIAN_POINT('Origin',(41.25,0.,0.));
#27787=CARTESIAN_POINT('',(46.9838415259036,-4.92541598660193,-1.76250313788096E-5));
#27788=CARTESIAN_POINT('',(46.7661584740964,-4.92542130869464,-7.54510152246871E-8));
#27789=CARTESIAN_POINT('',(41.25,-4.925,-6.03138548580071E-16));
#27790=CARTESIAN_POINT('Ctrl Pts',(46.9838415259036,-4.92541598660193,-1.76250313788096E-5));
#27791=CARTESIAN_POINT('Ctrl Pts',(46.9450170333497,-4.92525305960927,0.8007125042042));
#27792=CARTESIAN_POINT('Ctrl Pts',(46.9061925407958,-4.72610526188126,1.60152074077725));
#27793=CARTESIAN_POINT('Ctrl Pts',(46.8673680482419,-4.35075866585062,2.30882523177979));
#27794=CARTESIAN_POINT('Ctrl Pts',(46.8277317152435,-3.96756337619178,3.03091982960743));
#27795=CARTESIAN_POINT('Ctrl Pts',(46.7880953822452,-3.40072342726273,3.65555937291029));
#27796=CARTESIAN_POINT('Ctrl Pts',(46.7484590492469,-2.71911036961906,4.10684960976261));
#27797=CARTESIAN_POINT('Ctrl Pts',(46.7088227162486,-2.03749731197539,4.55813984661494));
#27798=CARTESIAN_POINT('Ctrl Pts',(46.6691863832502,-1.24111114561709,4.83608077701674));
#27799=CARTESIAN_POINT('Ctrl Pts',(46.6295500502519,-0.426713487684489,
4.90690233434551));
#27800=CARTESIAN_POINT('Ctrl Pts',(46.5899137172536,0.387684170248116,4.97772389167427));
#27801=CARTESIAN_POINT('Ctrl Pts',(46.5502773842553,1.22009331975503,4.84142607593));
#27802=CARTESIAN_POINT('Ctrl Pts',(46.510641051257,1.96937551967397,4.51456919117275));
#27803=CARTESIAN_POINT('Ctrl Pts',(46.4710047182587,2.71865771959291,4.18771230641549));
#27804=CARTESIAN_POINT('Ctrl Pts',(46.4313683852603,3.38481296992387,3.67029635264524));
#27805=CARTESIAN_POINT('Ctrl Pts',(46.391732052262,3.88690282395414,3.02518782169216));
#27806=CARTESIAN_POINT('Ctrl Pts',(46.3520957192637,4.38899267798441,2.38007929073908));
#27807=CARTESIAN_POINT('Ctrl Pts',(46.3124593862653,4.72701713571399,1.60727818260316));
#27808=CARTESIAN_POINT('Ctrl Pts',(46.272823053267,4.85990592929473,0.800680509181498));
#27809=CARTESIAN_POINT('Ctrl Pts',(46.2331867202687,4.99279472287548,-0.00591716424018909));
#27810=CARTESIAN_POINT('Ctrl Pts',(46.1935503872704,4.92054785230737,-0.846311402947627));
#27811=CARTESIAN_POINT('Ctrl Pts',(46.1539140542721,4.65194337567933,-1.61839357044276));
#27812=CARTESIAN_POINT('Ctrl Pts',(46.1142777212738,4.38333889905129,-2.39047573793788));
#27813=CARTESIAN_POINT('Ctrl Pts',(46.0746413882754,3.91837681636332,-3.0942458342207));
#27814=CARTESIAN_POINT('Ctrl Pts',(46.0350050552771,3.31355042814016,-3.64419517583092));
#27815=CARTESIAN_POINT('Ctrl Pts',(45.9953687222788,2.708724039917,-4.19414451744114));
#27816=CARTESIAN_POINT('Ctrl Pts',(45.9557323892805,1.96403334615864,-4.59027310437877));
#27817=CARTESIAN_POINT('Ctrl Pts',(45.9160960562822,1.16995891878022,-4.78445096617617));
#27818=CARTESIAN_POINT('Ctrl Pts',(45.8764597232838,0.375884491401773,-4.97862882797357));
#27819=CARTESIAN_POINT('Ctrl Pts',(45.8368233902855,-0.467573669596737,
-4.97085596463074));
#27820=CARTESIAN_POINT('Ctrl Pts',(45.7971870572872,-1.25793465847378,-4.76207678585587));
#27821=CARTESIAN_POINT('Ctrl Pts',(45.7575507242889,-2.0482956473508,-4.55329760708101));
#27822=CARTESIAN_POINT('Ctrl Pts',(45.7179143912906,-2.78555946410635,-4.14351211287411));
#27823=CARTESIAN_POINT('Ctrl Pts',(45.6782780582922,-3.38014790888984,-3.58250959990415));
#27824=CARTESIAN_POINT('Ctrl Pts',(45.6386417252939,-3.97473635367333,-3.02150708693418));
#27825=CARTESIAN_POINT('Ctrl Pts',(45.5990053922956,-4.42664942648476,-2.30928755520114));
#27826=CARTESIAN_POINT('Ctrl Pts',(45.5593690592973,-4.6809792929351,-1.53238630197798));
#27827=CARTESIAN_POINT('Ctrl Pts',(45.5341932148327,-4.84252221772373,-1.03892125019597));
#27828=CARTESIAN_POINT('Ctrl Pts',(45.5090173703681,-4.92435176961579,-0.519360872400719));
#27829=CARTESIAN_POINT('Ctrl Pts',(45.4838415259036,-4.92470113209118,9.20081859334676E-5));
#27830=CARTESIAN_POINT('Ctrl Pts',(45.2661584740964,-4.92466880697525,8.05726078428837E-5));
#27831=CARTESIAN_POINT('Ctrl Pts',(45.2905259395143,-4.9243752569861,-0.50270249221085));
#27832=CARTESIAN_POINT('Ctrl Pts',(45.3148934049322,-4.84780015486276,-1.00557295930924));
#27833=CARTESIAN_POINT('Ctrl Pts',(45.33926087035,-4.69630409857361,-1.48475684285591));
#27834=CARTESIAN_POINT('Ctrl Pts',(45.3788972033484,-4.44987928450151,-2.26420155119845));
#27835=CARTESIAN_POINT('Ctrl Pts',(45.4185335363467,-4.00522440706378,-2.98097496803579));
#27836=CARTESIAN_POINT('Ctrl Pts',(45.458169869345,-3.41636542355341,-3.54798849510125));
#27837=CARTESIAN_POINT('Ctrl Pts',(45.4978062023433,-2.82750644004303,-4.11500202216671));
#27838=CARTESIAN_POINT('Ctrl Pts',(45.5374425353416,-2.09444335046,-4.53225565946027));
#27839=CARTESIAN_POINT('Ctrl Pts',(45.5770788683399,-1.30624396262072,-4.74905272436441));
#27840=CARTESIAN_POINT('Ctrl Pts',(45.6167152013383,-0.518044574781435,
-4.96584978926855));
#27841=CARTESIAN_POINT('Ctrl Pts',(45.6563515343366,0.325291111314094,-4.98219028178326));
#27842=CARTESIAN_POINT('Ctrl Pts',(45.6959878673349,1.12129707073172,-4.79608881775695));
#27843=CARTESIAN_POINT('Ctrl Pts',(45.7356242003332,1.91730303014935,-4.60998735373063));
#27844=CARTESIAN_POINT('Ctrl Pts',(45.7752605333315,2.66597926288907,-4.22144393316328));
#27845=CARTESIAN_POINT('Ctrl Pts',(45.8148968663299,3.27636095055706,-3.67766692215644));
#27846=CARTESIAN_POINT('Ctrl Pts',(45.8545331993282,3.88674263822504,-3.1338899111496));
#27847=CARTESIAN_POINT('Ctrl Pts',(45.8941695323265,4.35882978082128,-2.43487930970328));
#27848=CARTESIAN_POINT('Ctrl Pts',(45.9338058653249,4.63526337679785,-1.6655655184864));
#27849=CARTESIAN_POINT('Ctrl Pts',(45.9734421983232,4.91169697277443,-0.896251727269502));
#27850=CARTESIAN_POINT('Ctrl Pts',(46.0130785313215,4.99247702213132,-0.0566347462819967));
#27851=CARTESIAN_POINT('Ctrl Pts',(46.0527148643198,4.86778867807864,0.751271225473264));
#27852=CARTESIAN_POINT('Ctrl Pts',(46.0923511973181,4.74310033402597,1.5591771972285));
#27853=CARTESIAN_POINT('Ctrl Pts',(46.1319875303164,4.41294359656375,2.33537215975155));
#27854=CARTESIAN_POINT('Ctrl Pts',(46.1716238633147,3.91743279863258,2.98554774486244));
#27855=CARTESIAN_POINT('Ctrl Pts',(46.2112601963131,3.42192200070141,3.63572332997333));
#27856=CARTESIAN_POINT('Ctrl Pts',(46.2508965293114,2.76105714230129,4.15987953767205));
#27857=CARTESIAN_POINT('Ctrl Pts',(46.2905328623097,2.01513388288903,4.4943309293695));
#27858=CARTESIAN_POINT('Ctrl Pts',(46.3301691953081,1.26921062347679,4.82878232106693));
#27859=CARTESIAN_POINT('Ctrl Pts',(46.3698055283064,0.438228963052423,4.9735288967631));
#27860=CARTESIAN_POINT('Ctrl Pts',(46.4094418613047,-0.376846098396358,
4.91098382065942));
#27861=CARTESIAN_POINT('Ctrl Pts',(46.449078194303,-1.19192115984518,4.84843874455575));
#27862=CARTESIAN_POINT('Ctrl Pts',(46.4887145273013,-1.99108962231841,4.5786020166522));
#27863=CARTESIAN_POINT('Ctrl Pts',(46.5283508602997,-2.67725181725943,4.13425903586556));
#27864=CARTESIAN_POINT('Ctrl Pts',(46.567987193298,-3.36341401220043,3.68991605507894));
#27865=CARTESIAN_POINT('Ctrl Pts',(46.6076235262963,-3.93656993960923,3.07106682140923));
#27866=CARTESIAN_POINT('Ctrl Pts',(46.6472598592946,-4.32708065200984,2.35290205908728));
#27867=CARTESIAN_POINT('Ctrl Pts',(46.6868927308952,-4.71755726153596,1.63480001331054));
#27868=CARTESIAN_POINT('Ctrl Pts',(46.7265256024958,-4.92542055507572,0.817399784357684));
#27869=CARTESIAN_POINT('Ctrl Pts',(46.7661584740964,-4.92542130864622,-7.54510065536516E-8));
#27870=CARTESIAN_POINT('Origin',(41.25,0.,0.));
#27871=CARTESIAN_POINT('',(48.4838415259036,-4.92464095784815,-6.78464642470123E-5));
#27872=CARTESIAN_POINT('',(48.2661584740964,-4.924668549948,-8.0469304329367E-5));
#27873=CARTESIAN_POINT('',(41.25,-4.925,-6.03138548580071E-16));
#27874=CARTESIAN_POINT('Ctrl Pts',(48.4838415259036,-4.92464095784815,-6.78464642470123E-5));
#27875=CARTESIAN_POINT('Ctrl Pts',(48.4602893623278,-4.92440377657073,0.485900652092098));
#27876=CARTESIAN_POINT('Ctrl Pts',(48.4367371987521,-4.85294368865689,0.971937392632399));
#27877=CARTESIAN_POINT('Ctrl Pts',(48.4131850351763,-4.71126924513192,1.43656431086514));
#27878=CARTESIAN_POINT('Ctrl Pts',(48.373548702178,-4.47284293653205,2.21849278176001));
#27879=CARTESIAN_POINT('Ctrl Pts',(48.3339123691797,-4.03555488870416,2.93978415837996));
#27880=CARTESIAN_POINT('Ctrl Pts',(48.2942760361814,-3.45253598268484,3.51280090634862));
#27881=CARTESIAN_POINT('Ctrl Pts',(48.2546397031831,-2.86951707666548,4.08581765431731));
#27882=CARTESIAN_POINT('Ctrl Pts',(48.2150033701847,-2.14076731245468,4.51055977363469));
#27883=CARTESIAN_POINT('Ctrl Pts',(48.1753670371864,-1.3548304250574,4.73542072457306));
#27884=CARTESIAN_POINT('Ctrl Pts',(48.1357307041881,-0.568893537660152,
4.96028167551142));
#27885=CARTESIAN_POINT('Ctrl Pts',(48.0960943711898,0.274230472923564,4.98526145807077));
#27886=CARTESIAN_POINT('Ctrl Pts',(48.0564580381915,1.07210130052046,4.80732500677867));
#27887=CARTESIAN_POINT('Ctrl Pts',(48.0168217051931,1.86997212811736,4.62938855548657));
#27888=CARTESIAN_POINT('Ctrl Pts',(47.9771853721948,2.62258977272744,4.24853587034301));
#27889=CARTESIAN_POINT('Ctrl Pts',(47.9375490391965,3.23851053096014,3.71104088636025));
#27890=CARTESIAN_POINT('Ctrl Pts',(47.8979127061982,3.85443128919285,3.17354590237749));
#27891=CARTESIAN_POINT('Ctrl Pts',(47.8582763731999,4.33365516104819,2.47940861955552));
#27892=CARTESIAN_POINT('Ctrl Pts',(47.8186400402016,4.617956026119,1.7129673260773));
#27893=CARTESIAN_POINT('Ctrl Pts',(47.7790037072032,4.90225689118982,0.946526032599082));
#27894=CARTESIAN_POINT('Ctrl Pts',(47.7393673742049,4.99163474947611,0.107780728464605));
#27895=CARTESIAN_POINT('Ctrl Pts',(47.6997310412066,4.87523011286816,-0.701360296823789));
#27896=CARTESIAN_POINT('Ctrl Pts',(47.6600947082082,4.7588254762602,-1.51050132211221));
#27897=CARTESIAN_POINT('Ctrl Pts',(47.6204583752099,4.43663834475798,-2.29003806855454));
#27898=CARTESIAN_POINT('Ctrl Pts',(47.5808220422116,3.94781473719369,-2.94525613829656));
#27899=CARTESIAN_POINT('Ctrl Pts',(47.5411857092133,3.45899112962941,-3.60047420803855));
#27900=CARTESIAN_POINT('Ctrl Pts',(47.501549376215,2.80353104600308,-4.13137360108024));
#27901=CARTESIAN_POINT('Ctrl Pts',(47.4619130432166,2.06107346089987,-4.47344957590353));
#27902=CARTESIAN_POINT('Ctrl Pts',(47.4222767102183,1.31861587579667,-4.81552555072681));
#27903=CARTESIAN_POINT('Ctrl Pts',(47.38264037722,0.489160789216602,-4.9687781073317));
#27904=CARTESIAN_POINT('Ctrl Pts',(47.3430040442217,-0.326512278912506,
-4.91458692578498));
#27905=CARTESIAN_POINT('Ctrl Pts',(47.3033677112234,-1.14218534704164,-4.86039574423825));
#27906=CARTESIAN_POINT('Ctrl Pts',(47.263731378225,-1.94407639671981,-4.59876082453989));
#27907=CARTESIAN_POINT('Ctrl Pts',(47.2240950452267,-2.63475496265902,-4.16147103872187));
#27908=CARTESIAN_POINT('Ctrl Pts',(47.1844587122284,-3.3254335285982,-3.72418125290388));
#27909=CARTESIAN_POINT('Ctrl Pts',(47.1448223792301,-3.90489961079844,-3.11123660096624));
#27910=CARTESIAN_POINT('Ctrl Pts',(47.1051860462318,-4.30274757244656,-2.3971103952848));
#27911=CARTESIAN_POINT('Ctrl Pts',(47.0655497132335,-4.7005955340947,-1.68298418960333));
#27912=CARTESIAN_POINT('Ctrl Pts',(47.0259133802351,-4.91682537519071,-0.867676430178051));
#27913=CARTESIAN_POINT('Ctrl Pts',(46.9862770472368,-4.92516498054441,-0.0502477242891959));
#27914=CARTESIAN_POINT('Ctrl Pts',(46.9854652067924,-4.92533579425003,-0.0335049624427779));
#27915=CARTESIAN_POINT('Ctrl Pts',(46.984653366348,-4.92541939349056,-0.0167613108132938));
#27916=CARTESIAN_POINT('Ctrl Pts',(46.9838415259036,-4.92541598660193,-1.76250313788096E-5));
#27917=CARTESIAN_POINT('Ctrl Pts',(46.7661584740964,-4.92542130864622,-7.54510065536516E-8));
#27918=CARTESIAN_POINT('Ctrl Pts',(46.8057982684924,-4.92542206234836,-0.817542713004385));
#27919=CARTESIAN_POINT('Ctrl Pts',(46.8454380628885,-4.71748324187784,-1.63508498109272));
#27920=CARTESIAN_POINT('Ctrl Pts',(46.8850778572845,-4.32687594630263,-2.35327848202517));
#27921=CARTESIAN_POINT('Ctrl Pts',(46.9247141902829,-3.9363027590578,-3.07140926937937));
#27922=CARTESIAN_POINT('Ctrl Pts',(46.9643505232812,-3.36309299739203,-3.69020863934389));
#27923=CARTESIAN_POINT('Ctrl Pts',(47.0039868562795,-2.67689214969072,-4.13449192617173));
#27924=CARTESIAN_POINT('Ctrl Pts',(47.0436231892778,-1.99069130198939,-4.57877521299958));
#27925=CARTESIAN_POINT('Ctrl Pts',(47.0832595222761,-1.19149936825251,-4.84854241669076));
#27926=CARTESIAN_POINT('Ctrl Pts',(47.1228958552744,-0.376418868815787,
-4.91101658558128));
#27927=CARTESIAN_POINT('Ctrl Pts',(47.1625321882728,0.438661630620939,-4.97349075447181));
#27928=CARTESIAN_POINT('Ctrl Pts',(47.2021685212711,1.26963069575751,-4.82867188856169));
#27929=CARTESIAN_POINT('Ctrl Pts',(47.2418048542694,2.01552485694469,-4.49415560697369));
#27930=CARTESIAN_POINT('Ctrl Pts',(47.2814411872677,2.7614190181319,-4.15963932538569));
#27931=CARTESIAN_POINT('Ctrl Pts',(47.3210775202661,3.4222382753697,-3.6354256281198));
#27932=CARTESIAN_POINT('Ctrl Pts',(47.3607138532644,3.9176925097825,-2.98520693879824));
#27933=CARTESIAN_POINT('Ctrl Pts',(47.4003501862627,4.41314674419528,-2.33498824947669));
#27934=CARTESIAN_POINT('Ctrl Pts',(47.439986519261,4.74323595578306,-1.55876456809948));
#27935=CARTESIAN_POINT('Ctrl Pts',(47.4796228522593,4.86785401605814,-0.750847752211934));
#27936=CARTESIAN_POINT('Ctrl Pts',(47.5192591852577,4.99247207633321,0.0570690636756077));
#27937=CARTESIAN_POINT('Ctrl Pts',(47.558895518256,4.91161898529556,0.896679014073474));
#27938=CARTESIAN_POINT('Ctrl Pts',(47.5985318512543,4.63511846436338,1.66596875420057));
#27939=CARTESIAN_POINT('Ctrl Pts',(47.6381681842526,4.35861794343121,2.43525849432767));
#27940=CARTESIAN_POINT('Ctrl Pts',(47.6778045172509,3.8864699926045,3.13422802418401));
#27941=CARTESIAN_POINT('Ctrl Pts',(47.7174408502492,3.27604100168431,3.67795193333712));
#27942=CARTESIAN_POINT('Ctrl Pts',(47.7570771832476,2.66561201076412,4.22167584249024));
#27943=CARTESIAN_POINT('Ctrl Pts',(47.7967135162459,1.91690197975045,4.61015413094014));
#27944=CARTESIAN_POINT('Ctrl Pts',(47.8363498492442,1.12087983355739,4.79618634619));
#27945=CARTESIAN_POINT('Ctrl Pts',(47.8759861822425,0.324857687364301,4.98221856143987));
#27946=CARTESIAN_POINT('Ctrl Pts',(47.9156225152409,-0.518476574008187,
4.96580470348969));
#27947=CARTESIAN_POINT('Ctrl Pts',(47.9552588482392,-1.3066570987317,4.74893907046501));
#27948=CARTESIAN_POINT('Ctrl Pts',(47.9948951812375,-2.09483762345518,4.53207343744033));
#27949=CARTESIAN_POINT('Ctrl Pts',(48.0345315142358,-2.8278644115297,4.11475602934116));
#27950=CARTESIAN_POINT('Ctrl Pts',(48.0741678472342,-3.41667406580256,3.54769127697538));
#27951=CARTESIAN_POINT('Ctrl Pts',(48.1138041802325,-4.00548372007542,2.98062652460961));
#27952=CARTESIAN_POINT('Ctrl Pts',(48.1534405132308,-4.45007624054664,2.26381442797724));
#27953=CARTESIAN_POINT('Ctrl Pts',(48.1930768462291,-4.69643324635205,1.48434828501067));
#27954=CARTESIAN_POINT('Ctrl Pts',(48.2174373888515,-4.84784458757054,1.00528736382791));
#27955=CARTESIAN_POINT('Ctrl Pts',(48.241797931474,-4.9243754795075,0.502559829996446));
#27956=CARTESIAN_POINT('Ctrl Pts',(48.2661584740964,-4.924668549948,-8.0469304329367E-5));
#27957=CARTESIAN_POINT('Origin',(41.25,0.,0.));
#27958=CARTESIAN_POINT('',(49.9838415259036,-4.92505697724291,0.000124540890093713));
#27959=CARTESIAN_POINT('',(49.7661584740964,-4.92500433765405,0.000126715614453391));
#27960=CARTESIAN_POINT('',(41.25,-4.925,-6.03138548580071E-16));
#27961=CARTESIAN_POINT('Ctrl Pts',(49.9838415259036,-4.92505697724291,0.000124540890093713));
#27962=CARTESIAN_POINT('Ctrl Pts',(49.975561691306,-4.92523258911014,0.170926810624905));
#27963=CARTESIAN_POINT('Ctrl Pts',(49.9672818567084,-4.91652003640936,0.341711252245115));
#27964=CARTESIAN_POINT('Ctrl Pts',(49.9590020221109,-4.8987843370784,0.511553455647789));
#27965=CARTESIAN_POINT('Ctrl Pts',(49.9193656891125,-4.81388190619586,1.32460377107337));
#27966=CARTESIAN_POINT('Ctrl Pts',(49.8797293561142,-4.52220276134002,2.11606151681266));
#27967=CARTESIAN_POINT('Ctrl Pts',(49.8400930231159,-4.05918617416124,2.78976388302373));
#27968=CARTESIAN_POINT('Ctrl Pts',(49.8004566901176,-3.59616958698247,3.46346624923481));
#27969=CARTESIAN_POINT('Ctrl Pts',(49.7608203571192,-2.96181555748075,4.01941323591768));
#27970=CARTESIAN_POINT('Ctrl Pts',(49.7211840241209,-2.23319865620258,4.39005679703905));
#27971=CARTESIAN_POINT('Ctrl Pts',(49.6815476911226,-1.5045817549244,4.76070035816043));
#27972=CARTESIAN_POINT('Ctrl Pts',(49.6419113581243,-0.68170198186976,4.9460404937203));
#27973=CARTESIAN_POINT('Ctrl Pts',(49.602275025126,0.135460049406341,4.92355821479023));
#27974=CARTESIAN_POINT('Ctrl Pts',(49.5626386921276,0.952622080682418,4.90107593586015));
#27975=CARTESIAN_POINT('Ctrl Pts',(49.5230023591293,1.76406637017997,4.67077124244014));
#27976=CARTESIAN_POINT('Ctrl Pts',(49.483366026131,2.4712017255922,4.26062635662838));
#27977=CARTESIAN_POINT('Ctrl Pts',(49.4437296931327,3.17833708100444,3.85048147081662));
#27978=CARTESIAN_POINT('Ctrl Pts',(49.4040933601344,3.78116350233136,3.2604963926131));
#27979=CARTESIAN_POINT('Ctrl Pts',(49.364457027136,4.20643705108794,2.56235482605598));
#27980=CARTESIAN_POINT('Ctrl Pts',(49.3248206941377,4.63171059984453,1.86421325949884));
#27981=CARTESIAN_POINT('Ctrl Pts',(49.2851843611394,4.87943127603075,1.05791520458814));
#27982=CARTESIAN_POINT('Ctrl Pts',(49.2455480281411,4.91950080039325,0.241426581613654));
#27983=CARTESIAN_POINT('Ctrl Pts',(49.2059116951428,4.95957032475575,-0.575062041360806));
#27984=CARTESIAN_POINT('Ctrl Pts',(49.1662753621445,4.79198869729451,-1.40174123239899));
#27985=CARTESIAN_POINT('Ctrl Pts',(49.1266390291461,4.43711723261043,-2.13816874531611));
#27986=CARTESIAN_POINT('Ctrl Pts',(49.0870026961478,4.08224576792633,-2.87459625823325));
#27987=CARTESIAN_POINT('Ctrl Pts',(49.0473663631494,3.54008446601938,-3.52077209302934));
#27988=CARTESIAN_POINT('Ctrl Pts',(49.0077300301511,2.87650640020383,-3.99818531948745));
#27989=CARTESIAN_POINT('Ctrl Pts',(48.9680936971528,2.2129283343883,-4.47559854594555));
#27990=CARTESIAN_POINT('Ctrl Pts',(48.9284573641545,1.42793350466419,-4.7842491640657));
#27991=CARTESIAN_POINT('Ctrl Pts',(48.8888210311562,0.616899470788016,-4.88663585325509));
#27992=CARTESIAN_POINT('Ctrl Pts',(48.8491846981579,-0.194134563088155,
-4.98902254244449));
#27993=CARTESIAN_POINT('Ctrl Pts',(48.8095483651595,-1.03120780111639,-4.88514530270314));
#27994=CARTESIAN_POINT('Ctrl Pts',(48.7699120321612,-1.79261511129173,-4.58762530969411));
#27995=CARTESIAN_POINT('Ctrl Pts',(48.7302756991629,-2.55402242146707,-4.29010531668508));
#27996=CARTESIAN_POINT('Ctrl Pts',(48.6906393661646,-3.23976380378953,-3.79894257040838));
#27997=CARTESIAN_POINT('Ctrl Pts',(48.6510030331663,-3.76652107934467,-3.17381377497632));
#27998=CARTESIAN_POINT('Ctrl Pts',(48.6113667001679,-4.29327835489981,-2.54868497954427));
#27999=CARTESIAN_POINT('Ctrl Pts',(48.5717303671696,-4.66105152368764,-1.78959013495686));
#28000=CARTESIAN_POINT('Ctrl Pts',(48.5320940341713,-4.82515582339564,-0.98875993007825));
#28001=CARTESIAN_POINT('Ctrl Pts',(48.5160098647487,-4.89174829448995,-0.663788175135068));
#28002=CARTESIAN_POINT('Ctrl Pts',(48.4999256953262,-4.92480293293963,-0.331943923991882));
#28003=CARTESIAN_POINT('Ctrl Pts',(48.4838415259036,-4.92464095784815,-6.78464642470123E-5));
#28004=CARTESIAN_POINT('Ctrl Pts',(48.2661584740964,-4.924668549948,-8.0469304329367E-5));
#28005=CARTESIAN_POINT('Ctrl Pts',(48.2814342644723,-4.92485232592885,-0.315271635839327));
#28006=CARTESIAN_POINT('Ctrl Pts',(48.2967100548482,-4.89505801306927,-0.630428500180749));
#28007=CARTESIAN_POINT('Ctrl Pts',(48.311985845224,-4.83495091642528,-0.939693941883922));
#28008=CARTESIAN_POINT('Ctrl Pts',(48.3516221782224,-4.67899008955348,-1.74214983651119));
#28009=CARTESIAN_POINT('Ctrl Pts',(48.3912585112207,-4.31894694467024,-2.50494143646496));
#28010=CARTESIAN_POINT('Ctrl Pts',(48.430894844219,-3.79856703940939,-3.1353888938643));
#28011=CARTESIAN_POINT('Ctrl Pts',(48.4705311772174,-3.27818713414853,-3.76583635126364));
#28012=CARTESIAN_POINT('Ctrl Pts',(48.5101675102157,-2.59747046851005,-4.26393966610853));
#28013=CARTESIAN_POINT('Ctrl Pts',(48.549803843214,-1.83912471392769,-4.56917884912326));
#28014=CARTESIAN_POINT('Ctrl Pts',(48.5894401762123,-1.08077895934533,-4.87441803213799));
#28015=CARTESIAN_POINT('Ctrl Pts',(48.6290765092106,-0.244804115819099,
-4.98679308332255));
#28016=CARTESIAN_POINT('Ctrl Pts',(48.6687128422089,0.567228140540522,-4.89265033547606));
#28017=CARTESIAN_POINT('Ctrl Pts',(48.7083491752073,1.37926039690017,-4.79850758762956));
#28018=CARTESIAN_POINT('Ctrl Pts',(48.7479855082056,2.16735006609319,-4.49784704075199));
#28019=CARTESIAN_POINT('Ctrl Pts',(48.7876218412039,2.83574356265565,-4.02719921477844));
#28020=CARTESIAN_POINT('Ctrl Pts',(48.8272581742023,3.50413705921809,-3.55655138880489));
#28021=CARTESIAN_POINT('Ctrl Pts',(48.8668945072006,4.05283438314997,-2.91591628373537));
#28022=CARTESIAN_POINT('Ctrl Pts',(48.9065308401989,4.41516832873248,-2.18313162626826));
#28023=CARTESIAN_POINT('Ctrl Pts',(48.9461671731972,4.77750227431499,-1.45034696880114));
#28024=CARTESIAN_POINT('Ctrl Pts',(48.9858035061955,4.95347284154814,-0.62541275893643));
#28025=CARTESIAN_POINT('Ctrl Pts',(49.0254398391939,4.92169945229804,0.191440773880888));
#28026=CARTESIAN_POINT('Ctrl Pts',(49.0650761721922,4.88992606304794,1.00829430669821));
#28027=CARTESIAN_POINT('Ctrl Pts',(49.1047125051905,4.6504087173146,1.81706716246813));
#28028=CARTESIAN_POINT('Ctrl Pts',(49.1443488381888,4.23224898251004,2.5194927304316));
#28029=CARTESIAN_POINT('Ctrl Pts',(49.1839851711871,3.81408924770549,3.22191829839507));
#28030=CARTESIAN_POINT('Ctrl Pts',(49.2236215041854,3.21728712382973,3.81799657855207));
#28031=CARTESIAN_POINT('Ctrl Pts',(49.2632578371838,2.51435459195233,4.23530353747916));
#28032=CARTESIAN_POINT('Ctrl Pts',(49.3028941701821,1.81142206007491,4.65261049640625));
#28033=CARTESIAN_POINT('Ctrl Pts',(49.3425305031804,1.00235912019584,4.89114613410341));
#28034=CARTESIAN_POINT('Ctrl Pts',(49.3821668361787,0.185467628547644,4.92192816154557));
#28035=CARTESIAN_POINT('Ctrl Pts',(49.4218031691771,-0.631423863100528,
4.95271018898772));
#28036=CARTESIAN_POINT('Ctrl Pts',(49.4614395021754,-1.45614390651782,4.77573860617489));
#28037=CARTESIAN_POINT('Ctrl Pts',(49.5010758351737,-2.18848829367015,4.41251561551062));
#28038=CARTESIAN_POINT('Ctrl Pts',(49.540712168172,-2.92083268082247,4.04929262484635));
#28039=CARTESIAN_POINT('Ctrl Pts',(49.5803485011703,-3.56080141170983,3.49981822633064));
#28040=CARTESIAN_POINT('Ctrl Pts',(49.6199848341686,-4.03063772468131,2.83085404092629));
#28041=CARTESIAN_POINT('Ctrl Pts',(49.659621167167,-4.50047403765279,2.16188985552195));
#28042=CARTESIAN_POINT('Ctrl Pts',(49.6992575001653,-4.8001779327084,1.37343588322897));
#28043=CARTESIAN_POINT('Ctrl Pts',(49.7388938331636,-4.89333512394708,0.561289972655089));
#28044=CARTESIAN_POINT('Ctrl Pts',(49.7479820468079,-4.9146951336259,0.375073060360803));
#28045=CARTESIAN_POINT('Ctrl Pts',(49.7570702604521,-4.92519617945162,0.18761057069032));
#28046=CARTESIAN_POINT('Ctrl Pts',(49.7661584740964,-4.92500433765405,0.000126715614453391));
#28047=CARTESIAN_POINT('Origin',(41.25,0.,0.));
#28048=CARTESIAN_POINT('',(51.4838415259036,-4.9251402971202,-0.000116503725961781));
#28049=CARTESIAN_POINT('',(51.2661584740964,-4.92519062564324,-0.000109311139069327));
#28050=CARTESIAN_POINT('',(41.25,-4.925,-6.03138548580071E-16));
#28051=CARTESIAN_POINT('Ctrl Pts',(51.4838415259036,-4.9251402971202,-0.000116503725961781));
#28052=CARTESIAN_POINT('Ctrl Pts',(51.4511976872858,-4.9244646577768,0.67325086546852));
#28053=CARTESIAN_POINT('Ctrl Pts',(51.4185538486681,-4.78528364631617,1.34688857405293));
#28054=CARTESIAN_POINT('Ctrl Pts',(51.3859100100504,-4.51678498406586,1.96428798565576));
#28055=CARTESIAN_POINT('Ctrl Pts',(51.3462736770521,-4.19077239372136,2.71393783406419));
#28056=CARTESIAN_POINT('Ctrl Pts',(51.3066373440537,-3.67410739356836,3.38067582335991));
#28057=CARTESIAN_POINT('Ctrl Pts',(51.2670010110554,-3.02956496398235,3.88349220413633));
#28058=CARTESIAN_POINT('Ctrl Pts',(51.2273646780571,-2.38502253439632,4.38630858491276));
#28059=CARTESIAN_POINT('Ctrl Pts',(51.1877283450588,-1.61260267537726,4.7252033571699));
#28060=CARTESIAN_POINT('Ctrl Pts',(51.1480920120604,-0.806155212049699,
4.85900075945319));
#28061=CARTESIAN_POINT('Ctrl Pts',(51.1084556790621,0.000292251277839023,
4.99279816173648));
#28062=CARTESIAN_POINT('Ctrl Pts',(51.0688193460638,0.840767318913887,4.92149819404594));
#28063=CARTESIAN_POINT('Ctrl Pts',(51.0291830130655,1.61315160142145,4.65376373941843));
#28064=CARTESIAN_POINT('Ctrl Pts',(50.9895466800672,2.38553588392901,4.38602928479092));
#28065=CARTESIAN_POINT('Ctrl Pts',(50.9499103470689,3.0898293813081,3.92186034322643));
#28066=CARTESIAN_POINT('Ctrl Pts',(50.9102740140705,3.64045978239183,3.31765391083831));
#28067=CARTESIAN_POINT('Ctrl Pts',(50.8706376810722,4.19109018347557,2.7134474784502));
#28068=CARTESIAN_POINT('Ctrl Pts',(50.8310013480739,4.58805748826396,1.96920355523843));
#28069=CARTESIAN_POINT('Ctrl Pts',(50.7913650150756,4.78312983838864,1.17534839855546));
#28070=CARTESIAN_POINT('Ctrl Pts',(50.7517286820773,4.97820218851332,0.381493241872491));
#28071=CARTESIAN_POINT('Ctrl Pts',(50.7120923490789,4.9713795839743,-0.461973148281703));
#28072=CARTESIAN_POINT('Ctrl Pts',(50.6724560160806,4.76349096865269,-1.25256885049863));
#28073=CARTESIAN_POINT('Ctrl Pts',(50.6328196830823,4.55560235333107,-2.04316455271558));
#28074=CARTESIAN_POINT('Ctrl Pts',(50.593183350084,4.14664772722689,-2.7808895669952));
#28075=CARTESIAN_POINT('Ctrl Pts',(50.5535470170856,3.58631544009297,-3.37610966551359));
#28076=CARTESIAN_POINT('Ctrl Pts',(50.5139106840873,3.02598315295906,-3.97132976403196));
#28077=CARTESIAN_POINT('Ctrl Pts',(50.474274351089,2.31427320479544,-4.42404494678905));
#28078=CARTESIAN_POINT('Ctrl Pts',(50.4346380180907,1.53765897587531,-4.67924991835887));
#28079=CARTESIAN_POINT('Ctrl Pts',(50.3950016850924,0.761044746955179,-4.93445488992869));
#28080=CARTESIAN_POINT('Ctrl Pts',(50.355365352094,-0.0804737627214679,
-4.99214965031124));
#28081=CARTESIAN_POINT('Ctrl Pts',(50.3157290190957,-0.884651315671221,
-4.84532423755135));
#28082=CARTESIAN_POINT('Ctrl Pts',(50.2760926860974,-1.68882886862102,-4.69849882479145));
#28083=CARTESIAN_POINT('Ctrl Pts',(50.2364563530991,-2.45566546484393,-4.34715323888908));
#28084=CARTESIAN_POINT('Ctrl Pts',(50.1968200201008,-3.0919897864075,-3.83397627544034));
#28085=CARTESIAN_POINT('Ctrl Pts',(50.1571836871025,-3.72831410797102,-3.32079931199164));
#28086=CARTESIAN_POINT('Ctrl Pts',(50.1175473541041,-4.23412615487522,-2.64579097099658));
#28087=CARTESIAN_POINT('Ctrl Pts',(50.0779110211058,-4.5479693198727,-1.89096535794314));
#28088=CARTESIAN_POINT('Ctrl Pts',(50.0465545227051,-4.79625219462155,-1.29381909495384));
#28089=CARTESIAN_POINT('Ctrl Pts',(50.0151980243043,-4.92439191888106,-0.646719431010621));
#28090=CARTESIAN_POINT('Ctrl Pts',(49.9838415259036,-4.92505697724291,0.000124540890093713));
#28091=CARTESIAN_POINT('Ctrl Pts',(49.7661584740964,-4.92500433765405,0.000126715614453391));
#28092=CARTESIAN_POINT('Ctrl Pts',(49.7967065934505,-4.92435950178655,-0.630060844448721));
#28093=CARTESIAN_POINT('Ctrl Pts',(49.8272547128045,-4.8029035475925,-1.26048979660438));
#28094=CARTESIAN_POINT('Ctrl Pts',(49.8578028321585,-4.56694351136301,-1.84466854276718));
#28095=CARTESIAN_POINT('Ctrl Pts',(49.8974391651569,-4.26078422011854,-2.6026432987608));
#28096=CARTESIAN_POINT('Ctrl Pts',(49.9370754981552,-3.76185515020785,-3.28275496189324));
#28097=CARTESIAN_POINT('Ctrl Pts',(49.9767118311536,-3.1307766208679,-3.80236936907387));
#28098=CARTESIAN_POINT('Ctrl Pts',(50.0163481641519,-2.49969809152796,-4.3219837762545));
#28099=CARTESIAN_POINT('Ctrl Pts',(50.0559844971501,-1.73647010275876,-4.68110092748333));
#28100=CARTESIAN_POINT('Ctrl Pts',(50.0956208301485,-0.93382552407062,-4.83608777415021));
#28101=CARTESIAN_POINT('Ctrl Pts',(50.1352571631468,-0.131180945382506,
-4.99107462081708));
#28102=CARTESIAN_POINT('Ctrl Pts',(50.1748934961451,0.710880223224554,-4.94193116292202));
#28103=CARTESIAN_POINT('Ctrl Pts',(50.2145298291435,1.49004681182054,-4.69462837370072));
#28104=CARTESIAN_POINT('Ctrl Pts',(50.2541661621418,2.26921340041652,-4.44732558447941));
#28105=CARTESIAN_POINT('Ctrl Pts',(50.2938024951401,2.98548540900144,-4.00186346393186));
#28106=CARTESIAN_POINT('Ctrl Pts',(50.3334388281384,3.55183516079068,-3.41236605002642));
#28107=CARTESIAN_POINT('Ctrl Pts',(50.3730751611367,4.11818491257993,-2.82286863612097));
#28108=CARTESIAN_POINT('Ctrl Pts',(50.412711494135,4.5346124075735,-2.08933592885763));
#28109=CARTESIAN_POINT('Ctrl Pts',(50.4523478271334,4.75052134023217,-1.3008927951479));
#28110=CARTESIAN_POINT('Ctrl Pts',(50.4919841601317,4.96643027289085,-0.512449661438156));
#28111=CARTESIAN_POINT('Ctrl Pts',(50.53162049313,4.98182064321461,0.330903898717918));
#28112=CARTESIAN_POINT('Ctrl Pts',(50.5712568261284,4.79482250762883,1.12669968894037));
#28113=CARTESIAN_POINT('Ctrl Pts',(50.6108931591267,4.60782437204306,1.92249547916279));
#28114=CARTESIAN_POINT('Ctrl Pts',(50.650529492125,4.21843773054774,2.67073349945155));
#28115=CARTESIAN_POINT('Ctrl Pts',(50.6901658251233,3.67397340151565,3.28050217407564));
#28116=CARTESIAN_POINT('Ctrl Pts',(50.7298021581216,3.12950907248357,3.89027084869974));
#28117=CARTESIAN_POINT('Ctrl Pts',(50.7694384911199,2.42996705591471,4.36157017765919));
#28118=CARTESIAN_POINT('Ctrl Pts',(50.8090748241183,1.66034231950991,4.63713688051827));
#28119=CARTESIAN_POINT('Ctrl Pts',(50.8487111571166,0.890717583105111,4.91270358337736));
#28120=CARTESIAN_POINT('Ctrl Pts',(50.8883474901149,0.051010126864362,4.99253766013608));
#28121=CARTESIAN_POINT('Ctrl Pts',(50.9279838231132,-0.756754856649776,
4.86693919837959));
#28122=CARTESIAN_POINT('Ctrl Pts',(50.9676201561115,-1.56451984016391,4.74134073662311));
#28123=CARTESIAN_POINT('Ctrl Pts',(51.0072564891099,-2.34034235095145,4.41030973635142));
#28124=CARTESIAN_POINT('Ctrl Pts',(51.0468928221082,-2.98995927551403,3.91406675844198));
#28125=CARTESIAN_POINT('Ctrl Pts',(51.0865291551065,-3.63957620007659,3.41782378053256));
#28126=CARTESIAN_POINT('Ctrl Pts',(51.1261654881048,-4.16298753841419,2.75636882498538));
#28127=CARTESIAN_POINT('Ctrl Pts',(51.1658018211031,-4.49659835128688,2.01006924011891));
#28128=CARTESIAN_POINT('Ctrl Pts',(51.1992540387675,-4.77815874507751,1.38020834564911));
#28129=CARTESIAN_POINT('Ctrl Pts',(51.232706256432,-4.92452424115612,0.689912629125271));
#28130=CARTESIAN_POINT('Ctrl Pts',(51.2661584740964,-4.92519062564324,-0.000109311139069327));
#28131=CARTESIAN_POINT('Origin',(27.2271873309261,0.,0.));
#28132=CARTESIAN_POINT('',(51.9771873309261,-4.07061595521377,-9.62900340455034E-5));
#28133=CARTESIAN_POINT('',(52.2728126690739,-4.07017027259505,4.41422946496905E-5));
#28134=CARTESIAN_POINT('',(27.2271873309261,-4.0705,-3.42898509504556E-13));
#28135=CARTESIAN_POINT('',(52.575,3.27123862564629,-2.42269060785926));
#28136=CARTESIAN_POINT('Ctrl Pts',(51.9771873309261,-4.07061595521377,-9.62900340453765E-5));
#28137=CARTESIAN_POINT('Ctrl Pts',(51.9841798253067,-4.07073557068603,-0.119309531040752));
#28138=CARTESIAN_POINT('Ctrl Pts',(52.0308086526856,-4.03650707267767,-0.914204069448567));
#28139=CARTESIAN_POINT('Ctrl Pts',(52.1170738130629,-3.53493171453767,-2.34618303073278));
#28140=CARTESIAN_POINT('Ctrl Pts',(52.2359828120577,-1.98456277868761,-3.74990797127371));
#28141=CARTESIAN_POINT('Ctrl Pts',(52.3548918110528,0.0480654662789952,
-4.24241179250651));
#28142=CARTESIAN_POINT('Ctrl Pts',(52.4678975403668,1.96866977915683,-3.73070679305914));
#28143=CARTESIAN_POINT('Ctrl Pts',(52.5412669366826,2.92852672977728,-2.88450285218581));
#28144=CARTESIAN_POINT('Ctrl Pts',(52.575,3.27123862564629,-2.42269060785926));
#28145=CARTESIAN_POINT('',(52.575,-1.2223317023727,-3.88263769354992));
#28146=CARTESIAN_POINT('Origin',(52.575,0.,0.));
#28147=CARTESIAN_POINT('Ctrl Pts',(52.2728126690739,-4.07017027259505,4.4142294649864E-5));
#28148=CARTESIAN_POINT('Ctrl Pts',(52.294269113386,-4.07009408388197,-0.365864931681719));
#28149=CARTESIAN_POINT('Ctrl Pts',(52.3553618906963,-3.93089510915561,-1.40778868062961));
#28150=CARTESIAN_POINT('Ctrl Pts',(52.456091001005,-3.05253321900086,-2.94673237789893));
#28151=CARTESIAN_POINT('Ctrl Pts',(52.5353636670017,-1.86695937376299,-3.67969605923878));
#28152=CARTESIAN_POINT('Ctrl Pts',(52.575,-1.2223317023727,-3.88263769354992));
#28153=CARTESIAN_POINT('Origin',(27.2271873309261,0.,0.));
#28154=CARTESIAN_POINT('',(50.4771873309261,-4.07054709154665,0.000102932729394074));
#28155=CARTESIAN_POINT('',(50.7728126690739,-4.07065755161032,-9.03453792341913E-5));
#28156=CARTESIAN_POINT('',(27.2271873309261,-4.0705,-3.42898509504556E-13));
#28157=CARTESIAN_POINT('Ctrl Pts',(50.4771873309261,-4.07054709154665,0.000102932729393948));
#28158=CARTESIAN_POINT('Ctrl Pts',(50.5085438293269,-4.06999742249853,-0.53451196831054));
#28159=CARTESIAN_POINT('Ctrl Pts',(50.5795366607259,-3.83021781331726,-1.74538787286129));
#28160=CARTESIAN_POINT('Ctrl Pts',(50.6901658251233,-2.66338977453238,-3.3025248835498));
#28161=CARTESIAN_POINT('Ctrl Pts',(50.8090748241182,-0.762024273055086,
-4.17368358857445));
#28162=CARTESIAN_POINT('Ctrl Pts',(50.9279838231132,1.32451446418683,-4.03062986950608));
#28163=CARTESIAN_POINT('Ctrl Pts',(51.0468928221082,3.08919386154722,-2.90812602092978));
#28164=CARTESIAN_POINT('Ctrl Pts',(51.1658018211032,4.10319374310485,-1.07894246521889));
#28165=CARTESIAN_POINT('Ctrl Pts',(51.2847108200981,4.12011033911056,1.01242602683551));
#28166=CARTESIAN_POINT('Ctrl Pts',(51.4036198190931,3.13583292948141,2.85777316760714));
#28167=CARTESIAN_POINT('Ctrl Pts',(51.522528818088,1.38954256537078,4.00867652393499));
#28168=CARTESIAN_POINT('Ctrl Pts',(51.641437817083,-0.694408965276457,4.18546425093048));
#28169=CARTESIAN_POINT('Ctrl Pts',(51.760346816078,-2.60961812434468,3.34517724353594));
#28170=CARTESIAN_POINT('Ctrl Pts',(51.8722633206923,-3.81535137102011,1.78922094636592));
#28171=CARTESIAN_POINT('Ctrl Pts',(51.9445434923084,-4.07005754101129,0.556440131551016));
#28172=CARTESIAN_POINT('Ctrl Pts',(51.9771873309261,-4.07061595521377,-9.62900340453765E-5));
#28173=CARTESIAN_POINT('Ctrl Pts',(50.7728126690739,-4.07065755161032,-9.03453792342607E-5));
#28174=CARTESIAN_POINT('Ctrl Pts',(50.7789967844078,-4.07075936832261,-0.105518617986562));
#28175=CARTESIAN_POINT('Ctrl Pts',(50.82481723274,-4.04102179465801,-0.886619249492749));
#28176=CARTESIAN_POINT('Ctrl Pts',(50.9102740140706,-3.55858319850174,-2.31015180666798));
#28177=CARTESIAN_POINT('Ctrl Pts',(51.0291830130655,-2.02255111411372,-3.72955803196629));
#28178=CARTESIAN_POINT('Ctrl Pts',(51.1480920120605,0.00496435909204525,
-4.24267489657216));
#28179=CARTESIAN_POINT('Ctrl Pts',(51.2670010110554,2.03127363780405,-3.72481476796509));
#28180=CARTESIAN_POINT('Ctrl Pts',(51.3859100100504,3.56397955602096,-2.30181723828556));
#28181=CARTESIAN_POINT('Ctrl Pts',(51.5048190090453,4.23063280642202,-0.3194758487847));
#28182=CARTESIAN_POINT('Ctrl Pts',(51.6237280080403,3.86923365048362,1.74050225085362));
#28183=CARTESIAN_POINT('Ctrl Pts',(51.7426370070353,2.56760636844359,3.37752823139821));
#28184=CARTESIAN_POINT('Ctrl Pts',(51.8615460060302,0.642041384412004,4.19382294217941));
#28185=CARTESIAN_POINT('Ctrl Pts',(51.9804550050252,-1.43953109567099,3.99098337113032));
#28186=CARTESIAN_POINT('Ctrl Pts',(52.0993640040201,-3.17131432296482,2.81838363574518));
#28187=CARTESIAN_POINT('Ctrl Pts',(52.196816558703,-3.95899732867403,1.29599053439507));
#28188=CARTESIAN_POINT('Ctrl Pts',(52.2546327803876,-4.07023482673565,0.310076230437316));
#28189=CARTESIAN_POINT('Ctrl Pts',(52.2728126690739,-4.07017027259505,4.4142294649864E-5));
#28190=CARTESIAN_POINT('Origin',(27.2271873309261,0.,0.));
#28191=CARTESIAN_POINT('',(48.9771873309261,-4.07020325257277,-5.60749305029008E-5));
#28192=CARTESIAN_POINT('',(49.2728126690739,-4.07050358506006,0.000104730133326306));
#28193=CARTESIAN_POINT('',(27.2271873309261,-4.0705,-3.42898509504556E-13));
#28194=CARTESIAN_POINT('Ctrl Pts',(48.9771873309261,-4.07020325257276,-5.60749305029626E-5));
#28195=CARTESIAN_POINT('Ctrl Pts',(48.9932715003487,-4.07033712457477,-0.274350810682044));
#28196=CARTESIAN_POINT('Ctrl Pts',(49.0489920027697,-3.9756937275254,-1.22450088620951));
#28197=CARTESIAN_POINT('Ctrl Pts',(49.1443488381888,-3.24442007311038,-2.73387162926461));
#28198=CARTESIAN_POINT('Ctrl Pts',(49.2632578371838,-1.54412953702292,-3.95170591883982));
#28199=CARTESIAN_POINT('Ctrl Pts',(49.3821668361787,0.531387183013984,-4.209268743835));
#28200=CARTESIAN_POINT('Ctrl Pts',(49.5010758351737,2.47777588619694,-3.44397188633769));
#28201=CARTESIAN_POINT('Ctrl Pts',(49.6199848341686,3.82206070614344,-1.84178382408138));
#28202=CARTESIAN_POINT('Ctrl Pts',(49.7388938331636,4.23757807543132,0.207960935586202));
#28203=CARTESIAN_POINT('Ctrl Pts',(49.8578028321586,3.62335654502556,2.20717082341209));
#28204=CARTESIAN_POINT('Ctrl Pts',(49.9767118311535,2.12865302339433,3.6700343325455));
#28205=CARTESIAN_POINT('Ctrl Pts',(50.0956208301485,0.11668308609495,4.24107306629136));
#28206=CARTESIAN_POINT('Ctrl Pts',(50.2145298291435,-1.92364104561195,3.78152361138994));
#28207=CARTESIAN_POINT('Ctrl Pts',(50.3334388281384,-3.49651703165463,2.40305729100861));
#28208=CARTESIAN_POINT('Ctrl Pts',(50.4209913287327,-4.02901994529592,0.95813548887407));
#28209=CARTESIAN_POINT('Ctrl Pts',(50.4689074963286,-4.07069223430921,0.141270575156956));
#28210=CARTESIAN_POINT('Ctrl Pts',(50.4771873309261,-4.07054709154665,0.000102932729393948));
#28211=CARTESIAN_POINT('Ctrl Pts',(49.2728126690739,-4.07050358506006,0.000104730133326219));
#28212=CARTESIAN_POINT('Ctrl Pts',(49.3033607884279,-4.06997062985216,-0.520743688797961));
#28213=CARTESIAN_POINT('Ctrl Pts',(49.3735452407803,-3.83934011354282,-1.71785383211517));
#28214=CARTESIAN_POINT('Ctrl Pts',(49.483366026131,-2.69680012382729,-3.27529920754662));
#28215=CARTESIAN_POINT('Ctrl Pts',(49.6022750251259,-0.804382137054723,
-4.16572744962391));
#28216=CARTESIAN_POINT('Ctrl Pts',(49.7211840241209,1.28350211887322,-4.04387661996188));
#28217=CARTESIAN_POINT('Ctrl Pts',(49.8400930231158,3.05949311031172,-2.93935668390779));
#28218=CARTESIAN_POINT('Ctrl Pts',(49.9590020221109,4.09202191338058,-1.12056792152273));
#28219=CARTESIAN_POINT('Ctrl Pts',(50.0779110211058,4.13018221941277,0.970520809410563));
#28220=CARTESIAN_POINT('Ctrl Pts',(50.1968200201008,3.16470100669801,2.82577128347271));
#28221=CARTESIAN_POINT('Ctrl Pts',(50.3157290190956,1.43019190307756,3.99435438105406));
#28222=CARTESIAN_POINT('Ctrl Pts',(50.4346380180907,-0.651856340959766,
4.1923023665036));
#28223=CARTESIAN_POINT('Ctrl Pts',(50.5535470170856,-2.57550234917945,3.37151352187054));
#28224=CARTESIAN_POINT('Ctrl Pts',(50.6662719007468,-3.8058022184373,1.81673645511013));
#28225=CARTESIAN_POINT('Ctrl Pts',(50.7393604514094,-4.07010678652308,0.570211036924561));
#28226=CARTESIAN_POINT('Ctrl Pts',(50.7728126690739,-4.07065755161032,-9.03453792342607E-5));
#28227=CARTESIAN_POINT('Origin',(27.2271873309261,0.,0.));
#28228=CARTESIAN_POINT('',(47.4771873309261,-4.0708438118707,-1.45670437023455E-5));
#28229=CARTESIAN_POINT('',(47.7728126690739,-4.07022605737327,-6.65076761975636E-5));
#28230=CARTESIAN_POINT('',(27.2271873309261,-4.0705,-3.42898509504556E-13));
#28231=CARTESIAN_POINT('Ctrl Pts',(47.4771873309261,-4.0708438118707,-1.4567043702333E-5));
#28232=CARTESIAN_POINT('Ctrl Pts',(47.4779991713705,-4.0708466276555,-0.0138531808457906));
#28233=CARTESIAN_POINT('Ctrl Pts',(47.5184473448133,-4.06740414240983,-0.703330421609799));
#28234=CARTESIAN_POINT('Ctrl Pts',(47.5985318512543,-3.70631686362458,-2.06483195502968));
#28235=CARTESIAN_POINT('Ctrl Pts',(47.7174408502492,-2.2695351249873,-3.58462355241781));
#28236=CARTESIAN_POINT('Ctrl Pts',(47.8363498492442,-0.281252373079731,
-4.23334534366577));
#28237=CARTESIAN_POINT('Ctrl Pts',(47.9552588482392,1.77537519844767,-3.85335679646156));
#28238=CARTESIAN_POINT('Ctrl Pts',(48.0741678472341,3.40058348498636,-2.53699579379582));
#28239=CARTESIAN_POINT('Ctrl Pts',(48.1930768462292,4.19944402434456,-0.604140366551068));
#28240=CARTESIAN_POINT('Ctrl Pts',(48.311985845224,3.97783230526572,1.47552222866482));
#28241=CARTESIAN_POINT('Ctrl Pts',(48.4308948442191,2.78960036391312,3.19663033611261));
#28242=CARTESIAN_POINT('Ctrl Pts',(48.549803843214,0.923490644693623,4.14095166903249));
#28243=CARTESIAN_POINT('Ctrl Pts',(48.6687128422089,-1.16702891982273,4.07901448837793));
#28244=CARTESIAN_POINT('Ctrl Pts',(48.787621841204,-2.97395841132729,3.02586963760755));
#28245=CARTESIAN_POINT('Ctrl Pts',(48.8904466707762,-3.91154991106107,1.4793451741346));
#28246=CARTESIAN_POINT('Ctrl Pts',(48.9536351673504,-4.07000722284897,0.401595655703711));
#28247=CARTESIAN_POINT('Ctrl Pts',(48.9771873309261,-4.07020325257276,-5.60749305029626E-5));
#28248=CARTESIAN_POINT('Ctrl Pts',(47.7728126690739,-4.07022605737327,-6.6507676197633E-5));
#28249=CARTESIAN_POINT('Ctrl Pts',(47.7880884594498,-4.07037794775498,-0.260571206839678));
#28250=CARTESIAN_POINT('Ctrl Pts',(47.843000582824,-3.98185834718379,-1.19690962418239));
#28251=CARTESIAN_POINT('Ctrl Pts',(47.9375490391964,-3.27202394254474,-2.70077306086147));
#28252=CARTESIAN_POINT('Ctrl Pts',(48.0564580381915,-1.58419215321593,-3.93581643735453));
#28253=CARTESIAN_POINT('Ctrl Pts',(48.1753670371864,0.48860110601671,-4.21444952111902));
#28254=CARTESIAN_POINT('Ctrl Pts',(48.2942760361814,2.44266344009801,-3.46896398442958));
#28255=CARTESIAN_POINT('Ctrl Pts',(48.4131850351763,3.80315427688869,-1.88051411934194));
#28256=CARTESIAN_POINT('Ctrl Pts',(48.5320940341713,4.23947195846584,0.164903972792664));
#28257=CARTESIAN_POINT('Ctrl Pts',(48.6510030331663,3.6455905234561,2.17025011050524));
#28258=CARTESIAN_POINT('Ctrl Pts',(48.7699120321612,2.16582420148474,3.64822166748742));
#28259=CARTESIAN_POINT('Ctrl Pts',(48.8888210311562,0.159758802432322,4.23966896489628));
#28260=CARTESIAN_POINT('Ctrl Pts',(49.0077300301511,-1.88512826562663,3.80086927281119));
#28261=CARTESIAN_POINT('Ctrl Pts',(49.1266390291461,-3.47192586100346,2.43845168550668));
#28262=CARTESIAN_POINT('Ctrl Pts',(49.214999908787,-4.02413103778621,0.985723268098756));
#28263=CARTESIAN_POINT('Ctrl Pts',(49.2637244554296,-4.07066214181886,0.155059660506298));
#28264=CARTESIAN_POINT('Ctrl Pts',(49.2728126690739,-4.07050358506006,0.000104730133326219));
#28265=CARTESIAN_POINT('Origin',(27.2271873309261,0.,0.));
#28266=CARTESIAN_POINT('',(45.9771873309261,-4.07025298643191,7.60445319761115E-5));
#28267=CARTESIAN_POINT('',(46.2728126690739,-4.07084821056548,-6.23604212610479E-8));
#28268=CARTESIAN_POINT('',(27.2271873309261,-4.0705,-3.42898509504556E-13));
#28269=CARTESIAN_POINT('Ctrl Pts',(45.9771873309261,-4.07025298643191,7.60445319760578E-5));
#28270=CARTESIAN_POINT('Ctrl Pts',(46.0023631753907,-4.06996423923268,-0.429250442864527));
#28271=CARTESIAN_POINT('Ctrl Pts',(46.0671753528536,-3.89585401982529,-1.53472846738843));
#28272=CARTESIAN_POINT('Ctrl Pts',(46.1716238633148,-2.91160450045647,-3.085915573865));
#28273=CARTESIAN_POINT('Ctrl Pts',(46.2905328623097,-1.08356448049494,-4.10197558655686));
#28274=CARTESIAN_POINT('Ctrl Pts',(46.4094418613047,1.00778360743057,-4.12124834203113));
#28275=CARTESIAN_POINT('Ctrl Pts',(46.5283508602997,2.85423851237071,-3.13905052692677));
#28276=CARTESIAN_POINT('Ctrl Pts',(46.6472598592946,4.00710845607509,-1.39405793184905));
#28277=CARTESIAN_POINT('Ctrl Pts',(46.7661688582896,4.18624402154559,0.689693184085104));
#28278=CARTESIAN_POINT('Ctrl Pts',(46.8850778572845,3.34811495239536,2.60584764743572));
#28279=CARTESIAN_POINT('Ctrl Pts',(47.0039868562795,1.6963880814478,3.88877656509363));
#28280=CARTESIAN_POINT('Ctrl Pts',(47.1228958552745,-0.367564066613851,
4.22672596143089));
#28281=CARTESIAN_POINT('Ctrl Pts',(47.2418048542694,-2.34219750224519,3.5375735408011));
#28282=CARTESIAN_POINT('Ctrl Pts',(47.3599020128199,-3.73807708372676,1.99935876618999));
#28283=CARTESIAN_POINT('Ctrl Pts',(47.4383628383722,-4.07070915312478,0.661786852459511));
#28284=CARTESIAN_POINT('Ctrl Pts',(47.4771873309261,-4.0708438118707,-1.4567043702333E-5));
#28285=CARTESIAN_POINT('Ctrl Pts',(46.2728126690739,-4.07084821052679,-6.2360414317037E-8));
#28286=CARTESIAN_POINT('Ctrl Pts',(46.2728161304716,-4.07084821058119,-5.90650821111205E-5));
#28287=CARTESIAN_POINT('Ctrl Pts',(46.3124559248676,-4.07083382666307,-0.675755980011897));
#28288=CARTESIAN_POINT('Ctrl Pts',(46.391732052262,-3.72710065291479,-2.02707585696816));
#28289=CARTESIAN_POINT('Ctrl Pts',(46.5106410512569,-2.30583141340579,-3.56138418312489));
#28290=CARTESIAN_POINT('Ctrl Pts',(46.6295500502519,-0.324241098922964,
-4.23026991061211));
#28291=CARTESIAN_POINT('Ctrl Pts',(46.7484590492469,1.73614037090757,-3.87119263526966));
#28292=CARTESIAN_POINT('Ctrl Pts',(46.8673680482418,3.37463668760993,-2.57140876437375));
#28293=CARTESIAN_POINT('Ctrl Pts',(46.9862770472368,4.1930903743722,-0.646768056731501));
#28294=CARTESIAN_POINT('Ctrl Pts',(47.1051860462317,3.99261575077701,1.43503842231084));
#28295=CARTESIAN_POINT('Ctrl Pts',(47.2240950452267,2.82192850173731,3.16812804948658));
#28296=CARTESIAN_POINT('Ctrl Pts',(47.3430040442217,0.965507680676692,4.13135700774157));
#28297=CARTESIAN_POINT('Ctrl Pts',(47.4619130432167,-1.12553319906949,4.0906589719327));
#28298=CARTESIAN_POINT('Ctrl Pts',(47.5808220422116,-2.943067538678,3.05592363609448));
#28299=CARTESIAN_POINT('Ctrl Pts',(47.6844552508307,-3.9038147944966,1.50692039589771));
#28300=CARTESIAN_POINT('Ctrl Pts',(47.7484521264515,-4.06998383539806,0.415364423959208));
#28301=CARTESIAN_POINT('Ctrl Pts',(47.7728126690739,-4.07022605737327,-6.6507676197633E-5));
#28302=CARTESIAN_POINT('Origin',(27.2271873309261,0.,0.));
#28303=CARTESIAN_POINT('',(44.4771873309261,-4.07046018544014,-0.000104814225191196));
#28304=CARTESIAN_POINT('',(44.7728126690739,-4.07022626980563,6.65930553608862E-5));
#28305=CARTESIAN_POINT('',(27.2271873309261,-4.0705,-3.42898509504556E-13));
#28306=CARTESIAN_POINT('Ctrl Pts',(44.4771873309261,-4.07046018544014,-0.000104814225191444));
#28307=CARTESIAN_POINT('Ctrl Pts',(44.4870908464125,-4.07062964953048,-0.168965898301323));
#28308=CARTESIAN_POINT('Ctrl Pts',(44.5366306948972,-4.01905312111591,-1.01354822912588));
#28309=CARTESIAN_POINT('Ctrl Pts',(44.6258068763802,-3.44676119221666,-2.47389429282434));
#28310=CARTESIAN_POINT('Ctrl Pts',(44.7447158753752,-1.84608863354493,-3.819983306226));
#28311=CARTESIAN_POINT('Ctrl Pts',(44.8636248743702,0.203186698440704,-4.23780967691975));
#28312=CARTESIAN_POINT('Ctrl Pts',(44.9825338733652,2.20308730674562,-3.62584087029532));
#28313=CARTESIAN_POINT('Ctrl Pts',(45.1014428723601,3.66763383799168,-2.13278637607099));
#28314=CARTESIAN_POINT('Ctrl Pts',(45.2203518713551,4.24093891825145,-0.12146105473511));
#28315=CARTESIAN_POINT('Ctrl Pts',(45.33926087035,3.78368840810334,1.91937951603509));
#28316=CARTESIAN_POINT('Ctrl Pts',(45.458169869345,2.40699498298607,3.49380750011858));
#28317=CARTESIAN_POINT('Ctrl Pts',(45.5770788683399,0.445397558168305,4.21923413800868));
#28318=CARTESIAN_POINT('Ctrl Pts',(45.6959878673349,-1.62443225394642,3.91937948512372));
#28319=CARTESIAN_POINT('Ctrl Pts',(45.8148968663298,-3.29952218115088,2.66710874772735));
#28320=CARTESIAN_POINT('Ctrl Pts',(45.9086300208603,-3.98792413853412,1.16908185563358));
#28321=CARTESIAN_POINT('Ctrl Pts',(45.9627268423924,-4.07041883689898,0.246672370505476));
#28322=CARTESIAN_POINT('Ctrl Pts',(45.9771873309261,-4.07025298643191,7.60445319760578E-5));
#28323=CARTESIAN_POINT('Ctrl Pts',(44.7728126690739,-4.07022626980563,6.65930553610944E-5));
#28324=CARTESIAN_POINT('Ctrl Pts',(44.7971801344918,-4.0699836514846,-0.415482333917985));
#28325=CARTESIAN_POINT('Ctrl Pts',(44.861183932908,-3.90374787388921,-1.50715653101103));
#28326=CARTESIAN_POINT('Ctrl Pts',(44.9648240643225,-2.94280167925739,-3.05617965494951));
#28327=CARTESIAN_POINT('Ctrl Pts',(45.0837330633174,-1.12517733033491,-4.09075687156072));
#28328=CARTESIAN_POINT('Ctrl Pts',(45.2026420623124,0.965867082001261,-4.13127299833094));
#28329=CARTESIAN_POINT('Ctrl Pts',(45.3215510613073,2.82220410049894,-3.16788254548659));
#28330=CARTESIAN_POINT('Ctrl Pts',(45.4404600603023,3.99274057599417,-1.43469108161613));
#28331=CARTESIAN_POINT('Ctrl Pts',(45.5593690592973,4.193034093298,0.647132829719501));
#28332=CARTESIAN_POINT('Ctrl Pts',(45.6782780582922,3.37441297664422,2.57170232918147));
#28333=CARTESIAN_POINT('Ctrl Pts',(45.7971870572872,1.73580359220705,3.87134365513335));
#28334=CARTESIAN_POINT('Ctrl Pts',(45.9160960562822,-0.324609107543747,
4.23024168744071));
#28335=CARTESIAN_POINT('Ctrl Pts',(46.0350050552771,-2.306141225207,3.56118357519822));
#28336=CARTESIAN_POINT('Ctrl Pts',(46.1539105928744,-3.72723561434065,2.02679627912053));
#28337=CARTESIAN_POINT('Ctrl Pts',(46.2331797974733,-4.07084758770274,0.675578847152629));
#28338=CARTESIAN_POINT('Ctrl Pts',(46.2728126690739,-4.07084821052679,-6.2360414317037E-8));
#28339=CARTESIAN_POINT('Origin',(27.2271873309261,0.,0.));
#28340=CARTESIAN_POINT('',(42.9771873309261,-4.07069838669775,9.14325826918604E-5));
#28341=CARTESIAN_POINT('',(43.2728126690739,-4.07050321383809,-0.0001047408713159));
#28342=CARTESIAN_POINT('',(27.2271873309261,-4.0705,-3.42898509504556E-13));
#28343=CARTESIAN_POINT('Ctrl Pts',(42.9771873309261,-4.07069838669775,9.14325826918867E-5));
#28344=CARTESIAN_POINT('Ctrl Pts',(43.0114548504327,-4.07016735320138,-0.584091151150294));
#28345=CARTESIAN_POINT('Ctrl Pts',(43.0853587029375,-3.79600152359016,-1.84449226855255));
#28346=CARTESIAN_POINT('Ctrl Pts',(43.1988988884408,-2.54082596366002,-3.39771592193865));
#28347=CARTESIAN_POINT('Ctrl Pts',(43.3178078874356,-0.608870803793044,
-4.19876433520088));
#28348=CARTESIAN_POINT('Ctrl Pts',(43.4367168864306,1.47103965821834,-3.97949031283073));
#28349=CARTESIAN_POINT('Ctrl Pts',(43.5556258854256,3.19348559196464,-2.79320086151097));
#28350=CARTESIAN_POINT('Ctrl Pts',(43.6745348844206,4.13990858508463,-0.928154848713153));
#28351=CARTESIAN_POINT('Ctrl Pts',(43.7934438834155,4.08032670854032,1.16243248575246));
#28352=CARTESIAN_POINT('Ctrl Pts',(43.9123528824105,3.0292182035071,2.97054765803357));
#28353=CARTESIAN_POINT('Ctrl Pts',(44.0312618814054,1.2420044090019,4.05681405687331));
#28354=CARTESIAN_POINT('Ctrl Pts',(44.1501708804004,-0.847018655558019,
4.15726777299333));
#28355=CARTESIAN_POINT('Ctrl Pts',(44.2690798793954,-2.73021469130703,3.24749801153628));
#28356=CARTESIAN_POINT('Ctrl Pts',(44.378085362904,-3.84837513323758,1.6900775035994));
#28357=CARTESIAN_POINT('Ctrl Pts',(44.4474545134142,-4.06995141207779,0.506858173271681));
#28358=CARTESIAN_POINT('Ctrl Pts',(44.4771873309261,-4.07046018544014,-0.000104814225191444));
#28359=CARTESIAN_POINT('Ctrl Pts',(43.2728126690739,-4.07050321383809,-0.000104740871315935));
#28360=CARTESIAN_POINT('Ctrl Pts',(43.2819078055136,-4.0706618730839,-0.155177721611787));
#28361=CARTESIAN_POINT('Ctrl Pts',(43.3306392749516,-4.0240885331959,-0.985959389093055));
#28362=CARTESIAN_POINT('Ctrl Pts',(43.419007077388,-3.47171372465588,-2.43875382803693));
#28363=CARTESIAN_POINT('Ctrl Pts',(43.5379160763829,-1.88479759986051,-3.80103319712063));
#28364=CARTESIAN_POINT('Ctrl Pts',(43.6568250753779,0.160127627215037,-4.23965507926387));
#28365=CARTESIAN_POINT('Ctrl Pts',(43.7757340743728,2.16614156925702,-3.64803322477728));
#28366=CARTESIAN_POINT('Ctrl Pts',(43.8946430733678,3.64577930876166,-2.16993296345209));
#28367=CARTESIAN_POINT('Ctrl Pts',(44.0135520723628,4.23948628841551,-0.1645351582025));
#28368=CARTESIAN_POINT('Ctrl Pts',(44.1324610713577,3.80299066814145,1.88084496359989));
#28369=CARTESIAN_POINT('Ctrl Pts',(44.2513700703527,2.44236165043659,3.46917647027723));
#28370=CARTESIAN_POINT('Ctrl Pts',(44.3702790693477,0.488234470571936,4.21449201028578));
#28371=CARTESIAN_POINT('Ctrl Pts',(44.4891880683426,-1.58453454124508,3.93567860682148));
#28372=CARTESIAN_POINT('Ctrl Pts',(44.6080970673376,-3.27225888233889,2.70048840272595));
#28373=CARTESIAN_POINT('Ctrl Pts',(44.7026386009147,-3.98191049238861,1.19667333697073));
#28374=CARTESIAN_POINT('Ctrl Pts',(44.7575438014934,-4.07037829657382,0.260453195861538));
#28375=CARTESIAN_POINT('Ctrl Pts',(44.7728126690739,-4.07022626980563,6.65930553610944E-5));
#28376=CARTESIAN_POINT('Origin',(27.2271873309261,0.,0.));
#28377=CARTESIAN_POINT('',(41.4771873309261,-4.06894895743657,0.00540651071496451));
#28378=CARTESIAN_POINT('',(41.7728126690739,-4.07070027400187,-0.000480811481659155));
#28379=CARTESIAN_POINT('',(27.2271873309261,-4.0705,-3.42898509504556E-13));
#28380=CARTESIAN_POINT('Ctrl Pts',(41.4771873309261,-4.06894895743657,0.00540651071496485));
#28381=CARTESIAN_POINT('Ctrl Pts',(41.5358188544528,-4.05939870704616,-0.995808554814875));
#28382=CARTESIAN_POINT('Ctrl Pts',(41.6737230439761,-3.1827766265387,-3.36894097376134));
#28383=CARTESIAN_POINT('Ctrl Pts',(41.8512635664978,0.0468156998159277,
-4.48442240866564));
#28384=CARTESIAN_POINT('Ctrl Pts',(42.0098088984911,2.60148746873208,-3.34400839089152));
#28385=CARTESIAN_POINT('Ctrl Pts',(42.1287178974861,3.88717983168713,-1.70435364109129));
#28386=CARTESIAN_POINT('Ctrl Pts',(42.247626896481,4.22697668061874,0.364604063255797));
#28387=CARTESIAN_POINT('Ctrl Pts',(42.366535895476,3.54029074951913,2.33730671702443));
#28388=CARTESIAN_POINT('Ctrl Pts',(42.485444894471,1.99296498656723,3.7458830298263));
#28389=CARTESIAN_POINT('Ctrl Pts',(42.6043538934659,-0.0384826524084342,
4.24227598834855));
#28390=CARTESIAN_POINT('Ctrl Pts',(42.7232628924609,-2.06066523781936,3.70875467629474));
#28391=CARTESIAN_POINT('Ctrl Pts',(42.8421718914558,-3.58205929234741,2.27351505986046));
#28392=CARTESIAN_POINT('Ctrl Pts',(42.9268133709443,-4.04543031358348,0.858803213014503));
#28393=CARTESIAN_POINT('Ctrl Pts',(42.9718185174344,-4.07078158559399,0.0916173843402187));
#28394=CARTESIAN_POINT('Ctrl Pts',(42.9771873309261,-4.07069838669775,9.14325826918867E-5));
#28395=CARTESIAN_POINT('Ctrl Pts',(41.7728126690739,-4.07070027400187,-0.000480811481659068));
#28396=CARTESIAN_POINT('Ctrl Pts',(41.8062718095338,-4.07015469889988,-0.57096407947981));
#28397=CARTESIAN_POINT('Ctrl Pts',(41.8793672829919,-3.80565769019447,-1.81613961322352));
#28398=CARTESIAN_POINT('Ctrl Pts',(41.9920990894484,-2.5752427483792,-3.37219006842077));
#28399=CARTESIAN_POINT('Ctrl Pts',(42.1110080884434,-0.651474736920205,
-4.19213227664958));
#28400=CARTESIAN_POINT('Ctrl Pts',(42.2299170874383,1.43053091718906,-3.99434360254506));
#28401=CARTESIAN_POINT('Ctrl Pts',(42.3488260864333,3.16495106439444,-2.82543900138727));
#28402=CARTESIAN_POINT('Ctrl Pts',(42.4677350854282,4.13026450704979,-0.970190049367721));
#28403=CARTESIAN_POINT('Ctrl Pts',(42.5866440844232,4.09192548053664,1.12093820678962));
#28404=CARTESIAN_POINT('Ctrl Pts',(42.7055530834182,3.05923685698906,2.9396156616928));
#28405=CARTESIAN_POINT('Ctrl Pts',(42.8244620824131,1.28315058703404,4.04399185547656));
#28406=CARTESIAN_POINT('Ctrl Pts',(42.9433710814081,-0.804744663182227,
4.16565565627073));
#28407=CARTESIAN_POINT('Ctrl Pts',(43.0622800804031,-2.69708497911968,3.27506549112629));
#28408=CARTESIAN_POINT('Ctrl Pts',(43.1720939429583,-3.83941755468911,1.71761765906299));
#28409=CARTESIAN_POINT('Ctrl Pts',(43.2422714725153,-4.06997044082866,0.520625697547703));
#28410=CARTESIAN_POINT('Ctrl Pts',(43.2728126690739,-4.07050321383809,-0.000104740871315935));
#28411=CARTESIAN_POINT('Origin',(27.2271873309261,0.,0.));
#28412=CARTESIAN_POINT('',(39.9771873309261,-4.07077050609724,-5.79609919884648E-5));
#28413=CARTESIAN_POINT('',(40.2728126690739,-4.07025619321701,0.000377108328969283));
#28414=CARTESIAN_POINT('',(27.2271873309261,-4.0705,-3.42898509504556E-13));
#28415=CARTESIAN_POINT('Ctrl Pts',(39.9771873309261,-4.07077050609724,-5.79609919882859E-5));
#28416=CARTESIAN_POINT('Ctrl Pts',(39.9809101924763,-4.07081705151356,-0.0635213177095936));
#28417=CARTESIAN_POINT('Ctrl Pts',(40.0242693870248,-4.05388725332644,-0.802638439329735));
#28418=CARTESIAN_POINT('Ctrl Pts',(40.1072649145718,-3.62830971000893,-2.19902759642159));
#28419=CARTESIAN_POINT('Ctrl Pts',(40.2261739135667,-2.13693872948098,-3.66517562577142));
#28420=CARTESIAN_POINT('Ctrl Pts',(40.3450829125617,-0.126195570511627,
-4.24090522757565));
#28421=CARTESIAN_POINT('Ctrl Pts',(40.4639919115566,1.91502918549748,-3.78563729041068));
#28422=CARTESIAN_POINT('Ctrl Pts',(40.5829009105516,3.49126579952493,-2.41135070611703));
#28423=CARTESIAN_POINT('Ctrl Pts',(40.7018099095465,4.21838606955971,-0.449310859787289));
#28424=CARTESIAN_POINT('Ctrl Pts',(40.8207189085415,3.92189238888511,1.61834114804089));
#28425=CARTESIAN_POINT('Ctrl Pts',(40.9396279075364,2.66945837179664,3.2998455083566));
#28426=CARTESIAN_POINT('Ctrl Pts',(41.0585369065315,0.774140435187547,4.16543344142367));
#28427=CARTESIAN_POINT('Ctrl Pts',(41.2170822385247,-2.01888746148146,4.0045386084997));
#28428=CARTESIAN_POINT('Ctrl Pts',(41.3566323799896,-3.87071962072282,2.05940168604075));
#28429=CARTESIAN_POINT('Ctrl Pts',(41.4565461884562,-4.07231110917807,0.357882816421777));
#28430=CARTESIAN_POINT('Ctrl Pts',(41.4771873309261,-4.06894895743657,0.00540651071496485));
#28431=CARTESIAN_POINT('Ctrl Pts',(40.2728126690739,-4.07025619321701,0.000377108328969492));
#28432=CARTESIAN_POINT('Ctrl Pts',(40.2909994805556,-4.07036169565849,-0.309620800904844));
#28433=CARTESIAN_POINT('Ctrl Pts',(40.3488226250356,-3.95913913945033,-1.29545413833272));
#28434=CARTESIAN_POINT('Ctrl Pts',(40.4462821025139,-3.17025406296392,-2.82213573711675));
#28435=CARTESIAN_POINT('Ctrl Pts',(40.5651911015089,-1.44080558796838,-3.98425201455624));
#28436=CARTESIAN_POINT('Ctrl Pts',(40.7237364335021,1.3412377851549,-4.2793985106552));
#28437=CARTESIAN_POINT('Ctrl Pts',(40.9219180984939,4.38508550900277,-1.98115657932714));
#28438=CARTESIAN_POINT('Ctrl Pts',(41.1597360964836,4.03738561363306,2.61791400162535));
#28439=CARTESIAN_POINT('Ctrl Pts',(41.3579177614753,0.682606151108172,4.43240558295318));
#28440=CARTESIAN_POINT('Ctrl Pts',(41.5164630934686,-2.02344151873906,3.72234728068988));
#28441=CARTESIAN_POINT('Ctrl Pts',(41.6353720924636,-3.55851387613991,2.31342601692174));
#28442=CARTESIAN_POINT('Ctrl Pts',(41.7208219509987,-4.04108037252554,0.88609737447698));
#28443=CARTESIAN_POINT('Ctrl Pts',(41.7666354765354,-4.07080099752324,0.104841230207512));
#28444=CARTESIAN_POINT('Ctrl Pts',(41.7728126690739,-4.07070027400187,-0.000480811481659068));
#28445=CARTESIAN_POINT('Origin',(27.2271873309261,0.,0.));
#28446=CARTESIAN_POINT('',(38.4771873309261,-4.07037658145865,9.98552888675809E-5));
#28447=CARTESIAN_POINT('',(38.7728126690739,-4.07079742697958,-5.00540521497506E-5));
#28448=CARTESIAN_POINT('',(27.2271873309261,-4.0705,-3.42898509504556E-13));
#28449=CARTESIAN_POINT('Ctrl Pts',(38.4771873309261,-4.07037658145865,9.98552888676826E-5));
#28450=CARTESIAN_POINT('Ctrl Pts',(38.5052741964965,-4.06993440527969,-0.478826890908034));
#28451=CARTESIAN_POINT('Ctrl Pts',(38.5729973950651,-3.86611251597914,-1.63398402620179));
#28452=CARTESIAN_POINT('Ctrl Pts',(38.6803569266322,-2.79679599758437,-3.19033663920374));
#28453=CARTESIAN_POINT('Ctrl Pts',(38.7992659256271,-0.932818789330533,
-4.13886031436587));
#28454=CARTESIAN_POINT('Ctrl Pts',(38.9181749246222,1.15783504299492,-4.081633735705));
#28455=CARTESIAN_POINT('Ctrl Pts',(39.037083923617,2.96713288406074,-3.03256289173867));
#28456=CARTESIAN_POINT('Ctrl Pts',(39.1559929226121,4.05541232630964,-1.24657417618181));
#28457=CARTESIAN_POINT('Ctrl Pts',(39.274901921607,4.15821928046345,0.8423347006637));
#28458=CARTESIAN_POINT('Ctrl Pts',(39.393810920602,3.25057202966842,2.72655386816114));
#28459=CARTESIAN_POINT('Ctrl Pts',(39.5127199195969,1.55302934330574,3.94821746331971));
#28460=CARTESIAN_POINT('Ctrl Pts',(39.631628918592,-0.521900729557193,4.21045371123498));
#28461=CARTESIAN_POINT('Ctrl Pts',(39.7505379175868,-2.47001093446444,3.44954947520581));
#28462=CARTESIAN_POINT('Ctrl Pts',(39.8657240550316,-3.77569799789881,1.90045186147924));
#28463=CARTESIAN_POINT('Ctrl Pts',(39.941273859478,-4.0703214946426,0.612156438801636));
#28464=CARTESIAN_POINT('Ctrl Pts',(39.9771873309261,-4.07077050609724,-5.79609919882859E-5));
#28465=CARTESIAN_POINT('Ctrl Pts',(38.7728126690739,-4.07079742697958,-5.00540521495944E-5));
#28466=CARTESIAN_POINT('Ctrl Pts',(38.7757271515774,-4.07082806252421,-0.049731900772906));
#28467=CARTESIAN_POINT('Ctrl Pts',(38.8182779670792,-4.05782430804937,-0.77506006973181));
#28468=CARTESIAN_POINT('Ctrl Pts',(38.9004651155794,-3.65047142573015,-2.16202983439362));
#28469=CARTESIAN_POINT('Ctrl Pts',(39.0193741145744,-2.17403875473271,-3.64333320582671));
#28470=CARTESIAN_POINT('Ctrl Pts',(39.1382831135694,-0.169311715692027,
-4.23929647022592));
#28471=CARTESIAN_POINT('Ctrl Pts',(39.2571921125643,1.87656008277306,-3.80511074896768));
#28472=CARTESIAN_POINT('Ctrl Pts',(39.3761011115593,3.46642106848062,-2.4462615072031));
#28473=CARTESIAN_POINT('Ctrl Pts',(39.4950101105543,4.21394248995934,-0.49299624037214));
#28474=CARTESIAN_POINT('Ctrl Pts',(39.6139191095491,3.93745486993259,1.58012745604));
#28475=CARTESIAN_POINT('Ctrl Pts',(39.7328281085442,2.7041860128382,3.26915872948103));
#28476=CARTESIAN_POINT('Ctrl Pts',(39.8517371075391,0.813740946052253,4.1640155130528));
#28477=CARTESIAN_POINT('Ctrl Pts',(39.9706461065341,-1.27433631150534,4.04653670722897));
#28478=CARTESIAN_POINT('Ctrl Pts',(40.089555105529,-3.05296367944959,2.94668522964312));
#28479=CARTESIAN_POINT('Ctrl Pts',(40.1902772930423,-3.93078192295446,1.40692776914096));
#28480=CARTESIAN_POINT('Ctrl Pts',(40.2513631475573,-4.0701317636604,0.365988575238109));
#28481=CARTESIAN_POINT('Ctrl Pts',(40.2728126690739,-4.07025619321701,0.000377108328969492));
#28482=CARTESIAN_POINT('Origin',(27.2271873309261,0.,0.));
#28483=CARTESIAN_POINT('',(36.9771873309261,-4.07031820724409,-9.1677525538646E-5));
#28484=CARTESIAN_POINT('',(37.2728126690739,-4.07033856695489,9.50420139643471E-5));
#28485=CARTESIAN_POINT('',(27.2271873309261,-4.0705,-3.42898509504556E-13));
#28486=CARTESIAN_POINT('Ctrl Pts',(36.9771873309261,-4.07031820724409,-9.16775255385346E-5));
#28487=CARTESIAN_POINT('Ctrl Pts',(36.9900018675183,-4.07049942327998,-0.218609364111448));
#28488=CARTESIAN_POINT('Ctrl Pts',(37.0424527371088,-3.99970858733677,-1.112902578135));
#28489=CARTESIAN_POINT('Ctrl Pts',(37.1345399396977,-3.35397800645881,-2.59829698616001));
#28490=CARTESIAN_POINT('Ctrl Pts',(37.2534489386926,-1.70514605210925,-3.88494435443889));
#28491=CARTESIAN_POINT('Ctrl Pts',(37.3723579376876,0.358039381572612,-4.22754343529587));
#28492=CARTESIAN_POINT('Ctrl Pts',(37.4912669366826,2.3342206179893,-3.54284205161814));
#28493=CARTESIAN_POINT('Ctrl Pts',(37.6101759356776,3.74318215294784,-1.99722383969792));
#28494=CARTESIAN_POINT('Ctrl Pts',(37.7290849346725,4.24254386394922,0.0337232658201172));
#28495=CARTESIAN_POINT('Ctrl Pts',(37.8479939336675,3.71095997990038,2.05647555874971));
#28496=CARTESIAN_POINT('Ctrl Pts',(37.9669029326624,2.27760631649146,3.57950068621502));
#28497=CARTESIAN_POINT('Ctrl Pts',(38.0858119316574,0.290790325944755,4.23270087345946));
#28498=CARTESIAN_POINT('Ctrl Pts',(38.2047209306524,-1.76668822311588,3.85734732873792));
#28499=CARTESIAN_POINT('Ctrl Pts',(38.3236299296473,-3.39485843815668,2.54465162401958));
#28500=CARTESIAN_POINT('Ctrl Pts',(38.4144520630719,-4.00834925103214,1.06972433652504));
#28501=CARTESIAN_POINT('Ctrl Pts',(38.4656378634982,-4.07055840663824,0.197037062173665));
#28502=CARTESIAN_POINT('Ctrl Pts',(38.4771873309261,-4.07037658145865,9.98552888676826E-5));
#28503=CARTESIAN_POINT('Ctrl Pts',(37.2728126690739,-4.07033856695489,9.50420139643297E-5));
#28504=CARTESIAN_POINT('Ctrl Pts',(37.3000911555976,-4.06993567621103,-0.465060000392124));
#28505=CARTESIAN_POINT('Ctrl Pts',(37.3670059751196,-3.87457929834536,-1.60642688649147));
#28506=CARTESIAN_POINT('Ctrl Pts',(37.4735571276399,-2.82905983413317,-3.16176157564063));
#28507=CARTESIAN_POINT('Ctrl Pts',(37.5924661266349,-0.974814094226818,
-4.12917101732149));
#28508=CARTESIAN_POINT('Ctrl Pts',(37.7113751256298,1.11631317895359,-4.09318466350003));
#28509=CARTESIAN_POINT('Ctrl Pts',(37.8302841246248,2.93617439347552,-3.06254726405115));
#28510=CARTESIAN_POINT('Ctrl Pts',(37.9491931236197,4.04254008318163,-1.28770550784711));
#28511=CARTESIAN_POINT('Ctrl Pts',(38.0681021226147,4.16656144887969,0.800050936289306));
#28512=CARTESIAN_POINT('Ctrl Pts',(38.1870111216096,3.27810107619118,2.69339361556102));
#28513=CARTESIAN_POINT('Ctrl Pts',(38.3059201206047,1.593056403167,3.93223689564486));
#28514=CARTESIAN_POINT('Ctrl Pts',(38.4248291195996,-0.479103781660292,
4.21553977736235));
#28515=CARTESIAN_POINT('Ctrl Pts',(38.5437381185946,-2.43484088061553,3.47445898581872));
#28516=CARTESIAN_POINT('Ctrl Pts',(38.659732635086,-3.76547389787559,1.92793678161055));
#28517=CARTESIAN_POINT('Ctrl Pts',(38.7360908185791,-4.07041142572947,0.625930491508946));
#28518=CARTESIAN_POINT('Ctrl Pts',(38.7728126690739,-4.07079742697958,-5.00540521495944E-5));
#28519=CARTESIAN_POINT('Origin',(27.2271873309261,0.,0.));
#28520=CARTESIAN_POINT('',(35.4771873309261,-4.07081121953653,4.27420412099477E-5));
#28521=CARTESIAN_POINT('',(35.7728126690739,-4.07035481323816,-9.73195012207717E-5));
#28522=CARTESIAN_POINT('',(27.2271873309261,-4.0705,-3.42898509504556E-13));
#28523=CARTESIAN_POINT('Ctrl Pts',(35.4771873309261,-4.07081121953653,4.27420412098516E-5));
#28524=CARTESIAN_POINT('Ctrl Pts',(35.5143658715385,-4.07046879867817,-0.633716582260352));
#28525=CARTESIAN_POINT('Ctrl Pts',(35.5911807451492,-3.75962139193843,-1.94345586451205));
#28526=CARTESIAN_POINT('Ctrl Pts',(35.7076319517581,-2.41486119677437,-3.48837513699617));
#28527=CARTESIAN_POINT('Ctrl Pts',(35.8265409507531,-0.454903298757822,
-4.21821984785987));
#28528=CARTESIAN_POINT('Ctrl Pts',(35.9454499497481,1.61559689818276,-3.92302974226322));
#28529=CARTESIAN_POINT('Ctrl Pts',(36.064358948743,3.29350421714833,-2.6745365332569));
#28530=CARTESIAN_POINT('Ctrl Pts',(36.183267947738,4.17108423869985,-0.776126258909775));
#28531=CARTESIAN_POINT('Ctrl Pts',(36.3021769467329,4.03508347943329,1.31088405669769));
#28532=CARTESIAN_POINT('Ctrl Pts',(36.4210859457279,2.91855036222394,3.07934724889256));
#28533=CARTESIAN_POINT('Ctrl Pts',(36.5399949447229,1.09280439154274,4.09952366232033));
#28534=CARTESIAN_POINT('Ctrl Pts',(36.6589039437179,-0.998494961682174,
4.12350864041721));
#28535=CARTESIAN_POINT('Ctrl Pts',(36.7778129427128,-2.84715828911907,3.14547379146596));
#28536=CARTESIAN_POINT('Ctrl Pts',(36.8839074051156,-3.87929173201797,1.59085652731975));
#28537=CARTESIAN_POINT('Ctrl Pts',(36.95036553452,-4.06993890834513,0.457282403743256));
#28538=CARTESIAN_POINT('Ctrl Pts',(36.9771873309261,-4.07031820724409,-9.16775255385346E-5));
#28539=CARTESIAN_POINT('Ctrl Pts',(35.7728126690739,-4.07035481323816,-9.73195012204595E-5));
#28540=CARTESIAN_POINT('Ctrl Pts',(35.7848188266194,-4.07053749389208,-0.204824981186366));
#28541=CARTESIAN_POINT('Ctrl Pts',(35.8364613171632,-4.0052715983505,-1.0853115636913));
#28542=CARTESIAN_POINT('Ctrl Pts',(35.9277401407054,-3.38019902696682,-2.56409249929749));
#28543=CARTESIAN_POINT('Ctrl Pts',(36.0466491397003,-1.74452218259612,-3.86742267683414));
#28544=CARTESIAN_POINT('Ctrl Pts',(36.1655581386953,0.315076609834192,-4.23096236532504));
#28545=CARTESIAN_POINT('Ctrl Pts',(36.2844671376903,2.29811123382828,-3.56637078327709));
#28546=CARTESIAN_POINT('Ctrl Pts',(36.4033761366852,3.72270080001742,-2.03514484998292));
#28547=CARTESIAN_POINT('Ctrl Pts',(36.5222851356802,4.24266754688635,-0.0093751510681078));
#28548=CARTESIAN_POINT('Ctrl Pts',(36.6411941346751,3.73165864358157,2.01867272598657));
#28549=CARTESIAN_POINT('Ctrl Pts',(36.7601031336701,2.31385014926909,3.55617959242768));
#28550=CARTESIAN_POINT('Ctrl Pts',(36.8790121326651,0.333772013114966,4.22952858485353));
#28551=CARTESIAN_POINT('Ctrl Pts',(36.99792113166,-1.72741330724408,3.87509471792328));
#28552=CARTESIAN_POINT('Ctrl Pts',(37.116830130655,-3.36883416623464,2.57900604248567));
#28553=CARTESIAN_POINT('Ctrl Pts',(37.2084606431263,-4.00286951946101,1.097315110437));
#28554=CARTESIAN_POINT('Ctrl Pts',(37.2604548225993,-4.07052108668355,0.210822077620177));
#28555=CARTESIAN_POINT('Ctrl Pts',(37.2728126690739,-4.07033856695489,9.50420139643297E-5));
#28556=CARTESIAN_POINT('Origin',(27.2271873309261,0.,0.));
#28557=CARTESIAN_POINT('',(33.9771873309261,-4.07016987886937,3.24954791396568E-5));
#28558=CARTESIAN_POINT('',(34.2728126690739,-4.07078562779549,5.5347657024335E-5));
#28559=CARTESIAN_POINT('',(27.2271873309261,-4.0705,-3.42898509504556E-13));
#28560=CARTESIAN_POINT('Ctrl Pts',(33.9771873309261,-4.07016987886936,3.24954791397145E-5));
#28561=CARTESIAN_POINT('Ctrl Pts',(33.9990935425603,-4.07006529445769,-0.373558417633581));
#28562=CARTESIAN_POINT('Ctrl Pts',(34.0606360871928,-3.92681616665385,-1.42319026575441));
#28563=CARTESIAN_POINT('Ctrl Pts',(34.1618149648236,-3.03590382713174,-2.96371450185516));
#28564=CARTESIAN_POINT('Ctrl Pts',(34.2807239638186,-1.25114215390858,-4.05400530424081));
#28565=CARTESIAN_POINT('Ctrl Pts',(34.3996329628135,0.837649255637629,-4.15916571209051));
#28566=CARTESIAN_POINT('Ctrl Pts',(34.5185419618086,2.72289042788497,-3.25364156197822));
#28567=CARTESIAN_POINT('Ctrl Pts',(34.6374509608034,3.94646445364522,-1.55747680952698));
#28568=CARTESIAN_POINT('Ctrl Pts',(34.7563599597985,4.21104070005508,0.517157537486679));
#28569=CARTESIAN_POINT('Ctrl Pts',(34.8752689587934,3.45232667550434,2.46612169644987));
#28570=CARTESIAN_POINT('Ctrl Pts',(34.9941779577884,1.85469121778504,3.8158139607128));
#28571=CARTESIAN_POINT('Ctrl Pts',(35.1130869567833,-0.193637456642115,
4.23825674440386));
#28572=CARTESIAN_POINT('Ctrl Pts',(35.2319959557783,-2.19491188970968,3.63079571065499));
#28573=CARTESIAN_POINT('Ctrl Pts',(35.3509049547733,-3.66281888647431,2.14104495538666));
#28574=CARTESIAN_POINT('Ctrl Pts',(35.4326354131559,-4.05998619783484,0.759479670105897));
#28575=CARTESIAN_POINT('Ctrl Pts',(35.4747295385402,-4.07083385623406,0.041939191340904));
#28576=CARTESIAN_POINT('Ctrl Pts',(35.4771873309261,-4.07081121953653,4.27420412098516E-5));
#28577=CARTESIAN_POINT('Ctrl Pts',(34.2728126690739,-4.07078562779549,5.5347657024309E-5));
#28578=CARTESIAN_POINT('Ctrl Pts',(34.3091828306396,-4.07036990121448,-0.619935370476085));
#28579=CARTESIAN_POINT('Ctrl Pts',(34.3851893252035,-3.76994385597486,-1.91598331854555));
#28580=CARTESIAN_POINT('Ctrl Pts',(34.5008321527658,-2.45017227519968,-3.46366447981092));
#28581=CARTESIAN_POINT('Ctrl Pts',(34.6197411517608,-0.497729417387068,
-4.21338121156021));
#28582=CARTESIAN_POINT('Ctrl Pts',(34.7386501507558,1.57566256123941,-3.93923892395085));
#28583=CARTESIAN_POINT('Ctrl Pts',(34.8575591497507,3.26616577576251,-2.70785467337129));
#28584=CARTESIAN_POINT('Ctrl Pts',(34.9764681487457,4.16298498204543,-0.818456991005179));
#28585=CARTESIAN_POINT('Ctrl Pts',(35.0953771477406,4.04819154107314,1.26982717471511));
#28586=CARTESIAN_POINT('Ctrl Pts',(35.2142861467356,2.94968046020461,3.04954111130644));
#28587=CARTESIAN_POINT('Ctrl Pts',(35.3331951457306,1.13439185749204,4.0882112128065));
#28588=CARTESIAN_POINT('Ctrl Pts',(35.4521041447256,-0.956555954881787,
4.13343882403517));
#28589=CARTESIAN_POINT('Ctrl Pts',(35.5710131437205,-2.81505899362824,3.17423355619177));
#28590=CARTESIAN_POINT('Ctrl Pts',(35.67791598517,-3.87091551080481,1.61841633854707));
#28591=CARTESIAN_POINT('Ctrl Pts',(35.7451824936211,-4.06993440408556,0.47104935594091));
#28592=CARTESIAN_POINT('Ctrl Pts',(35.7728126690739,-4.07035481323816,-9.73195012204595E-5));
#28593=CARTESIAN_POINT('Origin',(27.2271873309261,0.,0.));
#28594=CARTESIAN_POINT('',(32.4771873309261,-4.07063452722895,-9.39916808427117E-5));
#28595=CARTESIAN_POINT('',(32.7728126690739,-4.07016025367539,2.0115106517532E-5));
#28596=CARTESIAN_POINT('',(27.2271873309261,-4.0705,-3.42898509504556E-13));
#28597=CARTESIAN_POINT('Ctrl Pts',(32.4771873309261,-4.07063452722895,-9.399168084262E-5));
#28598=CARTESIAN_POINT('Ctrl Pts',(32.4838212135822,-4.07074636705293,-0.113191851009958));
#28599=CARTESIAN_POINT('Ctrl Pts',(32.5300914292365,-4.03852757013727,-0.901966866821061));
#28600=CARTESIAN_POINT('Ctrl Pts',(32.6159979778891,-3.54546956353323,-2.33022772913439));
#28601=CARTESIAN_POINT('Ctrl Pts',(32.7349069768841,-2.00143968510732,-3.74092968169653));
#28602=CARTESIAN_POINT('Ctrl Pts',(32.8538159758791,0.0289435448015357,
-4.24257916450323));
#28603=CARTESIAN_POINT('Ctrl Pts',(32.972724974874,2.05229344259103,-3.71327447432861));
#28604=CARTESIAN_POINT('Ctrl Pts',(33.091633973869,3.57693243670117,-2.28163757843869));
#28605=CARTESIAN_POINT('Ctrl Pts',(33.2105429728639,4.23237057927023,-0.295558751907219));
#28606=CARTESIAN_POINT('Ctrl Pts',(33.3294519718589,3.85933525284402,1.76234136938946));
#28607=CARTESIAN_POINT('Ctrl Pts',(33.4483609708539,2.54847469557654,3.39198944899592));
#28608=CARTESIAN_POINT('Ctrl Pts',(33.5672699698489,0.618330320477916,4.19737814723441));
#28609=CARTESIAN_POINT('Ctrl Pts',(33.6861789688438,-1.46206940626736,3.98279659879273));
#28610=CARTESIAN_POINT('Ctrl Pts',(33.8050879678388,-3.18718370466638,2.80038849605003));
#28611=CARTESIAN_POINT('Ctrl Pts',(33.9020907551995,-3.96267663186491,1.280678352677));
#28612=CARTESIAN_POINT('Ctrl Pts',(33.959457209562,-4.07025452583356,0.302403911433452));
#28613=CARTESIAN_POINT('Ctrl Pts',(33.9771873309261,-4.07016987886936,3.24954791397145E-5));
#28614=CARTESIAN_POINT('Ctrl Pts',(32.7728126690739,-4.07016025367539,2.01151065172891E-5));
#28615=CARTESIAN_POINT('Ctrl Pts',(32.7939105016614,-4.07009808342627,-0.359787052605734));
#28616=CARTESIAN_POINT('Ctrl Pts',(32.8546446672472,-3.93407800546665,-1.3956072406382));
#28617=CARTESIAN_POINT('Ctrl Pts',(32.9550151658314,-3.06585324807998,-2.93272222825354));
#28618=CARTESIAN_POINT('Ctrl Pts',(33.0739241648263,-1.29225906543464,-4.04108677395906));
#28619=CARTESIAN_POINT('Ctrl Pts',(33.1928331638213,0.795356335102055,-4.16746015062799));
#28620=CARTESIAN_POINT('Ctrl Pts',(33.3117421628162,2.68969875215823,-3.2811334062333));
#28621=CARTESIAN_POINT('Ctrl Pts',(33.4306511618112,3.93043965810529,-1.59748549315922));
#28622=CARTESIAN_POINT('Ctrl Pts',(33.5495601608062,4.21607683810534,0.47435419472437));
#28623=CARTESIAN_POINT('Ctrl Pts',(33.6684691598011,3.47719995677159,2.43092498187187));
#28624=CARTESIAN_POINT('Ctrl Pts',(33.7873781587961,1.89335739132502,3.79677673765208));
#28625=CARTESIAN_POINT('Ctrl Pts',(33.906287157791,-0.15057433877126,4.24000509143145));
#28626=CARTESIAN_POINT('Ctrl Pts',(34.025196156786,-2.1579162406289,3.65290477637881));
#28627=CARTESIAN_POINT('Ctrl Pts',(34.144105155781,-3.64088071375389,2.17814219808442));
#28628=CARTESIAN_POINT('Ctrl Pts',(34.2266439932103,-4.05612867944369,0.787058536401716));
#28629=CARTESIAN_POINT('Ctrl Pts',(34.2695464976412,-4.07082296153899,0.0557327459666281));
#28630=CARTESIAN_POINT('Ctrl Pts',(34.2728126690739,-4.07078562779549,5.5347657024309E-5));
#28631=CARTESIAN_POINT('Origin',(27.2271873309261,0.,0.));
#28632=CARTESIAN_POINT('',(30.9771873309261,-4.07052775430868,0.00010449998854035));
#28633=CARTESIAN_POINT('',(31.2728126690739,-4.07067546468071,-8.7070929181976E-5));
#28634=CARTESIAN_POINT('',(27.2271873309261,-4.0705,-3.42898509504556E-13));
#28635=CARTESIAN_POINT('Ctrl Pts',(30.9771873309261,-4.07052775430868,0.000104499988540334));
#28636=CARTESIAN_POINT('Ctrl Pts',(31.0081852176023,-4.06998453340041,-0.528403485036771));
#28637=CARTESIAN_POINT('Ctrl Pts',(31.0788194372768,-3.83428484306565,-1.73317487116484));
#28638=CARTESIAN_POINT('Ctrl Pts',(31.1890899899496,-2.67824532838493,-3.29048852198293));
#28639=CARTESIAN_POINT('Ctrl Pts',(31.3079989889446,-0.780824962758849,
-4.1702074196749));
#28640=CARTESIAN_POINT('Ctrl Pts',(31.4269079879395,1.30633725444068,-4.03655766520605));
#28641=CARTESIAN_POINT('Ctrl Pts',(31.5458169869345,3.07605722060134,-2.92201779428377));
#28642=CARTESIAN_POINT('Ctrl Pts',(31.6647259859295,4.09828989491981,-1.09742224157957));
#28643=CARTESIAN_POINT('Ctrl Pts',(31.7836349849244,4.12463093940056,0.993848720882264));
#28644=CARTESIAN_POINT('Ctrl Pts',(31.9025439839194,3.14867943729,2.84361276159299));
#28645=CARTESIAN_POINT('Ctrl Pts',(32.0214529829143,1.40759331257097,4.00237388736178));
#28646=CARTESIAN_POINT('Ctrl Pts',(32.1403619819093,-0.675540453973202,
4.18855115831721));
#28647=CARTESIAN_POINT('Ctrl Pts',(32.2592709809043,-2.59451670629275,3.35690314889015));
#28648=CARTESIAN_POINT('Ctrl Pts',(32.3715460972432,-3.81113575126776,1.80142850182054));
#28649=CARTESIAN_POINT('Ctrl Pts',(32.4441848805838,-4.07007814291696,0.562548834528985));
#28650=CARTESIAN_POINT('Ctrl Pts',(32.4771873309261,-4.07063452722895,-9.399168084262E-5));
#28651=CARTESIAN_POINT('Ctrl Pts',(31.2728126690739,-4.07067546468071,-8.70709291818372E-5));
#28652=CARTESIAN_POINT('Ctrl Pts',(31.2786381726832,-4.07076914227082,-0.0994003818986817));
#28653=CARTESIAN_POINT('Ctrl Pts',(31.3241000092909,-4.04297868156283,-0.874382434154477));
#28654=CARTESIAN_POINT('Ctrl Pts',(31.4091981788968,-3.56895760027616,-2.29409186709539));
#28655=CARTESIAN_POINT('Ctrl Pts',(31.5281071778918,-2.03933759614693,-3.72040561602178));
#28656=CARTESIAN_POINT('Ctrl Pts',(31.6470161768868,-0.0141549844227289,
-4.24265429393642));
#28657=CARTESIAN_POINT('Ctrl Pts',(31.7659251758817,2.01446731467499,-3.73393053486277));
#28658=CARTESIAN_POINT('Ctrl Pts',(31.8848341748767,3.55357052479912,-2.31785511487955));
#28659=CARTESIAN_POINT('Ctrl Pts',(32.0037431738717,4.229149869261,-0.338536837555411));
#28660=CARTESIAN_POINT('Ctrl Pts',(32.1226521728666,3.87703838273484,1.72304648374135));
#28661=CARTESIAN_POINT('Ctrl Pts',(32.2415611718616,2.58279977386025,3.36592648990226));
#28662=CARTESIAN_POINT('Ctrl Pts',(32.3604701708566,0.660936292926016,4.19088045920181));
#28663=CARTESIAN_POINT('Ctrl Pts',(32.4793791698515,-1.42153586561542,3.99744313151944));
#28664=CARTESIAN_POINT('Ctrl Pts',(32.5982881688465,-3.15857231724438,2.83262011635301));
#28665=CARTESIAN_POINT('Ctrl Pts',(32.6960993352539,-3.95605371558114,1.30826770260012));
#28666=CARTESIAN_POINT('Ctrl Pts',(32.7542741686631,-4.07021488218683,0.316179857998792));
#28667=CARTESIAN_POINT('Ctrl Pts',(32.7728126690739,-4.07016025367539,2.01151065172891E-5));
#28668=CARTESIAN_POINT('Origin',(52.575,4.52129938221115E-16,0.));
#28669=CARTESIAN_POINT('',(52.575,0.695807839646318,4.87560011181052));
#28670=CARTESIAN_POINT('Ctrl Pts',(52.575,3.27123862564629,-2.42269060785926));
#28671=CARTESIAN_POINT('Ctrl Pts',(52.575,3.33974877356658,-2.34761008169236));
#28672=CARTESIAN_POINT('Ctrl Pts',(52.575,3.40533191462526,-2.27003568459554));
#28673=CARTESIAN_POINT('Ctrl Pts',(52.575,3.46783701755502,-2.1901289314666));
#28674=CARTESIAN_POINT('Ctrl Pts',(52.575,3.54519071433771,-2.09123968142613));
#28675=CARTESIAN_POINT('Ctrl Pts',(52.575,3.61783176379727,-1.98877942727981));
#28676=CARTESIAN_POINT('Ctrl Pts',(52.575,3.68567005490555,-1.88315349412949));
#28677=CARTESIAN_POINT('Ctrl Pts',(52.575,3.72452565888664,-1.82265433706683));
#28678=CARTESIAN_POINT('Ctrl Pts',(52.575,3.76180508901478,-1.76111582740147));
#28679=CARTESIAN_POINT('Ctrl Pts',(52.575,3.79748635683124,-1.69860843369842));
#28680=CARTESIAN_POINT('Ctrl Pts',(52.575,3.81574454298833,-1.66662325771487));
#28681=CARTESIAN_POINT('Ctrl Pts',(52.575,3.83358420466306,-1.63438432888875));
#28682=CARTESIAN_POINT('Ctrl Pts',(52.575,3.85100198255905,-1.60190073374641));
#28683=CARTESIAN_POINT('Ctrl Pts',(52.575,3.86219017839908,-1.58103510862413));
#28684=CARTESIAN_POINT('Ctrl Pts',(52.575,3.87320429706676,-1.5600685282487));
#28685=CARTESIAN_POINT('Ctrl Pts',(52.575,3.88404338396807,-1.53900335395738));
#28686=CARTESIAN_POINT('Ctrl Pts',(52.575,3.89350384310779,-1.52061746753831));
#28687=CARTESIAN_POINT('Ctrl Pts',(52.575,3.90282655955187,-1.50216502101326));
#28688=CARTESIAN_POINT('Ctrl Pts',(52.575,3.91201088413724,-1.48364851325173));
#28689=CARTESIAN_POINT('Ctrl Pts',(52.575,3.96947384655046,-1.36779749125935));
#28690=CARTESIAN_POINT('Ctrl Pts',(52.575,4.02152670830412,-1.24943340089431));
#28691=CARTESIAN_POINT('Ctrl Pts',(52.575,4.06807408099195,-1.12898158468846));
#28692=CARTESIAN_POINT('Ctrl Pts',(52.575,4.11491086544974,-1.00778085030938));
#28693=CARTESIAN_POINT('Ctrl Pts',(52.575,4.15617394543224,-0.884465663289738));
#28694=CARTESIAN_POINT('Ctrl Pts',(52.575,4.1917261494215,-0.759434877005129));
#28695=CARTESIAN_POINT('Ctrl Pts',(52.575,4.20419944906554,-0.715568497791931));
#28696=CARTESIAN_POINT('Ctrl Pts',(52.575,4.21596939517056,-0.671490682417999));
#28697=CARTESIAN_POINT('Ctrl Pts',(52.575,4.22702874369151,-0.627217904445778));
#28698=CARTESIAN_POINT('Ctrl Pts',(52.575,4.23745334703906,-0.585486138005798));
#28699=CARTESIAN_POINT('Ctrl Pts',(52.575,4.24724657653273,-0.543581140564887));
#28700=CARTESIAN_POINT('Ctrl Pts',(52.575,4.25640176372427,-0.501516465484337));
#28701=CARTESIAN_POINT('Ctrl Pts',(52.575,4.26067115082541,-0.481900221988142));
#28702=CARTESIAN_POINT('Ctrl Pts',(52.575,4.26479980625067,-0.462258226011452));
#28703=CARTESIAN_POINT('Ctrl Pts',(52.575,4.26878680612531,-0.442595043227594));
#28704=CARTESIAN_POINT('Ctrl Pts',(52.575,4.27969784077511,-0.388783737627976));
#28705=CARTESIAN_POINT('Ctrl Pts',(52.575,4.28954966295039,-0.334806492626263));
#28706=CARTESIAN_POINT('Ctrl Pts',(52.575,4.29833604406102,-0.280694309983832));
#28707=CARTESIAN_POINT('Ctrl Pts',(52.575,4.31910349396582,-0.152795004442932));
#28708=CARTESIAN_POINT('Ctrl Pts',(52.575,4.33392209061696,-0.0241436197492663));
#28709=CARTESIAN_POINT('Ctrl Pts',(52.575,4.3429370549885,0.104855326937507));
#28710=CARTESIAN_POINT('Ctrl Pts',(52.575,4.35209690964512,0.235927570133247));
#28711=CARTESIAN_POINT('Ctrl Pts',(52.575,4.35526523050226,0.367359322916083));
#28712=CARTESIAN_POINT('Ctrl Pts',(52.575,4.35254513857273,0.498747978701545));
#28713=CARTESIAN_POINT('Ctrl Pts',(52.575,4.35009453448373,0.617119557845933));
#28714=CARTESIAN_POINT('Ctrl Pts',(52.575,4.34286386932909,0.735456833565131));
#28715=CARTESIAN_POINT('Ctrl Pts',(52.575,4.33089381744145,0.853472901232893));
#28716=CARTESIAN_POINT('Ctrl Pts',(52.575,4.32191627852572,0.941984951983714));
#28717=CARTESIAN_POINT('Ctrl Pts',(52.575,4.3102721617027,1.03031650957211));
#28718=CARTESIAN_POINT('Ctrl Pts',(52.575,4.2959663745933,1.11834669639071));
#28719=CARTESIAN_POINT('Ctrl Pts',(52.575,4.29282287279567,1.13769013051244));
#28720=CARTESIAN_POINT('Ctrl Pts',(52.575,4.28955081429939,1.1570190093928));
#28721=CARTESIAN_POINT('Ctrl Pts',(52.575,4.28615018278361,1.17633204195954));
#28722=CARTESIAN_POINT('Ctrl Pts',(52.575,4.28275394386741,1.19562012786028));
#28723=CARTESIAN_POINT('Ctrl Pts',(52.575,4.27923064364971,1.21488549512907));
#28724=CARTESIAN_POINT('Ctrl Pts',(52.575,4.27558218993528,1.23411866256198));
#28725=CARTESIAN_POINT('Ctrl Pts',(52.575,4.25019479115831,1.36795072665851));
#28726=CARTESIAN_POINT('Ctrl Pts',(52.575,4.21873023527054,1.50034525531864));
#28727=CARTESIAN_POINT('Ctrl Pts',(52.575,4.18131895579719,1.63087576261264));
#28728=CARTESIAN_POINT('Ctrl Pts',(52.575,4.15599231403848,1.71924214417873));
#28729=CARTESIAN_POINT('Ctrl Pts',(52.575,4.12793922655871,1.80675465116126));
#28730=CARTESIAN_POINT('Ctrl Pts',(52.575,4.09718683849603,1.89328327569644));
#28731=CARTESIAN_POINT('Ctrl Pts',(52.575,4.05202655950391,2.02035167821686));
#28732=CARTESIAN_POINT('Ctrl Pts',(52.575,4.00104762032723,2.14529897660314));
#28733=CARTESIAN_POINT('Ctrl Pts',(52.575,3.94453562255273,2.26782055577994));
#28734=CARTESIAN_POINT('Ctrl Pts',(52.575,3.88754808400084,2.39137313738635));
#28735=CARTESIAN_POINT('Ctrl Pts',(52.575,3.82493370056318,2.51245971712919));
#28736=CARTESIAN_POINT('Ctrl Pts',(52.575,3.75693415592833,2.63075466736293));
#28737=CARTESIAN_POINT('Ctrl Pts',(52.575,3.73798363353152,2.66372181612655));
#28738=CARTESIAN_POINT('Ctrl Pts',(52.575,3.71861457831358,2.69647203588586));
#28739=CARTESIAN_POINT('Ctrl Pts',(52.575,3.69883156699335,2.72899797900061));
#28740=CARTESIAN_POINT('Ctrl Pts',(52.575,3.68688426888272,2.74864095106543));
#28741=CARTESIAN_POINT('Ctrl Pts',(52.575,3.67478598909839,2.76820212301373));
#28742=CARTESIAN_POINT('Ctrl Pts',(52.575,3.66253768792789,2.78767984802252));
#28743=CARTESIAN_POINT('Ctrl Pts',(52.575,3.65179462941252,2.80476387760371));
#28744=CARTESIAN_POINT('Ctrl Pts',(52.575,3.64093526729776,2.8217849699757));
#28745=CARTESIAN_POINT('Ctrl Pts',(52.575,3.62997063555571,2.83872625989296));
#28746=CARTESIAN_POINT('Ctrl Pts',(52.575,3.55452375466503,2.95529811680457));
#28747=CARTESIAN_POINT('Ctrl Pts',(52.575,3.47399253337476,3.06826057686335));
#28748=CARTESIAN_POINT('Ctrl Pts',(52.575,3.38870787807495,3.17730716262715));
#28749=CARTESIAN_POINT('Ctrl Pts',(52.575,3.30236451551238,3.28770743167573));
#28750=CARTESIAN_POINT('Ctrl Pts',(52.575,3.21114868347686,3.39409473557566));
#28751=CARTESIAN_POINT('Ctrl Pts',(52.575,3.11535179231217,3.49613809434228));
#28752=CARTESIAN_POINT('Ctrl Pts',(52.575,3.02057356161899,3.59709637054837));
#28753=CARTESIAN_POINT('Ctrl Pts',(52.575,2.92131071507327,3.69380325966571));
#28754=CARTESIAN_POINT('Ctrl Pts',(52.575,2.8178008233524,3.78591524603509));
#28755=CARTESIAN_POINT('Ctrl Pts',(52.575,2.74290684774614,3.85256233401386));
#28756=CARTESIAN_POINT('Ctrl Pts',(52.575,2.66578852360097,3.91680346413161));
#28757=CARTESIAN_POINT('Ctrl Pts',(52.575,2.58658179140831,3.97858032782616));
#28758=CARTESIAN_POINT('Ctrl Pts',(52.575,2.5515363020237,4.005913868308));
#28759=CARTESIAN_POINT('Ctrl Pts',(52.575,2.51608184050385,4.03276485581719));
#28760=CARTESIAN_POINT('Ctrl Pts',(52.575,2.48022960363516,4.05912758981513));
#28761=CARTESIAN_POINT('Ctrl Pts',(52.575,2.45986381027416,4.07410288954327));
#28762=CARTESIAN_POINT('Ctrl Pts',(52.575,2.43936965724024,4.08892063278838));
#28763=CARTESIAN_POINT('Ctrl Pts',(52.575,2.41874915138383,4.1035797134609));
#28764=CARTESIAN_POINT('Ctrl Pts',(52.575,2.40331173815407,4.11455414287045));
#28765=CARTESIAN_POINT('Ctrl Pts',(52.575,2.38780325084898,4.12543975453688));
#28766=CARTESIAN_POINT('Ctrl Pts',(52.575,2.3722370798148,4.13622757204182));
#28767=CARTESIAN_POINT('Ctrl Pts',(52.575,2.25664941820129,4.21633324456537));
#28768=CARTESIAN_POINT('Ctrl Pts',(52.575,2.13771895193274,4.29116786534254));
#28769=CARTESIAN_POINT('Ctrl Pts',(52.575,2.01587804671584,4.36063651988135));
#28770=CARTESIAN_POINT('Ctrl Pts',(52.575,1.89144332325272,4.43158406251083));
#28771=CARTESIAN_POINT('Ctrl Pts',(52.575,1.76397243333656,4.49693525545565));
#28772=CARTESIAN_POINT('Ctrl Pts',(52.575,1.63388301973716,4.55655608155356));
#28773=CARTESIAN_POINT('Ctrl Pts',(52.575,1.50331587990202,4.61639585269885));
#28774=CARTESIAN_POINT('Ctrl Pts',(52.575,1.37011029782627,4.67046354765956));
#28775=CARTESIAN_POINT('Ctrl Pts',(52.575,1.23465458866001,4.71858364092287));
#28776=CARTESIAN_POINT('Ctrl Pts',(52.575,1.10035291241915,4.76629376865323));
#28777=CARTESIAN_POINT('Ctrl Pts',(52.575,0.96383858689367,4.80815757818582));
#28778=CARTESIAN_POINT('Ctrl Pts',(52.575,0.825466953202148,4.84395867267966));
#28779=CARTESIAN_POINT('Ctrl Pts',(52.575,0.782423633175989,4.85509533361567));
#28780=CARTESIAN_POINT('Ctrl Pts',(52.575,0.739200462732767,4.86564498253008));
#28781=CARTESIAN_POINT('Ctrl Pts',(52.575,0.695807839646318,4.87560011181052));
#28782=CARTESIAN_POINT('',(52.575,-4.925,-6.03138548580072E-16));
#28783=CARTESIAN_POINT('Origin',(52.575,0.,0.));
#28784=CARTESIAN_POINT('',(52.575,-3.42883835300376,3.535500303812));
#28785=CARTESIAN_POINT('Origin',(52.575,0.,0.));
#28786=CARTESIAN_POINT('Ctrl Pts',(52.575,-3.42895049711685,3.53554284596622));
#28787=CARTESIAN_POINT('Ctrl Pts',(52.575,-3.5091582599996,3.4437018410653));
#28788=CARTESIAN_POINT('Ctrl Pts',(52.575,-3.58581516971697,3.34898223367365));
#28789=CARTESIAN_POINT('Ctrl Pts',(52.575,-3.65871286157694,3.25152488213287));
#28790=CARTESIAN_POINT('Ctrl Pts',(52.575,-3.74535381180812,3.13569408791887));
#28791=CARTESIAN_POINT('Ctrl Pts',(52.575,-3.82668584084521,3.01599591002262));
#28792=CARTESIAN_POINT('Ctrl Pts',(52.575,-3.90252529089327,2.89283180460372));
#28793=CARTESIAN_POINT('Ctrl Pts',(52.575,-3.94702892486057,2.82055741097349));
#28794=CARTESIAN_POINT('Ctrl Pts',(52.575,-3.98964028296665,2.74708912931587));
#28795=CARTESIAN_POINT('Ctrl Pts',(52.575,-4.0303141866431,2.67250587749233));
#28796=CARTESIAN_POINT('Ctrl Pts',(52.575,-4.05883144723199,2.62021411703734));
#28797=CARTESIAN_POINT('Ctrl Pts',(52.575,-4.0863961915163,2.56737424131341));
#28798=CARTESIAN_POINT('Ctrl Pts',(52.575,-4.11299101431309,2.51401324086522));
#28799=CARTESIAN_POINT('Ctrl Pts',(52.575,-4.12678190058593,2.48634261135178));
#28800=CARTESIAN_POINT('Ctrl Pts',(52.575,-4.14031387620493,2.4585275644258));
#28801=CARTESIAN_POINT('Ctrl Pts',(52.575,-4.15357199766806,2.43059856460847));
#28802=CARTESIAN_POINT('Ctrl Pts',(52.575,-4.21456648591084,2.30211014671852));
#28803=CARTESIAN_POINT('Ctrl Pts',(52.575,-4.26981904241137,2.17111458465814));
#28804=CARTESIAN_POINT('Ctrl Pts',(52.575,-4.31915508190971,2.03799843572494));
#28805=CARTESIAN_POINT('Ctrl Pts',(52.575,-4.36809647196592,1.90594711109564));
#28806=CARTESIAN_POINT('Ctrl Pts',(52.575,-4.41121576812792,1.77180823660554));
#28807=CARTESIAN_POINT('Ctrl Pts',(52.575,-4.44829212455411,1.63595212520647));
#28808=CARTESIAN_POINT('Ctrl Pts',(52.575,-4.47402001950507,1.54167932983406));
#28809=CARTESIAN_POINT('Ctrl Pts',(52.575,-4.49683707512701,1.44657950014077));
#28810=CARTESIAN_POINT('Ctrl Pts',(52.575,-4.51665446402512,1.35077720141337));
#28811=CARTESIAN_POINT('Ctrl Pts',(52.575,-4.520764031306,1.33091050785917));
#28812=CARTESIAN_POINT('Ctrl Pts',(52.575,-4.52474456023551,1.3110136125633));
#28813=CARTESIAN_POINT('Ctrl Pts',(52.575,-4.5285951898601,1.29108763838625));
#28814=CARTESIAN_POINT('Ctrl Pts',(52.575,-4.53235405480569,1.27163652177849));
#28815=CARTESIAN_POINT('Ctrl Pts',(52.575,-4.53598714894778,1.25216798572193));
#28816=CARTESIAN_POINT('Ctrl Pts',(52.575,-4.53949403976558,1.23268319329843));
#28817=CARTESIAN_POINT('Ctrl Pts',(52.575,-4.54971862223298,1.17587393479983));
#28818=CARTESIAN_POINT('Ctrl Pts',(52.575,-4.55887058507416,1.11892617810197));
#28819=CARTESIAN_POINT('Ctrl Pts',(52.575,-4.56693872807373,1.06186570389229));
#28820=CARTESIAN_POINT('Ctrl Pts',(52.575,-4.58634449454588,0.924621949367475));
#28821=CARTESIAN_POINT('Ctrl Pts',(52.575,-4.59948385775869,0.786726058412982));
#28822=CARTESIAN_POINT('Ctrl Pts',(52.575,-4.60642483762348,0.648594126037778));
#28823=CARTESIAN_POINT('Ctrl Pts',(52.575,-4.61338604128565,0.510059721350728));
#28824=CARTESIAN_POINT('Ctrl Pts',(52.575,-4.61411253459408,0.371287080057338));
#28825=CARTESIAN_POINT('Ctrl Pts',(52.575,-4.60862119457809,0.232702682255874));
#28826=CARTESIAN_POINT('Ctrl Pts',(52.575,-4.60321433808265,0.0962503865976968));
#28827=CARTESIAN_POINT('Ctrl Pts',(52.575,-4.59177921640993,-0.0400201269089059));
#28828=CARTESIAN_POINT('Ctrl Pts',(52.575,-4.57428532046287,-0.175683930093663));
#28829=CARTESIAN_POINT('Ctrl Pts',(52.575,-4.56307295245554,-0.262634972399285));
#28830=CARTESIAN_POINT('Ctrl Pts',(52.575,-4.54937076504609,-0.349336392803606));
#28831=CARTESIAN_POINT('Ctrl Pts',(52.575,-4.5331611772412,-0.435670341473325));
#28832=CARTESIAN_POINT('Ctrl Pts',(52.575,-4.52960784261755,-0.454595770836303));
#28833=CARTESIAN_POINT('Ctrl Pts',(52.575,-4.52593398997846,-0.473503520597655));
#28834=CARTESIAN_POINT('Ctrl Pts',(52.575,-4.52213938767235,-0.492392312214098));
#28835=CARTESIAN_POINT('Ctrl Pts',(52.575,-4.51862284016697,-0.509897001159094));
#28836=CARTESIAN_POINT('Ctrl Pts',(52.575,-4.51500456977891,-0.527375548556558));
#28837=CARTESIAN_POINT('Ctrl Pts',(52.575,-4.51128481062968,-0.544826628462621));
#28838=CARTESIAN_POINT('Ctrl Pts',(52.575,-4.48314127653678,-0.676860731368406));
#28839=CARTESIAN_POINT('Ctrl Pts',(52.575,-4.44919050457636,-0.807332152072528));
#28840=CARTESIAN_POINT('Ctrl Pts',(52.575,-4.40946716653323,-0.935850761402154));
#28841=CARTESIAN_POINT('Ctrl Pts',(52.575,-4.38257279429726,-1.02286327064312));
#28842=CARTESIAN_POINT('Ctrl Pts',(52.575,-4.35303131455946,-1.10898041176107));
#28843=CARTESIAN_POINT('Ctrl Pts',(52.575,-4.32084101271981,-1.19407570764782));
#28844=CARTESIAN_POINT('Ctrl Pts',(52.575,-4.27308791576523,-1.3203113650548));
#28845=CARTESIAN_POINT('Ctrl Pts',(52.575,-4.21950722517578,-1.44430002393767));
#28846=CARTESIAN_POINT('Ctrl Pts',(52.575,-4.16031888017239,-1.56567297532392));
#28847=CARTESIAN_POINT('Ctrl Pts',(52.575,-4.10160823636378,-1.68606634189684));
#28848=CARTESIAN_POINT('Ctrl Pts',(52.575,-4.0373795113942,-1.8038866280582));
#28849=CARTESIAN_POINT('Ctrl Pts',(52.575,-3.96781301876157,-1.91873624560477));
#28850=CARTESIAN_POINT('Ctrl Pts',(52.575,-3.94906135545505,-1.94969398513736));
#28851=CARTESIAN_POINT('Ctrl Pts',(52.575,-3.92992169701845,-1.98043564353625));
#28852=CARTESIAN_POINT('Ctrl Pts',(52.575,-3.91039722592405,-2.01095287666042));
#28853=CARTESIAN_POINT('Ctrl Pts',(52.575,-3.89784596496109,-2.0305708092004));
#28854=CARTESIAN_POINT('Ctrl Pts',(52.575,-3.88513567617724,-2.05009599225496));
#28855=CARTESIAN_POINT('Ctrl Pts',(52.575,-3.87226717680479,-2.06952615257306));
#28856=CARTESIAN_POINT('Ctrl Pts',(52.575,-3.86251730577991,-2.08424749277064));
#28857=CARTESIAN_POINT('Ctrl Pts',(52.575,-3.85267685250824,-2.09891382958667));
#28858=CARTESIAN_POINT('Ctrl Pts',(52.575,-3.84275385977172,-2.11351315437222));
#28859=CARTESIAN_POINT('Ctrl Pts',(52.575,-3.76865945781698,-2.22252545213873));
#28860=CARTESIAN_POINT('Ctrl Pts',(52.575,-3.68985952194509,-2.32796672350722));
#28861=CARTESIAN_POINT('Ctrl Pts',(52.575,-3.60658777099566,-2.42951413079451));
#28862=CARTESIAN_POINT('Ctrl Pts',(52.575,-3.52423547904387,-2.52994028536101));
#28863=CARTESIAN_POINT('Ctrl Pts',(52.575,-3.4375089805729,-2.6265585971069));
#28864=CARTESIAN_POINT('Ctrl Pts',(52.575,-3.34660031521949,-2.71901977384784));
#28865=CARTESIAN_POINT('Ctrl Pts',(52.575,-3.26049006165378,-2.80660059293913));
#28866=CARTESIAN_POINT('Ctrl Pts',(52.575,-3.17062685965888,-2.89045165857665));
#28867=CARTESIAN_POINT('Ctrl Pts',(52.575,-3.07715226412168,-2.97023878224582));
#28868=CARTESIAN_POINT('Ctrl Pts',(52.575,-3.011002341584,-3.02670238093684));
#28869=CARTESIAN_POINT('Ctrl Pts',(52.575,-2.94304325285011,-3.08112987045868));
#28870=CARTESIAN_POINT('Ctrl Pts',(52.575,-2.87337756767158,-3.13344755448078));
#28871=CARTESIAN_POINT('Ctrl Pts',(52.575,-2.83651936368417,-3.16112740669057));
#28872=CARTESIAN_POINT('Ctrl Pts',(52.575,-2.79918341581072,-3.18821652073932));
#28873=CARTESIAN_POINT('Ctrl Pts',(52.575,-2.76138474990579,-3.2147028302475));
#28874=CARTESIAN_POINT('Ctrl Pts',(52.575,-2.74112364039756,-3.22890021009058));
#28875=CARTESIAN_POINT('Ctrl Pts',(52.575,-2.72072957913371,-3.24292437522167));
#28876=CARTESIAN_POINT('Ctrl Pts',(52.575,-2.7002048753135,-3.25677336970125));
#28877=CARTESIAN_POINT('Ctrl Pts',(52.575,-2.68589766540415,-3.26642712513607));
#28878=CARTESIAN_POINT('Ctrl Pts',(52.575,-2.67153123289055,-3.27599285175447));
#28879=CARTESIAN_POINT('Ctrl Pts',(52.575,-2.6571127928066,-3.28546597843703));
#28880=CARTESIAN_POINT('Ctrl Pts',(52.575,-2.54789859172799,-3.35722131093679));
#28881=CARTESIAN_POINT('Ctrl Pts',(52.575,-2.43559227130387,-3.42374252423472));
#28882=CARTESIAN_POINT('Ctrl Pts',(52.575,-2.32058097401746,-3.4848624014124));
#28883=CARTESIAN_POINT('Ctrl Pts',(52.575,-2.20823312579863,-3.54456685520368));
#28884=CARTESIAN_POINT('Ctrl Pts',(52.575,-2.09330325260344,-3.59911731784978));
#28885=CARTESIAN_POINT('Ctrl Pts',(52.575,-1.97613525323649,-3.6483087705229));
#28886=CARTESIAN_POINT('Ctrl Pts',(52.575,-1.85480067208434,-3.6992495080844));
#28887=CARTESIAN_POINT('Ctrl Pts',(52.575,-1.73106512455838,-3.74444394571983));
#28888=CARTESIAN_POINT('Ctrl Pts',(52.575,-1.6053049271685,-3.78360508850387));
#28889=CARTESIAN_POINT('Ctrl Pts',(52.575,-1.48790458016673,-3.82016301261065));
#28890=CARTESIAN_POINT('Ctrl Pts',(52.575,-1.3687391774276,-3.85146273611988));
#28891=CARTESIAN_POINT('Ctrl Pts',(52.575,-1.24812069852349,-3.8772198432059));
#28892=CARTESIAN_POINT('Ctrl Pts',(52.575,-1.23953169122129,-3.8790539567087));
#28893=CARTESIAN_POINT('Ctrl Pts',(52.575,-1.23093532080581,-3.88085994437867));
#28894=CARTESIAN_POINT('Ctrl Pts',(52.575,-1.22233170237281,-3.88263769354989));
#28895=CARTESIAN_POINT('Ctrl Pts',(29.5066541949775,-1.79217368492188,3.65473442716068));
#28896=CARTESIAN_POINT('Ctrl Pts',(29.5462905279758,-2.39896296820844,3.35718290666796));
#28897=CARTESIAN_POINT('Ctrl Pts',(29.6255631939724,-3.46086359021348,2.45430519088321));
#28898=CARTESIAN_POINT('Ctrl Pts',(29.7444721929674,-4.21283764794082,0.502366200250802));
#28899=CARTESIAN_POINT('Ctrl Pts',(29.8633811919624,-3.94100156145658,-1.57116912916543));
#28900=CARTESIAN_POINT('Ctrl Pts',(29.9822901909573,-2.71153768352562,-3.2631402427874));
#28901=CARTESIAN_POINT('Ctrl Pts',(30.1011991899523,-0.823144019015715,
-4.16204660810053));
#28902=CARTESIAN_POINT('Ctrl Pts',(30.2201081889472,1.26526436571728,-4.04962641418862));
#28903=CARTESIAN_POINT('Ctrl Pts',(30.3390171879422,3.04621666442482,-2.95311080905282));
#28904=CARTESIAN_POINT('Ctrl Pts',(30.4579261869372,4.08693028190598,-1.13899868222102));
#28905=CARTESIAN_POINT('Ctrl Pts',(30.5768351859321,4.13451402698658,0.951899428186699));
#28906=CARTESIAN_POINT('Ctrl Pts',(30.6957441849271,3.17740294051253,2.81148064688808));
#28907=CARTESIAN_POINT('Ctrl Pts',(30.814653183922,1.44817770927032,3.9878689759897));
#28908=CARTESIAN_POINT('Ctrl Pts',(30.933562182917,-0.632957413458418,4.19519723441137));
#28909=CARTESIAN_POINT('Ctrl Pts',(31.052471181912,-2.56028269018139,3.38308567277929));
#28910=CARTESIAN_POINT('Ctrl Pts',(31.1713801809069,-3.86545482835077,1.74887813197202));
#28911=CARTESIAN_POINT('Ctrl Pts',(31.2902891799019,-4.23131464672371,-0.310309744443803));
#28912=CARTESIAN_POINT('Ctrl Pts',(31.4091981788968,-3.56895760027616,-2.29409186709539));
#28913=CARTESIAN_POINT('Ctrl Pts',(31.5281071778918,-2.03933759614693,-3.72040561602178));
#28914=CARTESIAN_POINT('Ctrl Pts',(31.6470161768868,-0.0141549844227289,
-4.24265429393642));
#28915=CARTESIAN_POINT('Ctrl Pts',(31.7659251758817,2.01446731467499,-3.73393053486277));
#28916=CARTESIAN_POINT('Ctrl Pts',(31.8848341748767,3.55357052479912,-2.31785511487955));
#28917=CARTESIAN_POINT('Ctrl Pts',(32.0037431738717,4.229149869261,-0.338536837555411));
#28918=CARTESIAN_POINT('Ctrl Pts',(32.1226521728666,3.87703838273484,1.72304648374135));
#28919=CARTESIAN_POINT('Ctrl Pts',(32.2415611718616,2.58279977386025,3.36592648990226));
#28920=CARTESIAN_POINT('Ctrl Pts',(32.3604701708566,0.660936292926016,4.19088045920181));
#28921=CARTESIAN_POINT('Ctrl Pts',(32.4793791698515,-1.42153586561542,3.99744313151944));
#28922=CARTESIAN_POINT('Ctrl Pts',(32.5982881688465,-3.15857231724438,2.83262011635301));
#28923=CARTESIAN_POINT('Ctrl Pts',(32.7171971678415,-4.12807015963076,0.979465448103537));
#28924=CARTESIAN_POINT('Ctrl Pts',(32.8361061668364,-4.09443971780787,-1.11170104079509));
#28925=CARTESIAN_POINT('Ctrl Pts',(32.9550151658314,-3.06585324807998,-2.93272222825354));
#28926=CARTESIAN_POINT('Ctrl Pts',(33.0739241648263,-1.29225906543464,-4.04108677395906));
#28927=CARTESIAN_POINT('Ctrl Pts',(33.1928331638213,0.795356335102055,-4.16746015062799));
#28928=CARTESIAN_POINT('Ctrl Pts',(33.3117421628162,2.68969875215823,-3.2811334062333));
#28929=CARTESIAN_POINT('Ctrl Pts',(33.4306511618112,3.93043965810529,-1.59748549315922));
#28930=CARTESIAN_POINT('Ctrl Pts',(33.5495601608062,4.21607683810534,0.47435419472437));
#28931=CARTESIAN_POINT('Ctrl Pts',(33.6684691598011,3.47719995677159,2.43092498187187));
#28932=CARTESIAN_POINT('Ctrl Pts',(33.7873781587961,1.89335739132502,3.79677673765208));
#28933=CARTESIAN_POINT('Ctrl Pts',(33.906287157791,-0.15057433877126,4.24000509143145));
#28934=CARTESIAN_POINT('Ctrl Pts',(34.025196156786,-2.1579162406289,3.65290477637881));
#28935=CARTESIAN_POINT('Ctrl Pts',(34.144105155781,-3.64088071375389,2.17814219808442));
#28936=CARTESIAN_POINT('Ctrl Pts',(34.2630141547759,-4.23910479193002,0.174087247944916));
#28937=CARTESIAN_POINT('Ctrl Pts',(34.3819231537709,-3.80721897563096,-1.87227120857439));
#28938=CARTESIAN_POINT('Ctrl Pts',(34.5008321527658,-2.45017227519968,-3.46366447981092));
#28939=CARTESIAN_POINT('Ctrl Pts',(34.6197411517608,-0.497729417387068,
-4.21338121156021));
#28940=CARTESIAN_POINT('Ctrl Pts',(34.7386501507558,1.57566256123941,-3.93923892395085));
#28941=CARTESIAN_POINT('Ctrl Pts',(34.8575591497507,3.26616577576251,-2.70785467337129));
#28942=CARTESIAN_POINT('Ctrl Pts',(34.9764681487457,4.16298498204543,-0.818456991005179));
#28943=CARTESIAN_POINT('Ctrl Pts',(35.0953771477406,4.04819154107314,1.26982717471511));
#28944=CARTESIAN_POINT('Ctrl Pts',(35.2142861467356,2.94968046020461,3.04954111130644));
#28945=CARTESIAN_POINT('Ctrl Pts',(35.3331951457306,1.13439185749204,4.0882112128065));
#28946=CARTESIAN_POINT('Ctrl Pts',(35.4521041447256,-0.956555954881787,
4.13343882403517));
#28947=CARTESIAN_POINT('Ctrl Pts',(35.5710131437205,-2.81505899362824,3.17423355619177));
#28948=CARTESIAN_POINT('Ctrl Pts',(35.6899221427155,-3.98949776286473,1.44368397059688));
#28949=CARTESIAN_POINT('Ctrl Pts',(35.8088311417104,-4.1944815831844,-0.637683350251475));
#28950=CARTESIAN_POINT('Ctrl Pts',(35.9277401407054,-3.38019902696682,-2.56409249929749));
#28951=CARTESIAN_POINT('Ctrl Pts',(36.0466491397003,-1.74452218259612,-3.86742267683414));
#28952=CARTESIAN_POINT('Ctrl Pts',(36.1655581386953,0.315076609834192,-4.23096236532504));
#28953=CARTESIAN_POINT('Ctrl Pts',(36.2844671376903,2.29811123382828,-3.56637078327709));
#28954=CARTESIAN_POINT('Ctrl Pts',(36.4033761366852,3.72270080001742,-2.03514484998292));
#28955=CARTESIAN_POINT('Ctrl Pts',(36.5222851356802,4.24266754688635,-0.0093751510681078));
#28956=CARTESIAN_POINT('Ctrl Pts',(36.6411941346751,3.73165864358157,2.01867272598657));
#28957=CARTESIAN_POINT('Ctrl Pts',(36.7601031336701,2.31385014926909,3.55617959242768));
#28958=CARTESIAN_POINT('Ctrl Pts',(36.8790121326651,0.333772013114966,4.22952858485353));
#28959=CARTESIAN_POINT('Ctrl Pts',(36.99792113166,-1.72741330724408,3.87509471792328));
#28960=CARTESIAN_POINT('Ctrl Pts',(37.116830130655,-3.36883416623464,2.57900604248567));
#28961=CARTESIAN_POINT('Ctrl Pts',(37.23573912965,-4.19162241816321,0.65621437846393));
#28962=CARTESIAN_POINT('Ctrl Pts',(37.3546481286449,-3.99583907563888,-1.42603852981441));
#28963=CARTESIAN_POINT('Ctrl Pts',(37.4735571276399,-2.82905983413317,-3.16176157564063));
#28964=CARTESIAN_POINT('Ctrl Pts',(37.5924661266349,-0.974814094226818,
-4.12917101732149));
#28965=CARTESIAN_POINT('Ctrl Pts',(37.7113751256298,1.11631317895359,-4.09318466350003));
#28966=CARTESIAN_POINT('Ctrl Pts',(37.8302841246248,2.93617439347552,-3.06254726405115));
#28967=CARTESIAN_POINT('Ctrl Pts',(37.9491931236197,4.04254008318163,-1.28770550784711));
#28968=CARTESIAN_POINT('Ctrl Pts',(38.0681021226147,4.16656144887969,0.800050936289306));
#28969=CARTESIAN_POINT('Ctrl Pts',(38.1870111216096,3.27810107619118,2.69339361556102));
#28970=CARTESIAN_POINT('Ctrl Pts',(38.3059201206047,1.593056403167,3.93223689564486));
#28971=CARTESIAN_POINT('Ctrl Pts',(38.4248291195996,-0.479103781660292,
4.21553977736235));
#28972=CARTESIAN_POINT('Ctrl Pts',(38.5437381185946,-2.43484088061553,3.47445898581872));
#28973=CARTESIAN_POINT('Ctrl Pts',(38.6626471175895,-3.79890743219015,1.88907880761477));
#28974=CARTESIAN_POINT('Ctrl Pts',(38.7815561165844,-4.23983271101909,-0.155351304211019));
#28975=CARTESIAN_POINT('Ctrl Pts',(38.9004651155794,-3.65047142573015,-2.16202983439362));
#28976=CARTESIAN_POINT('Ctrl Pts',(39.0193741145744,-2.17403875473271,-3.64333320582671));
#28977=CARTESIAN_POINT('Ctrl Pts',(39.1382831135694,-0.169311715692027,
-4.23929647022592));
#28978=CARTESIAN_POINT('Ctrl Pts',(39.2571921125643,1.87656008277306,-3.80511074896768));
#28979=CARTESIAN_POINT('Ctrl Pts',(39.3761011115593,3.46642106848062,-2.4462615072031));
#28980=CARTESIAN_POINT('Ctrl Pts',(39.4950101105543,4.21394248995934,-0.49299624037214));
#28981=CARTESIAN_POINT('Ctrl Pts',(39.6139191095491,3.93745486993259,1.58012745604));
#28982=CARTESIAN_POINT('Ctrl Pts',(39.7328281085442,2.7041860128382,3.26915872948103));
#28983=CARTESIAN_POINT('Ctrl Pts',(39.8517371075391,0.813740946052253,4.1640155130528));
#28984=CARTESIAN_POINT('Ctrl Pts',(39.9706461065341,-1.27433631150534,4.04653670722897));
#28985=CARTESIAN_POINT('Ctrl Pts',(40.089555105529,-3.05296367944959,2.94668522964312));
#28986=CARTESIAN_POINT('Ctrl Pts',(40.208464104524,-4.08928438704866,1.12890284381863));
#28987=CARTESIAN_POINT('Ctrl Pts',(40.327373103519,-4.13276214523759,-0.959452031103675));
#28988=CARTESIAN_POINT('Ctrl Pts',(40.4462821025139,-3.17025406296392,-2.82213573711675));
#28989=CARTESIAN_POINT('Ctrl Pts',(40.5651911015089,-1.44080558796838,-3.98425201455624));
#28990=CARTESIAN_POINT('Ctrl Pts',(40.7237364335021,1.3412377851549,-4.2793985106552));
#28991=CARTESIAN_POINT('Ctrl Pts',(40.9219180984939,4.38508550900277,-1.98115657932714));
#28992=CARTESIAN_POINT('Ctrl Pts',(41.1597360964836,4.03738561363306,2.61791400162535));
#28993=CARTESIAN_POINT('Ctrl Pts',(41.3579177614753,0.682606151108172,4.43240558295318));
#28994=CARTESIAN_POINT('Ctrl Pts',(41.5164630934686,-2.02344151873906,3.72234728068988));
#28995=CARTESIAN_POINT('Ctrl Pts',(41.6353720924636,-3.55851387613991,2.31342601692174));
#28996=CARTESIAN_POINT('Ctrl Pts',(41.7542810914585,-4.23003633407526,0.327205992458881));
#28997=CARTESIAN_POINT('Ctrl Pts',(41.8731900904534,-3.87307885762452,-1.73087509415429));
#28998=CARTESIAN_POINT('Ctrl Pts',(41.9920990894484,-2.5752427483792,-3.37219006842077));
#28999=CARTESIAN_POINT('Ctrl Pts',(42.1110080884434,-0.651474736920205,
-4.19213227664958));
#29000=CARTESIAN_POINT('Ctrl Pts',(42.2299170874383,1.43053091718906,-3.99434360254506));
#29001=CARTESIAN_POINT('Ctrl Pts',(42.3488260864333,3.16495106439444,-2.82543900138727));
#29002=CARTESIAN_POINT('Ctrl Pts',(42.4677350854282,4.13026450704979,-0.970190049367721));
#29003=CARTESIAN_POINT('Ctrl Pts',(42.5866440844232,4.09192548053664,1.12093820678962));
#29004=CARTESIAN_POINT('Ctrl Pts',(42.7055530834182,3.05923685698906,2.9396156616928));
#29005=CARTESIAN_POINT('Ctrl Pts',(42.8244620824131,1.28315058703404,4.04399185547656));
#29006=CARTESIAN_POINT('Ctrl Pts',(42.9433710814081,-0.804744663182227,
4.16565565627073));
#29007=CARTESIAN_POINT('Ctrl Pts',(43.0622800804031,-2.69708497911968,3.27506549112629));
#29008=CARTESIAN_POINT('Ctrl Pts',(43.181189079398,-3.93402920382485,1.58862483246787));
#29009=CARTESIAN_POINT('Ctrl Pts',(43.300098078393,-4.21499729336116,-0.483852521028536));
#29010=CARTESIAN_POINT('Ctrl Pts',(43.419007077388,-3.47171372465588,-2.43875382803693));
#29011=CARTESIAN_POINT('Ctrl Pts',(43.5379160763829,-1.88479759986051,-3.80103319712063));
#29012=CARTESIAN_POINT('Ctrl Pts',(43.6568250753779,0.160127627215037,-4.23965507926387));
#29013=CARTESIAN_POINT('Ctrl Pts',(43.7757340743728,2.16614156925702,-3.64803322477728));
#29014=CARTESIAN_POINT('Ctrl Pts',(43.8946430733678,3.64577930876166,-2.16993296345209));
#29015=CARTESIAN_POINT('Ctrl Pts',(44.0135520723628,4.23948628841551,-0.1645351582025));
#29016=CARTESIAN_POINT('Ctrl Pts',(44.1324610713577,3.80299066814145,1.88084496359989));
#29017=CARTESIAN_POINT('Ctrl Pts',(44.2513700703527,2.44236165043659,3.46917647027723));
#29018=CARTESIAN_POINT('Ctrl Pts',(44.3702790693477,0.488234470571936,4.21449201028578));
#29019=CARTESIAN_POINT('Ctrl Pts',(44.4891880683426,-1.58453454124508,3.93567860682148));
#29020=CARTESIAN_POINT('Ctrl Pts',(44.6080970673376,-3.27225888233889,2.70048840272595));
#29021=CARTESIAN_POINT('Ctrl Pts',(44.7270060663325,-4.16481857957887,0.809074784004825));
#29022=CARTESIAN_POINT('Ctrl Pts',(44.8459150653275,-4.04532006216723,-1.27894542556692));
#29023=CARTESIAN_POINT('Ctrl Pts',(44.9648240643225,-2.94280167925739,-3.05617965494951));
#29024=CARTESIAN_POINT('Ctrl Pts',(45.0837330633174,-1.12517733033491,-4.09075687156072));
#29025=CARTESIAN_POINT('Ctrl Pts',(45.2026420623124,0.965867082001261,-4.13127299833094));
#29026=CARTESIAN_POINT('Ctrl Pts',(45.3215510613073,2.82220410049894,-3.16788254548659));
#29027=CARTESIAN_POINT('Ctrl Pts',(45.4404600603023,3.99274057599417,-1.43469108161613));
#29028=CARTESIAN_POINT('Ctrl Pts',(45.5593690592973,4.193034093298,0.647132829719501));
#29029=CARTESIAN_POINT('Ctrl Pts',(45.6782780582922,3.37441297664422,2.57170232918147));
#29030=CARTESIAN_POINT('Ctrl Pts',(45.7971870572872,1.73580359220705,3.87134365513335));
#29031=CARTESIAN_POINT('Ctrl Pts',(45.9160960562822,-0.324609107543747,
4.23024168744071));
#29032=CARTESIAN_POINT('Ctrl Pts',(46.0350050552771,-2.306141225207,3.56118357519822));
#29033=CARTESIAN_POINT('Ctrl Pts',(46.1539140542721,-3.7272769830857,2.02675161236416));
#29034=CARTESIAN_POINT('Ctrl Pts',(46.272823053267,-4.24267790113794,-0.000184544637164212));
#29035=CARTESIAN_POINT('Ctrl Pts',(46.391732052262,-3.72710065291479,-2.02707585696816));
#29036=CARTESIAN_POINT('Ctrl Pts',(46.5106410512569,-2.30583141340579,-3.56138418312489));
#29037=CARTESIAN_POINT('Ctrl Pts',(46.6295500502519,-0.324241098922964,
-4.23026991061211));
#29038=CARTESIAN_POINT('Ctrl Pts',(46.7484590492469,1.73614037090757,-3.87119263526966));
#29039=CARTESIAN_POINT('Ctrl Pts',(46.8673680482418,3.37463668760993,-2.57140876437375));
#29040=CARTESIAN_POINT('Ctrl Pts',(46.9862770472368,4.1930903743722,-0.646768056731501));
#29041=CARTESIAN_POINT('Ctrl Pts',(47.1051860462317,3.99261575077701,1.43503842231084));
#29042=CARTESIAN_POINT('Ctrl Pts',(47.2240950452267,2.82192850173731,3.16812804948658));
#29043=CARTESIAN_POINT('Ctrl Pts',(47.3430040442217,0.965507680676692,4.13135700774157));
#29044=CARTESIAN_POINT('Ctrl Pts',(47.4619130432167,-1.12553319906949,4.0906589719327));
#29045=CARTESIAN_POINT('Ctrl Pts',(47.5808220422116,-2.943067538678,3.05592363609448));
#29046=CARTESIAN_POINT('Ctrl Pts',(47.6997310412065,-4.04543130796411,1.27859350045461));
#29047=CARTESIAN_POINT('Ctrl Pts',(47.8186400402016,-4.16474817883747,-0.809437096833958));
#29048=CARTESIAN_POINT('Ctrl Pts',(47.9375490391964,-3.27202394254474,-2.70077306086147));
#29049=CARTESIAN_POINT('Ctrl Pts',(48.0564580381915,-1.58419215321593,-3.93581643735453));
#29050=CARTESIAN_POINT('Ctrl Pts',(48.1753670371864,0.48860110601671,-4.21444952111902));
#29051=CARTESIAN_POINT('Ctrl Pts',(48.2942760361814,2.44266344009801,-3.46896398442958));
#29052=CARTESIAN_POINT('Ctrl Pts',(48.4131850351763,3.80315427688869,-1.88051411934194));
#29053=CARTESIAN_POINT('Ctrl Pts',(48.5320940341713,4.23947195846584,0.164903972792664));
#29054=CARTESIAN_POINT('Ctrl Pts',(48.6510030331663,3.6455905234561,2.17025011050524));
#29055=CARTESIAN_POINT('Ctrl Pts',(48.7699120321612,2.16582420148474,3.64822166748742));
#29056=CARTESIAN_POINT('Ctrl Pts',(48.8888210311562,0.159758802432322,4.23966896489628));
#29057=CARTESIAN_POINT('Ctrl Pts',(49.0077300301511,-1.88512826562663,3.80086927281119));
#29058=CARTESIAN_POINT('Ctrl Pts',(49.1266390291461,-3.47192586100346,2.43845168550668));
#29059=CARTESIAN_POINT('Ctrl Pts',(49.2455480281411,-4.21503938678446,0.483486064662875));
#29060=CARTESIAN_POINT('Ctrl Pts',(49.364457027136,-3.93389095371854,-1.58896751732501));
#29061=CARTESIAN_POINT('Ctrl Pts',(49.483366026131,-2.69680012382729,-3.27529920754662));
#29062=CARTESIAN_POINT('Ctrl Pts',(49.6022750251259,-0.804382137054723,
-4.16572744962391));
#29063=CARTESIAN_POINT('Ctrl Pts',(49.7211840241209,1.28350211887322,-4.04387661996188));
#29064=CARTESIAN_POINT('Ctrl Pts',(49.8400930231158,3.05949311031172,-2.93935668390779));
#29065=CARTESIAN_POINT('Ctrl Pts',(49.9590020221109,4.09202191338058,-1.12056792152273));
#29066=CARTESIAN_POINT('Ctrl Pts',(50.0779110211058,4.13018221941277,0.970520809410563));
#29067=CARTESIAN_POINT('Ctrl Pts',(50.1968200201008,3.16470100669801,2.82577128347271));
#29068=CARTESIAN_POINT('Ctrl Pts',(50.3157290190956,1.43019190307756,3.99435438105406));
#29069=CARTESIAN_POINT('Ctrl Pts',(50.4346380180907,-0.651856340959766,
4.1923023665036));
#29070=CARTESIAN_POINT('Ctrl Pts',(50.5535470170856,-2.57550234917945,3.37151352187054));
#29071=CARTESIAN_POINT('Ctrl Pts',(50.6724560160807,-3.87329677722202,1.73144099605029));
#29072=CARTESIAN_POINT('Ctrl Pts',(50.7913650150755,-4.22987328984736,-0.329374754514203));
#29073=CARTESIAN_POINT('Ctrl Pts',(50.9102740140706,-3.55858319850174,-2.31015180666798));
#29074=CARTESIAN_POINT('Ctrl Pts',(51.0291830130655,-2.02255111411372,-3.72955803196629));
#29075=CARTESIAN_POINT('Ctrl Pts',(51.1480920120605,0.00496435909204525,
-4.24267489657216));
#29076=CARTESIAN_POINT('Ctrl Pts',(51.2670010110554,2.03127363780405,-3.72481476796509));
#29077=CARTESIAN_POINT('Ctrl Pts',(51.3859100100504,3.56397955602096,-2.30181723828556));
#29078=CARTESIAN_POINT('Ctrl Pts',(51.5048190090453,4.23063280642202,-0.3194758487847));
#29079=CARTESIAN_POINT('Ctrl Pts',(51.6237280080403,3.86923365048362,1.74050225085362));
#29080=CARTESIAN_POINT('Ctrl Pts',(51.7426370070353,2.56760636844359,3.37752823139821));
#29081=CARTESIAN_POINT('Ctrl Pts',(51.8615460060302,0.642041384412004,4.19382294217941));
#29082=CARTESIAN_POINT('Ctrl Pts',(51.9804550050252,-1.43953109567099,3.99098337113032));
#29083=CARTESIAN_POINT('Ctrl Pts',(52.0993640040201,-3.17131432296482,2.81838363574518));
#29084=CARTESIAN_POINT('Ctrl Pts',(52.2182730030151,-4.13242404491094,0.960800318946468));
#29085=CARTESIAN_POINT('Ctrl Pts',(52.3371820020101,-4.08942446914233,-1.13003555618484));
#29086=CARTESIAN_POINT('Ctrl Pts',(52.456091001005,-3.05253321900086,-2.94673237789893));
#29087=CARTESIAN_POINT('Ctrl Pts',(52.5353636670017,-1.86695937376299,-3.67969605923878));
#29088=CARTESIAN_POINT('Ctrl Pts',(52.575,-1.2223317023727,-3.88263769354992));
#29089=CARTESIAN_POINT('Ctrl Pts',(29.6711027966516,-1.91758108071809,3.91047455474607));
#29090=CARTESIAN_POINT('Ctrl Pts',(29.71073912965,-2.5668304583885,3.5921018596015));
#29091=CARTESIAN_POINT('Ctrl Pts',(29.7900117956466,-3.70303760141909,2.62604525439793));
#29092=CARTESIAN_POINT('Ctrl Pts',(29.9089207946415,-4.50763106153991,0.537519286940777));
#29093=CARTESIAN_POINT('Ctrl Pts',(30.0278297936365,-4.21677323850402,-1.68111172596939));
#29094=CARTESIAN_POINT('Ctrl Pts',(30.1467387926315,-2.9012775967691,-3.49147855810178));
#29095=CARTESIAN_POINT('Ctrl Pts',(30.2656477916264,-0.880743541125958,
-4.45328591749101));
#29096=CARTESIAN_POINT('Ctrl Pts',(30.3845567906214,1.35380126949692,-4.33299911786337));
#29097=CARTESIAN_POINT('Ctrl Pts',(30.5034657896164,3.25937574723617,-3.15975480744252));
#29098=CARTESIAN_POINT('Ctrl Pts',(30.6223747886113,4.3729133246025,-1.21870014182534));
#29099=CARTESIAN_POINT('Ctrl Pts',(30.7412837876063,4.42382674336541,1.01850861308497));
#29100=CARTESIAN_POINT('Ctrl Pts',(30.8601927866012,3.39974178608172,3.00821407134581));
#29101=CARTESIAN_POINT('Ctrl Pts',(30.9791017855962,1.54951397857154,4.26692020147249));
#29102=CARTESIAN_POINT('Ctrl Pts',(31.0980107845912,-0.677248623367102,
4.48875625965845));
#29103=CARTESIAN_POINT('Ctrl Pts',(31.2169197835861,-2.73943853170453,3.6198171723813));
#29104=CARTESIAN_POINT('Ctrl Pts',(31.3358287825811,-4.13594012097048,1.87125592043129));
#29105=CARTESIAN_POINT('Ctrl Pts',(31.4547377815761,-4.52740098874766,-0.332023676116975));
#29106=CARTESIAN_POINT('Ctrl Pts',(31.573646780571,-3.81869549238083,-2.45462099950604));
#29107=CARTESIAN_POINT('Ctrl Pts',(31.692555779566,-2.18204029245024,-3.98074108659382));
#29108=CARTESIAN_POINT('Ctrl Pts',(31.811464778561,-0.0151454797909917,
-4.53953412804105));
#29109=CARTESIAN_POINT('Ctrl Pts',(31.9303737775559,2.15542971244672,-3.99521241194915));
#29110=CARTESIAN_POINT('Ctrl Pts',(32.0492827765509,3.80223170593499,-2.48004708111342));
#29111=CARTESIAN_POINT('Ctrl Pts',(32.1681917755458,4.52508473093102,-0.362225960733676));
#29112=CARTESIAN_POINT('Ctrl Pts',(32.2871007745408,4.14833423484531,1.84361670200747));
#29113=CARTESIAN_POINT('Ctrl Pts',(32.4060097735358,2.76353124884398,3.60145727527845));
#29114=CARTESIAN_POINT('Ctrl Pts',(32.5249187725307,0.707185325584214,4.48413741800195));
#29115=CARTESIAN_POINT('Ctrl Pts',(32.6438277715257,-1.5210078712796,4.27716430876084));
#29116=CARTESIAN_POINT('Ctrl Pts',(32.7627367705206,-3.37959348950701,3.03083277568429));
#29117=CARTESIAN_POINT('Ctrl Pts',(32.8816457695156,-4.41693196623964,1.04800356589453));
#29118=CARTESIAN_POINT('Ctrl Pts',(33.0005547685106,-4.38094823345843,-1.1894923472979));
#29119=CARTESIAN_POINT('Ctrl Pts',(33.1194637675055,-3.28038640129495,-3.13793953522177));
#29120=CARTESIAN_POINT('Ctrl Pts',(33.2383727665005,-1.38268492396259,-4.32386191610767));
#29121=CARTESIAN_POINT('Ctrl Pts',(33.3572817654954,0.851011413376168,-4.4590782727843));
#29122=CARTESIAN_POINT('Ctrl Pts',(33.4761907644904,2.87791048566509,-3.51073079358346));
#29123=CARTESIAN_POINT('Ctrl Pts',(33.5950997634854,4.20547226571702,-1.70926957815328));
#29124=CARTESIAN_POINT('Ctrl Pts',(33.7140087624804,4.51109691411248,0.507547140668087));
#29125=CARTESIAN_POINT('Ctrl Pts',(33.8329177614753,3.72051710561174,2.60102901471052));
#29126=CARTESIAN_POINT('Ctrl Pts',(33.9518267604703,2.02584511935904,4.06245627925823));
#29127=CARTESIAN_POINT('Ctrl Pts',(34.0707357594652,-0.161110781671782,
4.53669954752843));
#29128=CARTESIAN_POINT('Ctrl Pts',(34.1896447584602,-2.30891648037153,3.90851687410766));
#29129=CARTESIAN_POINT('Ctrl Pts',(34.3085537574551,-3.89565142741744,2.33055774967624));
#29130=CARTESIAN_POINT('Ctrl Pts',(34.4274627564501,-4.53573624954818,0.186269007218487));
#29131=CARTESIAN_POINT('Ctrl Pts',(34.546371755445,-4.07362921308556,-2.00328343047395));
#29132=CARTESIAN_POINT('Ctrl Pts',(34.66528075444,-2.62162313784214,-3.70603448333205));
#29133=CARTESIAN_POINT('Ctrl Pts',(34.784189753435,-0.532558045086988,-4.50821266103637));
#29134=CARTESIAN_POINT('Ctrl Pts',(34.9030987524299,1.68591958605854,-4.21488726039734));
#29135=CARTESIAN_POINT('Ctrl Pts',(35.0220077514249,3.49471580281806,-2.89733686789252));
#29136=CARTESIAN_POINT('Ctrl Pts',(35.1409167504199,4.4542899541748,-0.875728538220039));
#29137=CARTESIAN_POINT('Ctrl Pts',(35.2598257494149,4.33146383946785,1.35868336116181));
#29138=CARTESIAN_POINT('Ctrl Pts',(35.3787347484098,3.15608441985291,3.26293282236661));
#29139=CARTESIAN_POINT('Ctrl Pts',(35.4976437474048,1.21377095442749,4.37428388867294));
#29140=CARTESIAN_POINT('Ctrl Pts',(35.6165527463997,-1.02349098034518,4.42267630306216));
#29141=CARTESIAN_POINT('Ctrl Pts',(35.7354617453947,-3.01204281298337,3.39635062401849));
#29142=CARTESIAN_POINT('Ctrl Pts',(35.8543707443896,-4.26866296274744,1.54470579042862));
#29143=CARTESIAN_POINT('Ctrl Pts',(35.9732797433846,-4.48799053072001,-0.68230525769852));
#29144=CARTESIAN_POINT('Ctrl Pts',(36.0921887423795,-3.61672853346016,-2.74351493230322));
#29145=CARTESIAN_POINT('Ctrl Pts',(36.2110977413746,-1.86659516339526,-4.1380456696978));
#29146=CARTESIAN_POINT('Ctrl Pts',(36.3300067403695,0.337124103025285,-4.52702405644983));
#29147=CARTESIAN_POINT('Ctrl Pts',(36.4489157393645,2.4589216215207,-3.81592766280134));
#29148=CARTESIAN_POINT('Ctrl Pts',(36.5678247383594,3.9831968761436,-2.17755415877468));
#29149=CARTESIAN_POINT('Ctrl Pts',(36.6867337373544,4.53954830836646,-0.0100311774848461));
#29150=CARTESIAN_POINT('Ctrl Pts',(36.8056427363494,3.99278154502206,2.15992939751383));
#29151=CARTESIAN_POINT('Ctrl Pts',(36.9245517353443,2.47576186794007,3.80502334313229));
#29152=CARTESIAN_POINT('Ctrl Pts',(37.0434607343393,0.357127717590833,4.52548994715605));
#29153=CARTESIAN_POINT('Ctrl Pts',(37.1623697333342,-1.84828909408761,4.14625456204281));
#29154=CARTESIAN_POINT('Ctrl Pts',(37.2812787323292,-3.60456841633064,2.75947205102715));
#29155=CARTESIAN_POINT('Ctrl Pts',(37.4001877313241,-4.48493129555913,0.702132995046478));
#29156=CARTESIAN_POINT('Ctrl Pts',(37.5190967303191,-4.27544800903229,-1.52582560951193));
#29157=CARTESIAN_POINT('Ctrl Pts',(37.6380057293141,-3.02702336263229,-3.38300591633462));
#29158=CARTESIAN_POINT('Ctrl Pts',(37.756914728309,-1.04302673342079,-4.4181098564732));
#29159=CARTESIAN_POINT('Ctrl Pts',(37.875823727304,1.19442721993263,-4.37960535669586));
#29160=CARTESIAN_POINT('Ctrl Pts',(37.994732726299,3.14163326578642,-3.27684908095586));
#29161=CARTESIAN_POINT('Ctrl Pts',(38.113641725294,4.32541692067733,-1.37781273107568));
#29162=CARTESIAN_POINT('Ctrl Pts',(38.2325507242888,4.45811668435999,0.856034519392032));
#29163=CARTESIAN_POINT('Ctrl Pts',(38.3514597232839,3.50748627617526,2.88186389722148));
#29164=CARTESIAN_POINT('Ctrl Pts',(38.4703687222788,1.70453056248457,4.20739526499576));
#29165=CARTESIAN_POINT('Ctrl Pts',(38.5892777212738,-0.51262908006167,4.51052227253135));
#29166=CARTESIAN_POINT('Ctrl Pts',(38.7081867202687,-2.60521892856097,3.7175843351519));
#29167=CARTESIAN_POINT('Ctrl Pts',(38.8270957192637,-4.06473606919677,2.02126714165294));
#29168=CARTESIAN_POINT('Ctrl Pts',(38.9460047182586,-4.53651510479265,-0.166222015380657));
#29169=CARTESIAN_POINT('Ctrl Pts',(39.0649137172536,-3.90591324969007,-2.31331792295678));
#29170=CARTESIAN_POINT('Ctrl Pts',(39.1838227162486,-2.32616716777937,-3.89827553268081));
#29171=CARTESIAN_POINT('Ctrl Pts',(39.3027317152435,-0.181159306983774,
-4.53594134053735));
#29172=CARTESIAN_POINT('Ctrl Pts',(39.4216407142385,2.00787241874566,-4.07137346321188));
#29173=CARTESIAN_POINT('Ctrl Pts',(39.5405497132335,3.70898396435881,-2.61743871376292));
#29174=CARTESIAN_POINT('Ctrl Pts',(39.6594587122284,4.50881321490469,-0.527493663899006));
#29175=CARTESIAN_POINT('Ctrl Pts',(39.7783677112234,4.21297836715714,1.69069691197792));
#29176=CARTESIAN_POINT('Ctrl Pts',(39.8972767102183,2.89341149275226,3.4979181885435));
#29177=CARTESIAN_POINT('Ctrl Pts',(40.0161857092133,0.870682487910497,4.45539259661367));
#29178=CARTESIAN_POINT('Ctrl Pts',(40.1350947082083,-1.36350802490509,4.32969320858648));
#29179=CARTESIAN_POINT('Ctrl Pts',(40.2540037072032,-3.26659488479615,3.15287959796235));
#29180=CARTESIAN_POINT('Ctrl Pts',(40.3729127061982,-4.37543215830797,1.20789784689305));
#29181=CARTESIAN_POINT('Ctrl Pts',(40.4918217051931,-4.42195227364979,-1.02658970956888));
#29182=CARTESIAN_POINT('Ctrl Pts',(40.6107307041881,-3.39209266565834,-3.01961475176409));
#29183=CARTESIAN_POINT('Ctrl Pts',(40.729639703183,-1.54162599290793,-4.26305014307757));
#29184=CARTESIAN_POINT('Ctrl Pts',(40.8881850351763,1.43509093074836,-4.57884952218982));
#29185=CARTESIAN_POINT('Ctrl Pts',(41.086366700168,4.69193197073497,-2.11978805760871));
#29186=CARTESIAN_POINT('Ctrl Pts',(41.3241846981578,4.31990176700075,2.80110259552361));
#29187=CARTESIAN_POINT('Ctrl Pts',(41.5223663631495,0.730371532602854,4.74256326797414));
#29188=CARTESIAN_POINT('Ctrl Pts',(41.6809116951428,-2.16503188665146,3.98281861929281));
#29189=CARTESIAN_POINT('Ctrl Pts',(41.7998206941377,-3.80752096840224,2.47530805692173));
#29190=CARTESIAN_POINT('Ctrl Pts',(41.9187296931327,-4.52603322614153,0.350102239484753));
#29191=CARTESIAN_POINT('Ctrl Pts',(42.0376386921276,-4.14409764187218,-1.85199311961837));
#29192=CARTESIAN_POINT('Ctrl Pts',(42.1565476911226,-2.75544542032698,-3.60815914785125));
#29193=CARTESIAN_POINT('Ctrl Pts',(42.2754566901175,-0.697061696974139,
-4.48547683140511));
#29194=CARTESIAN_POINT('Ctrl Pts',(42.3943656891125,1.53063235179888,-4.27384789017351));
#29195=CARTESIAN_POINT('Ctrl Pts',(42.5132746881075,3.38641858963907,-3.02314916202976));
#29196=CARTESIAN_POINT('Ctrl Pts',(42.6321836871024,4.41927986317098,-1.03807912091381));
#29197=CARTESIAN_POINT('Ctrl Pts',(42.7510926860974,4.37825806237496,1.19937588420037));
#29198=CARTESIAN_POINT('Ctrl Pts',(42.8700016850923,3.27330702808166,3.14531533682823));
#29199=CARTESIAN_POINT('Ctrl Pts',(42.9889106840873,1.37293907957147,4.32697028077277));
#29200=CARTESIAN_POINT('Ctrl Pts',(43.1078196830823,-0.861056689934789,
4.45714750889189));
#29201=CARTESIAN_POINT('Ctrl Pts',(43.2267286820772,-2.88581356403206,3.50423827597399));
#29202=CARTESIAN_POINT('Ctrl Pts',(43.3456376810722,-4.20931298998283,1.69978889252144));
#29203=CARTESIAN_POINT('Ctrl Pts',(43.4645466800671,-4.50994182819939,-0.517710112579008));
#29204=CARTESIAN_POINT('Ctrl Pts',(43.5834556790622,-3.71464697427457,-2.6094056845703));
#29205=CARTESIAN_POINT('Ctrl Pts',(43.7023646780571,-2.01668635628528,-4.06701058457831));
#29206=CARTESIAN_POINT('Ctrl Pts',(43.8212736770521,0.171332561699331,-4.53632504325118));
#29207=CARTESIAN_POINT('Ctrl Pts',(43.940182676047,2.31771737656405,-3.90330443556811));
#29208=CARTESIAN_POINT('Ctrl Pts',(44.0590916750419,3.90089280172621,-2.32177407365723));
#29209=CARTESIAN_POINT('Ctrl Pts',(44.178000674037,4.53614444125922,-0.176048509771458));
#29210=CARTESIAN_POINT('Ctrl Pts',(44.2969096730319,4.06910502967991,2.01245713420922));
#29211=CARTESIAN_POINT('Ctrl Pts',(44.4158186720269,2.61326596442736,3.71193217546101));
#29212=CARTESIAN_POINT('Ctrl Pts',(44.5347276710218,0.522398689144923,4.50940118792892));
#29213=CARTESIAN_POINT('Ctrl Pts',(44.6536366700168,-1.69541238307399,4.21107780999301));
#29214=CARTESIAN_POINT('Ctrl Pts',(44.7725456690117,-3.50123527467057,2.88945514228534));
#29215=CARTESIAN_POINT('Ctrl Pts',(44.8914546680068,-4.45625185773881,0.865689811063943));
#29216=CARTESIAN_POINT('Ctrl Pts',(45.0103636670016,-4.3283914287579,-1.36843966183164));
#29217=CARTESIAN_POINT('Ctrl Pts',(45.1292726659967,-3.14872429604695,-3.27003589825739));
#29218=CARTESIAN_POINT('Ctrl Pts',(45.2481816649915,-1.2039116405156,-4.37700767995842));
#29219=CARTESIAN_POINT('Ctrl Pts',(45.3670906639866,1.03345365380405,-4.42035892365329));
#29220=CARTESIAN_POINT('Ctrl Pts',(45.4859996629815,3.01968789887557,-3.3895552011897));
#29221=CARTESIAN_POINT('Ctrl Pts',(45.6049086619765,4.27213269180196,-1.53508362382972));
#29222=CARTESIAN_POINT('Ctrl Pts',(45.7238176609714,4.48644175269473,0.692415964714791));
#29223=CARTESIAN_POINT('Ctrl Pts',(45.8427266599664,3.61053760413,2.7516572602125));
#29224=CARTESIAN_POINT('Ctrl Pts',(45.9616356589614,1.85726648943845,4.14224101854581));
#29225=CARTESIAN_POINT('Ctrl Pts',(46.0805446579563,-0.34732363748649,4.52625294911356));
#29226=CARTESIAN_POINT('Ctrl Pts',(46.1994536569513,-2.46751351173521,3.81037747971504));
#29227=CARTESIAN_POINT('Ctrl Pts',(46.3183626559463,-3.98809327772981,2.16857360415595));
#29228=CARTESIAN_POINT('Ctrl Pts',(46.4372716549412,-4.53955938715706,-0.000197458152468345));
#29229=CARTESIAN_POINT('Ctrl Pts',(46.5561806539361,-3.98790460885106,-2.1689205377837));
#29230=CARTESIAN_POINT('Ctrl Pts',(46.6750896529312,-2.46718202084595,-3.81059212518606));
#29231=CARTESIAN_POINT('Ctrl Pts',(46.7939986519261,-0.346929877453853,
-4.52628314720205));
#29232=CARTESIAN_POINT('Ctrl Pts',(46.912907650921,1.85762683423641,-4.14207943106362));
#29233=CARTESIAN_POINT('Ctrl Pts',(47.031816649916,3.61077696927579,-2.75134315320047));
#29234=CARTESIAN_POINT('Ctrl Pts',(47.1507256489109,4.48650197203841,-0.692025666728421));
#29235=CARTESIAN_POINT('Ctrl Pts',(47.269634647906,4.27199913193732,1.53545526969767));
#29236=CARTESIAN_POINT('Ctrl Pts',(47.3885436469008,3.01939301508414,3.38981788433784));
#29237=CARTESIAN_POINT('Ctrl Pts',(47.5074526458959,1.03306910336338,4.42044881162439));
#29238=CARTESIAN_POINT('Ctrl Pts',(47.6263616448908,-1.20429241117321,4.37690292980164));
#29239=CARTESIAN_POINT('Ctrl Pts',(47.7452706438858,-3.14900875898673,3.26976196447697));
#29240=CARTESIAN_POINT('Ctrl Pts',(47.8641796428807,-4.32851045898203,1.36806311075136));
#29241=CARTESIAN_POINT('Ctrl Pts',(47.9830886418757,-4.45617653070388,-0.866077476741777));
#29242=CARTESIAN_POINT('Ctrl Pts',(48.1019976408706,-3.50098389495883,-2.88975971938056));
#29243=CARTESIAN_POINT('Ctrl Pts',(48.2209066398657,-1.69504603643448,-4.21122528522083));
#29244=CARTESIAN_POINT('Ctrl Pts',(48.3398156388606,0.522790979913529,-4.50935572558172));
#29245=CARTESIAN_POINT('Ctrl Pts',(48.4587246378556,2.61358887182741,-3.7117048209112));
#29246=CARTESIAN_POINT('Ctrl Pts',(48.5776336368505,4.06928008695307,-2.01210313911658));
#29247=CARTESIAN_POINT('Ctrl Pts',(48.6965426358455,4.53612910857099,0.176443132171203));
#29248=CARTESIAN_POINT('Ctrl Pts',(48.8154516348404,3.90069080616449,2.32211341308284));
#29249=CARTESIAN_POINT('Ctrl Pts',(48.9343606338354,2.31737780097448,3.90350606456131));
#29250=CARTESIAN_POINT('Ctrl Pts',(49.0532696328304,0.17093792839381,4.53633990053105));
#29251=CARTESIAN_POINT('Ctrl Pts',(49.1721786318254,-2.01704016039613,4.06683518966148));
#29252=CARTESIAN_POINT('Ctrl Pts',(49.2910876308203,-3.71487395486803,2.60908239960943));
#29253=CARTESIAN_POINT('Ctrl Pts',(49.4099966298152,-4.50998686711097,0.51731801342058));
#29254=CARTESIAN_POINT('Ctrl Pts',(49.5289056288102,-4.2091650658221,-1.70015555675947));
#29255=CARTESIAN_POINT('Ctrl Pts',(49.6478146278052,-2.88550877598391,-3.50448834670629));
#29256=CARTESIAN_POINT('Ctrl Pts',(49.7667236268002,-0.860668796033026,
-4.45722432598666));
#29257=CARTESIAN_POINT('Ctrl Pts',(49.885632625795,1.37331520985932,-4.32684698165025));
#29258=CARTESIAN_POINT('Ctrl Pts',(50.0045416247901,3.27358121273658,-3.14503823706665));
#29259=CARTESIAN_POINT('Ctrl Pts',(50.123450623785,4.37836124310941,-1.19897968821326));
#29260=CARTESIAN_POINT('Ctrl Pts',(50.24235962278,4.41919181745465,1.03843302589838));
#29261=CARTESIAN_POINT('Ctrl Pts',(50.3612686217749,3.38615103414948,3.02350469556191));
#29262=CARTESIAN_POINT('Ctrl Pts',(50.4801776207699,1.53026961516699,4.27385942290892));
#29263=CARTESIAN_POINT('Ctrl Pts',(50.5990866197649,-0.697470003765305,
4.48565882330066));
#29264=CARTESIAN_POINT('Ctrl Pts',(50.7179956187599,-2.7557231866993,3.60743525994027));
#29265=CARTESIAN_POINT('Ctrl Pts',(50.8369046177548,-4.14433081039863,1.85259862051291));
#29266=CARTESIAN_POINT('Ctrl Pts',(50.9558136167497,-4.52585877288994,-0.352422760715905));
#29267=CARTESIAN_POINT('Ctrl Pts',(51.0747226157447,-3.807595141598,-2.47180473372834));
#29268=CARTESIAN_POINT('Ctrl Pts',(51.1936316147397,-2.16407917594154,-3.99053394305953));
#29269=CARTESIAN_POINT('Ctrl Pts',(51.3125406137346,0.00531174023636265,
-4.53955617234671));
#29270=CARTESIAN_POINT('Ctrl Pts',(51.4314496127296,2.17341205843241,-3.9854587690482));
#29271=CARTESIAN_POINT('Ctrl Pts',(51.5503586117245,3.81336910936164,-2.46288695372717));
#29272=CARTESIAN_POINT('Ctrl Pts',(51.6692676107196,4.5266714366548,-0.341831178824977));
#29273=CARTESIAN_POINT('Ctrl Pts',(51.7881766097145,4.13998336627106,1.86229393683439));
#29274=CARTESIAN_POINT('Ctrl Pts',(51.9070856087095,2.74727468452559,3.61387084890872));
#29275=CARTESIAN_POINT('Ctrl Pts',(52.0259946077044,0.686968245402081,4.48728580129519));
#29276=CARTESIAN_POINT('Ctrl Pts',(52.1449036066994,-1.54026231798197,4.27025252648642));
#29277=CARTESIAN_POINT('Ctrl Pts',(52.2638126056943,-3.39322711737773,3.01560009701075));
#29278=CARTESIAN_POINT('Ctrl Pts',(52.3827216046892,-4.42159051474481,1.02803234388526));
#29279=CARTESIAN_POINT('Ctrl Pts',(52.5016306036843,-4.37558204264944,-1.20910982083371));
#29280=CARTESIAN_POINT('Ctrl Pts',(52.6205396026792,-3.26613430286741,-3.15293004541843));
#29281=CARTESIAN_POINT('Ctrl Pts',(52.6998122686759,-1.99759989989662,-3.93718287761649));
#29282=CARTESIAN_POINT('Ctrl Pts',(52.7394486016742,-1.30786439202407,-4.15432535756649));
#29283=CARTESIAN_POINT('Ctrl Pts',(29.8355513983258,-2.04298847651431,4.16621468233146));
#29284=CARTESIAN_POINT('Ctrl Pts',(29.8751877313241,-2.73469794856857,3.82702081253504));
#29285=CARTESIAN_POINT('Ctrl Pts',(29.9544603973208,-3.9452116126247,2.79778531791265));
#29286=CARTESIAN_POINT('Ctrl Pts',(30.0733693963157,-4.80242447513901,0.572672373630749));
#29287=CARTESIAN_POINT('Ctrl Pts',(30.1922783953107,-4.49254491555146,-1.79105432277335));
#29288=CARTESIAN_POINT('Ctrl Pts',(30.3111873943056,-3.09101751001259,-3.71981687341617));
#29289=CARTESIAN_POINT('Ctrl Pts',(30.4300963933007,-0.938343063236198,
-4.74452522688149));
#29290=CARTESIAN_POINT('Ctrl Pts',(30.5490053922956,1.44233817327656,-4.61637182153812));
#29291=CARTESIAN_POINT('Ctrl Pts',(30.6679143912906,3.47253483004752,-3.36639880583222));
#29292=CARTESIAN_POINT('Ctrl Pts',(30.7868233902855,4.65889636729902,-1.29840160142966));
#29293=CARTESIAN_POINT('Ctrl Pts',(30.9057323892805,4.71313945974424,1.08511779798324));
#29294=CARTESIAN_POINT('Ctrl Pts',(31.0246413882754,3.62208063165091,3.20494749580355));
#29295=CARTESIAN_POINT('Ctrl Pts',(31.1435503872704,1.65085024787275,4.54597142695528));
#29296=CARTESIAN_POINT('Ctrl Pts',(31.2624593862653,-0.721539833275788,
4.78231528490551));
#29297=CARTESIAN_POINT('Ctrl Pts',(31.3813683852603,-2.91859437322766,3.85654867198333));
#29298=CARTESIAN_POINT('Ctrl Pts',(31.5002773842553,-4.40642541359019,1.99363370889056));
#29299=CARTESIAN_POINT('Ctrl Pts',(31.6191863832502,-4.8234873307716,-0.353737607790146));
#29300=CARTESIAN_POINT('Ctrl Pts',(31.7380953822452,-4.0684333844855,-2.6151501319167));
#29301=CARTESIAN_POINT('Ctrl Pts',(31.8570043812401,-2.32474298875354,-4.24107655716586));
#29302=CARTESIAN_POINT('Ctrl Pts',(31.9759133802352,-0.0161359751592512,
-4.83641396214568));
#29303=CARTESIAN_POINT('Ctrl Pts',(32.09482237923,2.29639211021845,-4.25649428903554));
#29304=CARTESIAN_POINT('Ctrl Pts',(32.2137313782251,4.05089288707086,-2.64223904734728));
#29305=CARTESIAN_POINT('Ctrl Pts',(32.33264037722,4.82101959260105,-0.385915083911942));
#29306=CARTESIAN_POINT('Ctrl Pts',(32.451549376215,4.41963008695579,1.96418692027359));
#29307=CARTESIAN_POINT('Ctrl Pts',(32.5704583752099,2.94426272382771,3.83698806065463));
#29308=CARTESIAN_POINT('Ctrl Pts',(32.6893673742049,0.753434358242411,4.77739437680209));
#29309=CARTESIAN_POINT('Ctrl Pts',(32.8082763731998,-1.62047987694377,4.55688548600226));
#29310=CARTESIAN_POINT('Ctrl Pts',(32.9271853721948,-3.60061466176965,3.22904543501556));
#29311=CARTESIAN_POINT('Ctrl Pts',(33.0460943711898,-4.70579377284853,1.11654168368553));
#29312=CARTESIAN_POINT('Ctrl Pts',(33.1650033701848,-4.66745674910901,-1.26728365380071));
#29313=CARTESIAN_POINT('Ctrl Pts',(33.2839123691797,-3.49491955450991,-3.34315684219));
#29314=CARTESIAN_POINT('Ctrl Pts',(33.4028213681747,-1.47311078249056,-4.60663705825629));
#29315=CARTESIAN_POINT('Ctrl Pts',(33.5217303671696,0.906666491650291,-4.7506963949406));
#29316=CARTESIAN_POINT('Ctrl Pts',(33.6406393661646,3.06612221917194,-3.74032818093363));
#29317=CARTESIAN_POINT('Ctrl Pts',(33.7595483651595,4.48050487332878,-1.82105366314733));
#29318=CARTESIAN_POINT('Ctrl Pts',(33.8784573641545,4.80611699011961,0.540740086611801));
#29319=CARTESIAN_POINT('Ctrl Pts',(33.9973663631495,3.96383425445189,2.77113304754918));
#29320=CARTESIAN_POINT('Ctrl Pts',(34.1162753621445,2.15833284739307,4.32813582086438));
#29321=CARTESIAN_POINT('Ctrl Pts',(34.2351843611394,-0.171647224572306,
4.8333940036254));
#29322=CARTESIAN_POINT('Ctrl Pts',(34.3540933601344,-2.45991672011416,4.16412897183651));
#29323=CARTESIAN_POINT('Ctrl Pts',(34.4730023591293,-4.150422141081,2.48297330126805));
#29324=CARTESIAN_POINT('Ctrl Pts',(34.5919113581243,-4.83236770716634,0.198450766492061));
#29325=CARTESIAN_POINT('Ctrl Pts',(34.7108203571192,-4.34003945054015,-2.13429565237352));
#29326=CARTESIAN_POINT('Ctrl Pts',(34.8297293561142,-2.7930740004846,-3.94840448685318));
#29327=CARTESIAN_POINT('Ctrl Pts',(34.9486383551091,-0.567386672786905,
-4.80304411051253));
#29328=CARTESIAN_POINT('Ctrl Pts',(35.0675473541042,1.79617661087767,-4.4905355968438));
#29329=CARTESIAN_POINT('Ctrl Pts',(35.1864563530991,3.72326582987361,-3.08681906241375));
#29330=CARTESIAN_POINT('Ctrl Pts',(35.3053653520941,4.74559492630417,-0.933000085434894));
#29331=CARTESIAN_POINT('Ctrl Pts',(35.424274351089,4.61473613786257,1.4475395476085));
#29332=CARTESIAN_POINT('Ctrl Pts',(35.543183350084,3.36248837950119,3.47632453342676));
#29333=CARTESIAN_POINT('Ctrl Pts',(35.662092349079,1.29315005136293,4.66035656453939));
#29334=CARTESIAN_POINT('Ctrl Pts',(35.7810013480739,-1.09042600580856,4.71191378208915));
#29335=CARTESIAN_POINT('Ctrl Pts',(35.8999103470689,-3.20902663233849,3.61846769184522));
#29336=CARTESIAN_POINT('Ctrl Pts',(36.0188193460638,-4.54782816263016,1.64572761026036));
#29337=CARTESIAN_POINT('Ctrl Pts',(36.1377283450588,-4.78149947825562,-0.726927165145562));
#29338=CARTESIAN_POINT('Ctrl Pts',(36.2566373440538,-3.85325803995349,-2.92293736530895));
#29339=CARTESIAN_POINT('Ctrl Pts',(36.3755463430487,-1.9886681441944,-4.40866866256147));
#29340=CARTESIAN_POINT('Ctrl Pts',(36.4944553420437,0.359171596216373,-4.82308574757461));
#29341=CARTESIAN_POINT('Ctrl Pts',(36.6133643410386,2.61973200921313,-4.06548454232559));
#29342=CARTESIAN_POINT('Ctrl Pts',(36.7322733400336,4.24369295226976,-2.31996346756645));
#29343=CARTESIAN_POINT('Ctrl Pts',(36.8511823390285,4.83642906984657,-0.0106872039015828));
#29344=CARTESIAN_POINT('Ctrl Pts',(36.9700913380235,4.25390444646255,2.3011860690411));
#29345=CARTESIAN_POINT('Ctrl Pts',(37.0890003370185,2.63767358661105,4.05386709383689));
#29346=CARTESIAN_POINT('Ctrl Pts',(37.2079093360135,0.380483422066699,4.82145130945858));
#29347=CARTESIAN_POINT('Ctrl Pts',(37.3268183350084,-1.96916488093114,4.41741440616232));
#29348=CARTESIAN_POINT('Ctrl Pts',(37.4457273340034,-3.84030266642664,2.93993805956863));
#29349=CARTESIAN_POINT('Ctrl Pts',(37.5646363329983,-4.77824017295507,0.748051611629016));
#29350=CARTESIAN_POINT('Ctrl Pts',(37.6835453319933,-4.55505694242569,-1.62561268920943));
#29351=CARTESIAN_POINT('Ctrl Pts',(37.8024543309882,-3.22498689113141,-3.60425025702862));
#29352=CARTESIAN_POINT('Ctrl Pts',(37.9213633299832,-1.11123937261475,-4.70704869562491));
#29353=CARTESIAN_POINT('Ctrl Pts',(38.0402723289781,1.27254126091167,-4.66602604989169));
#29354=CARTESIAN_POINT('Ctrl Pts',(38.1591813279731,3.34709213809732,-3.49115089786058));
#29355=CARTESIAN_POINT('Ctrl Pts',(38.2780903269681,4.60829375817302,-1.46791995430425));
#29356=CARTESIAN_POINT('Ctrl Pts',(38.396999325963,4.74967191984029,0.912018102494755));
#29357=CARTESIAN_POINT('Ctrl Pts',(38.515908324958,3.73687147615934,3.07033417888194));
#29358=CARTESIAN_POINT('Ctrl Pts',(38.634817323953,1.81600472180213,4.48255363434665));
#29359=CARTESIAN_POINT('Ctrl Pts',(38.7537263229479,-0.546154378463043,
4.80550476770034));
#29360=CARTESIAN_POINT('Ctrl Pts',(38.8726353219429,-2.77559697650641,3.9607096844851));
#29361=CARTESIAN_POINT('Ctrl Pts',(38.9915443209379,-4.33056470620339,2.15345547569111));
#29362=CARTESIAN_POINT('Ctrl Pts',(39.1104533199328,-4.83319749856621,-0.17709272655029));
#29363=CARTESIAN_POINT('Ctrl Pts',(39.2293623189278,-4.16135507364998,-2.46460601151995));
#29364=CARTESIAN_POINT('Ctrl Pts',(39.3482713179228,-2.47829558082605,-4.15321785953489));
#29365=CARTESIAN_POINT('Ctrl Pts',(39.4671803169177,-0.193006898275515,
-4.83258621084879));
#29366=CARTESIAN_POINT('Ctrl Pts',(39.5860893159127,2.13918475471825,-4.33763617745607));
#29367=CARTESIAN_POINT('Ctrl Pts',(39.7049983149076,3.95154686023701,-2.78861592032275));
#29368=CARTESIAN_POINT('Ctrl Pts',(39.8239073139026,4.80368393985005,-0.561991087425867));
#29369=CARTESIAN_POINT('Ctrl Pts',(39.9428163128975,4.48850186438168,1.80126636791584));
#29370=CARTESIAN_POINT('Ctrl Pts',(40.0617253118926,3.08263697266631,3.72667764760597));
#29371=CARTESIAN_POINT('Ctrl Pts',(40.1806343108874,0.927624029768742,4.74676968017454));
#29372=CARTESIAN_POINT('Ctrl Pts',(40.2995433098825,-1.45267973830484,4.612849709944));
#29373=CARTESIAN_POINT('Ctrl Pts',(40.4184523088774,-3.48022609014271,3.35907396628158));
#29374=CARTESIAN_POINT('Ctrl Pts',(40.5373613078724,-4.66157992956727,1.28689284996747));
#29375=CARTESIAN_POINT('Ctrl Pts',(40.6562703068673,-4.71114240206199,-1.09372738803408));
#29376=CARTESIAN_POINT('Ctrl Pts',(40.7751793058623,-3.61393126835275,-3.21709376641143));
#29377=CARTESIAN_POINT('Ctrl Pts',(40.8940883048572,-1.64244639784748,-4.5418482715989));
#29378=CARTESIAN_POINT('Ctrl Pts',(41.0526336368505,1.52894407634182,-4.87830053372444));
#29379=CARTESIAN_POINT('Ctrl Pts',(41.2508153018422,4.99877843246716,-2.25841953589028));
#29380=CARTESIAN_POINT('Ctrl Pts',(41.488633299832,4.60241792036846,2.98429118942186));
#29381=CARTESIAN_POINT('Ctrl Pts',(41.6868149648237,0.778136914097525,5.0527209529951));
#29382=CARTESIAN_POINT('Ctrl Pts',(41.8453602968169,-2.30662225456386,4.24328995789574));
#29383=CARTESIAN_POINT('Ctrl Pts',(41.9642692958119,-4.05652806066456,2.63719009692172));
#29384=CARTESIAN_POINT('Ctrl Pts',(42.0831782948068,-4.8220301182078,0.372998486510622));
#29385=CARTESIAN_POINT('Ctrl Pts',(42.2020872938019,-4.41511642611984,-1.97311114508245));
#29386=CARTESIAN_POINT('Ctrl Pts',(42.3209962927967,-2.93564809227475,-3.84412822728174));
#29387=CARTESIAN_POINT('Ctrl Pts',(42.4399052917918,-0.742648657028073,
-4.77882138616062));
#29388=CARTESIAN_POINT('Ctrl Pts',(42.5588142907866,1.63073378640869,-4.55335217780196));
#29389=CARTESIAN_POINT('Ctrl Pts',(42.6777232897817,3.60788611488371,-3.22085932267223));
#29390=CARTESIAN_POINT('Ctrl Pts',(42.7966322887766,4.70829521929217,-1.10596819245989));
#29391=CARTESIAN_POINT('Ctrl Pts',(42.9155412877716,4.66459064421329,1.27781356161113));
#29392=CARTESIAN_POINT('Ctrl Pts',(43.0344502867665,3.48737719917427,3.35101501196365));
#29393=CARTESIAN_POINT('Ctrl Pts',(43.1533592857615,1.46272757210891,4.60994870606898));
#29394=CARTESIAN_POINT('Ctrl Pts',(43.2722682847565,-0.917368716687352,
4.74863936151306));
#29395=CARTESIAN_POINT('Ctrl Pts',(43.3911772837514,-3.07454214894444,3.73341106082168));
#29396=CARTESIAN_POINT('Ctrl Pts',(43.5100862827464,-4.48459677614081,1.810952952575));
#29397=CARTESIAN_POINT('Ctrl Pts',(43.6289952817414,-4.80488636303764,-0.551567704129478));
#29398=CARTESIAN_POINT('Ctrl Pts',(43.7479042807363,-3.95758022389326,-2.78005754110368));
#29399=CARTESIAN_POINT('Ctrl Pts',(43.8668132797313,-2.14857511271005,-4.33298797203599));
#29400=CARTESIAN_POINT('Ctrl Pts',(43.9857222787262,0.182537496183628,-4.83299500723848));
#29401=CARTESIAN_POINT('Ctrl Pts',(44.1046312777212,2.46929318387108,-4.15857564635895));
#29402=CARTESIAN_POINT('Ctrl Pts',(44.2235402767161,4.15600629469078,-2.47361518386237));
#29403=CARTESIAN_POINT('Ctrl Pts',(44.3424492757112,4.83280259410293,-0.187561861340418));
#29404=CARTESIAN_POINT('Ctrl Pts',(44.461358274706,4.33521939121839,2.14406930481855));
#29405=CARTESIAN_POINT('Ctrl Pts',(44.580267273701,2.78417027841813,3.95468788064478));
#29406=CARTESIAN_POINT('Ctrl Pts',(44.699176272696,0.556562907717911,4.80431036557206));
#29407=CARTESIAN_POINT('Ctrl Pts',(44.818085271691,-1.80629022490289,4.48647701316453));
#29408=CARTESIAN_POINT('Ctrl Pts',(44.9369942706859,-3.73021166700226,3.07842188184474));
#29409=CARTESIAN_POINT('Ctrl Pts',(45.0559032696809,-4.74768513589875,0.922304838123059));
#29410=CARTESIAN_POINT('Ctrl Pts',(45.1748122686758,-4.61146279534857,-1.45793389809636));
#29411=CARTESIAN_POINT('Ctrl Pts',(45.2937212676708,-3.3546469128365,-3.48389214156527));
#29412=CARTESIAN_POINT('Ctrl Pts',(45.4126302666657,-1.28264595069628,-4.66325848835612));
#29413=CARTESIAN_POINT('Ctrl Pts',(45.5315392656608,1.10104022560684,-4.70944484897563));
#29414=CARTESIAN_POINT('Ctrl Pts',(45.6504482646557,3.21717169725219,-3.61122785689281));
#29415=CARTESIAN_POINT('Ctrl Pts',(45.7693572636507,4.55152480760976,-1.63547616604331));
#29416=CARTESIAN_POINT('Ctrl Pts',(45.8882662626456,4.77984941209146,0.737699099710084));
#29417=CARTESIAN_POINT('Ctrl Pts',(46.0071752616406,3.84666223161579,2.93161219124352));
#29418=CARTESIAN_POINT('Ctrl Pts',(46.1260842606355,1.97872938666984,4.41313838195828));
#29419=CARTESIAN_POINT('Ctrl Pts',(46.2449932596306,-0.370038167429234,
4.82226421078643));
#29420=CARTESIAN_POINT('Ctrl Pts',(46.3639022586254,-2.62888579826341,4.05957138423185));
#29421=CARTESIAN_POINT('Ctrl Pts',(46.4828112576205,-4.24890957237392,2.31039559594774));
#29422=CARTESIAN_POINT('Ctrl Pts',(46.6017202566154,-4.83644087317617,-0.000210371667774191));
#29423=CARTESIAN_POINT('Ctrl Pts',(46.7206292556104,-4.24870856478734,-2.31076521859925));
#29424=CARTESIAN_POINT('Ctrl Pts',(46.8395382546053,-2.62853262828611,-4.05980006724723));
#29425=CARTESIAN_POINT('Ctrl Pts',(46.9584472536003,-0.369618655984746,
-4.82229638379199));
#29426=CARTESIAN_POINT('Ctrl Pts',(47.0773562525952,1.97911329756526,-4.41296622685759));
#29427=CARTESIAN_POINT('Ctrl Pts',(47.1962652515902,3.84691725094163,-2.9312775420272));
#29428=CARTESIAN_POINT('Ctrl Pts',(47.3151742505852,4.77991356970463,-0.737283276725339));
#29429=CARTESIAN_POINT('Ctrl Pts',(47.4340832495801,4.55138251309761,1.6358721170845));
#29430=CARTESIAN_POINT('Ctrl Pts',(47.552992248575,3.21685752843096,3.61150771918909));
#29431=CARTESIAN_POINT('Ctrl Pts',(47.6719012475701,1.10063052605007,4.70954061550722));
#29432=CARTESIAN_POINT('Ctrl Pts',(47.7908102465649,-1.28305162327693,4.66314688767058));
#29433=CARTESIAN_POINT('Ctrl Pts',(47.9097192455601,-3.35494997929547,3.48360029285948));
#29434=CARTESIAN_POINT('Ctrl Pts',(48.0286282445548,-4.61158960999993,1.45753272104811));
#29435=CARTESIAN_POINT('Ctrl Pts',(48.1475372435499,-4.7476048825703,-0.922717856649593));
#29436=CARTESIAN_POINT('Ctrl Pts',(48.2664462425448,-3.72994384737292,-3.07874637789965));
#29437=CARTESIAN_POINT('Ctrl Pts',(48.3853552415398,-1.80589991965302,-4.48663413308713));
#29438=CARTESIAN_POINT('Ctrl Pts',(48.5042642405348,0.556980853810344,-4.80426193004442));
#29439=CARTESIAN_POINT('Ctrl Pts',(48.6231732395297,2.7845143035568,-3.95444565739282));
#29440=CARTESIAN_POINT('Ctrl Pts',(48.7420822385247,4.33540589701746,-2.14369215889122));
#29441=CARTESIAN_POINT('Ctrl Pts',(48.8609912375196,4.83278625867614,0.187982291549743));
#29442=CARTESIAN_POINT('Ctrl Pts',(48.9799002365146,4.15579108887287,2.47397671566045));
#29443=CARTESIAN_POINT('Ctrl Pts',(49.0988092355096,2.46893140046422,4.1587904616352));
#29444=CARTESIAN_POINT('Ctrl Pts',(49.2177182345045,0.182117054355301,4.8330108361658));
#29445=CARTESIAN_POINT('Ctrl Pts',(49.3366272334995,-2.14895205516562,4.33280110651177));
#29446=CARTESIAN_POINT('Ctrl Pts',(49.4555362324944,-3.95782204873261,2.77971311371218));
#29447=CARTESIAN_POINT('Ctrl Pts',(49.5744452314894,-4.80493434743749,0.551149962178289));
#29448=CARTESIAN_POINT('Ctrl Pts',(49.6933542304843,-4.48443917792565,-1.81134359619393));
#29449=CARTESIAN_POINT('Ctrl Pts',(49.8122632294794,-3.07421742814054,-3.73367748586597));
#29450=CARTESIAN_POINT('Ctrl Pts',(49.9311722284743,-0.91695545501133,-4.74872120234939));
#29451=CARTESIAN_POINT('Ctrl Pts',(50.0500812274693,1.46312830084543,-4.60981734333861));
#29452=CARTESIAN_POINT('Ctrl Pts',(50.1689902264642,3.48766931516144,-3.35071979022551));
#29453=CARTESIAN_POINT('Ctrl Pts',(50.2878992254592,4.66470057283824,-1.2773914549038));
#29454=CARTESIAN_POINT('Ctrl Pts',(50.4068082244542,4.70820141549651,1.1063452423862));
#29455=CARTESIAN_POINT('Ctrl Pts',(50.5257172234491,3.60760106160095,3.2212381076511));
#29456=CARTESIAN_POINT('Ctrl Pts',(50.6446262224441,1.63034732725642,4.55336446476378));
#29457=CARTESIAN_POINT('Ctrl Pts',(50.763535221439,-0.743083666570843,4.77901528009773));
#29458=CARTESIAN_POINT('Ctrl Pts',(50.882444220434,-2.93594402421914,3.84335699801001));
#29459=CARTESIAN_POINT('Ctrl Pts',(51.001353219429,-4.41536484357523,1.97375624497553));
#29460=CARTESIAN_POINT('Ctrl Pts',(51.1202622184239,-4.82184425593253,-0.375470766917604));
#29461=CARTESIAN_POINT('Ctrl Pts',(51.2391712174189,-4.05660708469425,-2.6334576607887));
#29462=CARTESIAN_POINT('Ctrl Pts',(51.3580802164138,-2.30560723776937,-4.25150985415276));
#29463=CARTESIAN_POINT('Ctrl Pts',(51.4769892154088,0.00565912138068442,
-4.83643744812126));
#29464=CARTESIAN_POINT('Ctrl Pts',(51.5958982144037,2.31555047906077,-4.2461027701313));
#29465=CARTESIAN_POINT('Ctrl Pts',(51.7148072133987,4.06275866270233,-2.62395666916879));
#29466=CARTESIAN_POINT('Ctrl Pts',(51.8337162123937,4.82271006688757,-0.364186508865252));
#29467=CARTESIAN_POINT('Ctrl Pts',(51.9526252113887,4.41073308205851,1.98408562281516));
#29468=CARTESIAN_POINT('Ctrl Pts',(52.0715342103836,2.92694300060758,3.85021346641923));
#29469=CARTESIAN_POINT('Ctrl Pts',(52.1904432093786,0.731895106392164,4.78074866041095));
#29470=CARTESIAN_POINT('Ctrl Pts',(52.3093522083735,-1.64099354029295,4.54952168184252));
#29471=CARTESIAN_POINT('Ctrl Pts',(52.4282612073685,-3.61513991179064,3.21281655827632));
#29472=CARTESIAN_POINT('Ctrl Pts',(52.5471702063634,-4.71075698457868,1.09526436882405));
#29473=CARTESIAN_POINT('Ctrl Pts',(52.6660792053584,-4.66173961615656,-1.28818408548258));
#29474=CARTESIAN_POINT('Ctrl Pts',(52.7849882043534,-3.47973538673397,-3.35912771293794));
#29475=CARTESIAN_POINT('Ctrl Pts',(52.86426087035,-2.12824042603024,-4.1946696959942));
#29476=CARTESIAN_POINT('Ctrl Pts',(52.9038972033484,-1.39339708167545,-4.42601302158306));
#29477=CARTESIAN_POINT('Ctrl Pts',(30.,-2.16839587231052,4.42195480991684));
#29478=CARTESIAN_POINT('Ctrl Pts',(30.0396363329983,-2.90256543874863,4.06193976546858));
#29479=CARTESIAN_POINT('Ctrl Pts',(30.118908998995,-4.1873856238303,2.96952538142736));
#29480=CARTESIAN_POINT('Ctrl Pts',(30.2378179979899,-5.0972178887381,0.607825460320724));
#29481=CARTESIAN_POINT('Ctrl Pts',(30.3567269969849,-4.7683165925989,-1.90099691957731));
#29482=CARTESIAN_POINT('Ctrl Pts',(30.4756359959799,-3.28075742325608,-3.94815518873056));
#29483=CARTESIAN_POINT('Ctrl Pts',(30.5945449949748,-0.995942585346445,
-5.03576453627197));
#29484=CARTESIAN_POINT('Ctrl Pts',(30.7134539939698,1.53087507705621,-4.89974452521287));
#29485=CARTESIAN_POINT('Ctrl Pts',(30.8323629929647,3.68569391285887,-3.57304280422193));
#29486=CARTESIAN_POINT('Ctrl Pts',(30.9512719919597,4.94487940999554,-1.37810306103397));
#29487=CARTESIAN_POINT('Ctrl Pts',(31.0701809909546,5.00245217612307,1.15172698288151));
#29488=CARTESIAN_POINT('Ctrl Pts',(31.1890899899496,3.8444194772201,3.40168092026129));
#29489=CARTESIAN_POINT('Ctrl Pts',(31.3079989889446,1.75218651717396,4.82502265243806));
#29490=CARTESIAN_POINT('Ctrl Pts',(31.4269079879395,-0.765831043184473,
5.07587431015258));
#29491=CARTESIAN_POINT('Ctrl Pts',(31.5458169869345,-3.0977502147508,4.09328017158535));
#29492=CARTESIAN_POINT('Ctrl Pts',(31.6647259859294,-4.6769107062099,2.11601149734983));
#29493=CARTESIAN_POINT('Ctrl Pts',(31.7836349849244,-5.11957367279555,-0.375451539463316));
#29494=CARTESIAN_POINT('Ctrl Pts',(31.9025439839194,-4.31817127659016,-2.77567926432736));
#29495=CARTESIAN_POINT('Ctrl Pts',(32.0214529829144,-2.46744568505685,-4.5014120277379));
#29496=CARTESIAN_POINT('Ctrl Pts',(32.1403619819093,-0.0171264705275148,
-5.1332937962503));
#29497=CARTESIAN_POINT('Ctrl Pts',(32.2592709809043,2.43735450799018,-4.51777616612193));
#29498=CARTESIAN_POINT('Ctrl Pts',(32.3781799798992,4.29955406820673,-2.80443101358115));
#29499=CARTESIAN_POINT('Ctrl Pts',(32.4970889788942,5.11695445427107,-0.409604207090211));
#29500=CARTESIAN_POINT('Ctrl Pts',(32.6159979778891,4.69092593906626,2.08475713853971));
#29501=CARTESIAN_POINT('Ctrl Pts',(32.7349069768841,3.12499419881144,4.07251884603082));
#29502=CARTESIAN_POINT('Ctrl Pts',(32.8538159758791,0.799683390900607,5.07065133560223));
#29503=CARTESIAN_POINT('Ctrl Pts',(32.9727249748741,-1.71995188260795,4.83660666324366));
#29504=CARTESIAN_POINT('Ctrl Pts',(33.091633973869,-3.82163583403228,3.42725809434683));
#29505=CARTESIAN_POINT('Ctrl Pts',(33.210542972864,-4.99465557945741,1.18507980147653));
#29506=CARTESIAN_POINT('Ctrl Pts',(33.3294519718589,-4.95396526475957,-1.34507496030352));
#29507=CARTESIAN_POINT('Ctrl Pts',(33.4483609708539,-3.70945270772488,-3.54837414915822));
#29508=CARTESIAN_POINT('Ctrl Pts',(33.5672699698489,-1.56353664101852,-4.88941220040492));
#29509=CARTESIAN_POINT('Ctrl Pts',(33.6861789688438,0.962321569924411,-5.0423145170969));
#29510=CARTESIAN_POINT('Ctrl Pts',(33.8050879678388,3.2543339526788,-3.9699255682838));
#29511=CARTESIAN_POINT('Ctrl Pts',(33.9239969668337,4.75553748094053,-1.93283774814137));
#29512=CARTESIAN_POINT('Ctrl Pts',(34.0429059658287,5.10113706612673,0.573933032555513));
#29513=CARTESIAN_POINT('Ctrl Pts',(34.1618149648236,4.20715140329205,2.94123708038784));
#29514=CARTESIAN_POINT('Ctrl Pts',(34.2807239638186,2.29082057542709,4.59381536247054));
#29515=CARTESIAN_POINT('Ctrl Pts',(34.3996329628136,-0.182183667472828,
5.13008845972237));
#29516=CARTESIAN_POINT('Ctrl Pts',(34.5185419618085,-2.61091695985679,4.41974106956536));
#29517=CARTESIAN_POINT('Ctrl Pts',(34.6374509608035,-4.40519285474456,2.63538885285986));
#29518=CARTESIAN_POINT('Ctrl Pts',(34.7563599597985,-5.1289991647845,0.210632525765634));
#29519=CARTESIAN_POINT('Ctrl Pts',(34.8752689587934,-4.60644968799474,-2.26530787427308));
#29520=CARTESIAN_POINT('Ctrl Pts',(34.9941779577884,-2.96452486312706,-4.19077449037431));
#29521=CARTESIAN_POINT('Ctrl Pts',(35.1130869567833,-0.602215300486822,
-5.09787555998869));
#29522=CARTESIAN_POINT('Ctrl Pts',(35.2319959557783,1.90643363569679,-4.76618393329028));
#29523=CARTESIAN_POINT('Ctrl Pts',(35.3509049547733,3.95181585692917,-3.27630125693498));
#29524=CARTESIAN_POINT('Ctrl Pts',(35.4698139537682,5.03689989843353,-0.990271632649752));
#29525=CARTESIAN_POINT('Ctrl Pts',(35.5887229527632,4.89800843625729,1.53639573405519));
#29526=CARTESIAN_POINT('Ctrl Pts',(35.7076319517581,3.56889233914948,3.68971624448692));
#29527=CARTESIAN_POINT('Ctrl Pts',(35.8265409507531,1.37252914829839,4.94642924040584));
#29528=CARTESIAN_POINT('Ctrl Pts',(35.9454499497481,-1.15736103127196,5.00115126111614));
#29529=CARTESIAN_POINT('Ctrl Pts',(36.064358948743,-3.40601045169361,3.84058475967195));
#29530=CARTESIAN_POINT('Ctrl Pts',(36.183267947738,-4.82699336251288,1.7467494300921));
#29531=CARTESIAN_POINT('Ctrl Pts',(36.3021769467329,-5.07500842579123,-0.771549072592608));
#29532=CARTESIAN_POINT('Ctrl Pts',(36.421085945728,-4.08978754644683,-3.10235979831467));
#29533=CARTESIAN_POINT('Ctrl Pts',(36.5399949447229,-2.11074112499353,-4.67929165542513));
#29534=CARTESIAN_POINT('Ctrl Pts',(36.6589039437178,0.381219089407465,-5.11914743869939));
#29535=CARTESIAN_POINT('Ctrl Pts',(36.7778129427128,2.78054239690555,-4.31504142184985));
#29536=CARTESIAN_POINT('Ctrl Pts',(36.8967219417078,4.50418902839594,-2.46237277635822));
#29537=CARTESIAN_POINT('Ctrl Pts',(37.0156309407027,5.13330983132668,-0.0113432303183229));
#29538=CARTESIAN_POINT('Ctrl Pts',(37.1345399396977,4.51502734790305,2.44244274056837));
#29539=CARTESIAN_POINT('Ctrl Pts',(37.2534489386926,2.79958530528203,4.3027108445415));
#29540=CARTESIAN_POINT('Ctrl Pts',(37.3723579376876,0.403839126542568,5.11741267176111));
#29541=CARTESIAN_POINT('Ctrl Pts',(37.4912669366826,-2.09004066777468,4.68857425028185));
#29542=CARTESIAN_POINT('Ctrl Pts',(37.6101759356776,-4.07603691652264,3.12040406811011));
#29543=CARTESIAN_POINT('Ctrl Pts',(37.7290849346725,-5.071549050351,0.793970228211562));
#29544=CARTESIAN_POINT('Ctrl Pts',(37.8479939336675,-4.83466587581909,-1.72539976890694));
#29545=CARTESIAN_POINT('Ctrl Pts',(37.9669029326624,-3.42295041963053,-3.82549459772262));
#29546=CARTESIAN_POINT('Ctrl Pts',(38.0858119316574,-1.17945201180872,-4.99598753477663));
#29547=CARTESIAN_POINT('Ctrl Pts',(38.2047209306523,1.35065530189071,-4.95244674308752));
#29548=CARTESIAN_POINT('Ctrl Pts',(38.3236299296473,3.55255101040822,-3.7054527147653));
#29549=CARTESIAN_POINT('Ctrl Pts',(38.4425389286423,4.89117059566871,-1.55802717753281));
#29550=CARTESIAN_POINT('Ctrl Pts',(38.5614479276372,5.0412271553206,0.968001685597478));
#29551=CARTESIAN_POINT('Ctrl Pts',(38.6803569266322,3.96625667614341,3.25880446054239));
#29552=CARTESIAN_POINT('Ctrl Pts',(38.7992659256271,1.9274788811197,4.75771200369754));
#29553=CARTESIAN_POINT('Ctrl Pts',(38.9181749246221,-0.57967967686442,5.10048726286934));
#29554=CARTESIAN_POINT('Ctrl Pts',(39.0370839236171,-2.94597502445185,4.20383503381829));
#29555=CARTESIAN_POINT('Ctrl Pts',(39.1559929226121,-4.59639334321001,2.28564380972928));
#29556=CARTESIAN_POINT('Ctrl Pts',(39.274901921607,-5.12987989233977,-0.18796343771993));
#29557=CARTESIAN_POINT('Ctrl Pts',(39.393810920602,-4.41679689760991,-2.6158941000831));
#29558=CARTESIAN_POINT('Ctrl Pts',(39.5127199195969,-2.63042399387271,-4.408160186389));
#29559=CARTESIAN_POINT('Ctrl Pts',(39.6316289185919,-0.204854489567262,
-5.12923108116021));
#29560=CARTESIAN_POINT('Ctrl Pts',(39.7505379175869,2.27049709069084,-4.60389889170027));
#29561=CARTESIAN_POINT('Ctrl Pts',(39.8694469165818,4.19410975611519,-2.95979312688258));
#29562=CARTESIAN_POINT('Ctrl Pts',(39.9883559155768,5.09855466479541,-0.596488510952733));
#29563=CARTESIAN_POINT('Ctrl Pts',(40.1072649145717,4.76402536160622,1.91183582385376));
#29564=CARTESIAN_POINT('Ctrl Pts',(40.2261739135667,3.27186245258037,3.95543710666844));
#29565=CARTESIAN_POINT('Ctrl Pts',(40.3450829125616,0.984565571626985,5.03814676373541));
#29566=CARTESIAN_POINT('Ctrl Pts',(40.4639919115567,-1.54185145170459,4.89600621130151));
#29567=CARTESIAN_POINT('Ctrl Pts',(40.5829009105515,-3.69385729548926,3.56526833460081));
#29568=CARTESIAN_POINT('Ctrl Pts',(40.7018099095466,-4.94772770082657,1.3658878530419));
#29569=CARTESIAN_POINT('Ctrl Pts',(40.8207189085415,-5.0003325304742,-1.16086506649928));
#29570=CARTESIAN_POINT('Ctrl Pts',(40.9396279075364,-3.83576987104716,-3.41457278105877));
#29571=CARTESIAN_POINT('Ctrl Pts',(41.0585369065314,-1.74326680278702,-4.82064640012023));
#29572=CARTESIAN_POINT('Ctrl Pts',(41.2170822385247,1.62279722193528,-5.17775154525906));
#29573=CARTESIAN_POINT('Ctrl Pts',(41.4152639035163,5.30562489419936,-2.39705101417185));
#29574=CARTESIAN_POINT('Ctrl Pts',(41.6530819015062,4.88493407373615,3.16747978332012));
#29575=CARTESIAN_POINT('Ctrl Pts',(41.8512635664978,0.825902295592203,5.36287863801606));
#29576=CARTESIAN_POINT('Ctrl Pts',(42.0098088984911,-2.44821262247626,4.50376129649866));
#29577=CARTESIAN_POINT('Ctrl Pts',(42.1287178974861,-4.30553515292689,2.79907213692171));
#29578=CARTESIAN_POINT('Ctrl Pts',(42.247626896481,-5.11802701027407,0.395894733536493));
#29579=CARTESIAN_POINT('Ctrl Pts',(42.366535895476,-4.6861352103675,-2.09422917054652));
#29580=CARTESIAN_POINT('Ctrl Pts',(42.485444894471,-3.11585076422253,-4.08009730671223));
#29581=CARTESIAN_POINT('Ctrl Pts',(42.6043538934659,-0.788235617082007,
-5.07216594091614));
#29582=CARTESIAN_POINT('Ctrl Pts',(42.7232628924609,1.73083522101851,-4.83285646543042));
#29583=CARTESIAN_POINT('Ctrl Pts',(42.8421718914558,3.82935364012834,-3.41856948331472));
#29584=CARTESIAN_POINT('Ctrl Pts',(42.9610808904508,4.99731057541337,-1.17385726400598));
#29585=CARTESIAN_POINT('Ctrl Pts',(43.0799898894458,4.9509232260516,1.35625123902188));
#29586=CARTESIAN_POINT('Ctrl Pts',(43.1988988884407,3.70144737026687,3.55671468709909));
#29587=CARTESIAN_POINT('Ctrl Pts',(43.3178078874357,1.55251606464634,4.89292713136518));
#29588=CARTESIAN_POINT('Ctrl Pts',(43.4367168864306,-0.973680743439912,
5.04013121413423));
#29589=CARTESIAN_POINT('Ctrl Pts',(43.5556258854256,-3.26327073385682,3.96258384566937));
#29590=CARTESIAN_POINT('Ctrl Pts',(43.6745348844206,-4.7598805622988,1.92211701262856));
#29591=CARTESIAN_POINT('Ctrl Pts',(43.7934438834155,-5.09983089787587,-0.58542529567995));
#29592=CARTESIAN_POINT('Ctrl Pts',(43.9123528824105,-4.20051347351195,-2.95070939763705));
#29593=CARTESIAN_POINT('Ctrl Pts',(44.0312618814054,-2.28046386913482,-4.59896535949367));
#29594=CARTESIAN_POINT('Ctrl Pts',(44.1501708804004,0.193742430667919,-5.12966497122579));
#29595=CARTESIAN_POINT('Ctrl Pts',(44.2690798793954,2.62086899117812,-4.41384685714979));
#29596=CARTESIAN_POINT('Ctrl Pts',(44.3879888783903,4.41111978765533,-2.62545629406751));
#29597=CARTESIAN_POINT('Ctrl Pts',(44.5068978773853,5.12946074694665,-0.199075212909377));
#29598=CARTESIAN_POINT('Ctrl Pts',(44.6258068763802,4.60133375275685,2.27568147542788));
#29599=CARTESIAN_POINT('Ctrl Pts',(44.7447158753752,2.9550745924089,4.19744358582857));
#29600=CARTESIAN_POINT('Ctrl Pts',(44.8636248743702,0.590727126290896,5.09921954321519));
#29601=CARTESIAN_POINT('Ctrl Pts',(44.9825338733651,-1.91716806673179,4.76187621633605));
#29602=CARTESIAN_POINT('Ctrl Pts',(45.1014428723601,-3.95918805933394,3.26738862140414));
#29603=CARTESIAN_POINT('Ctrl Pts',(45.220351871355,-5.03911841405869,0.978919865182178));
#29604=CARTESIAN_POINT('Ctrl Pts',(45.3392608703501,-4.89453416193924,-1.54742813436108));
#29605=CARTESIAN_POINT('Ctrl Pts',(45.458169869345,-3.56056952962606,-3.69774838487314));
#29606=CARTESIAN_POINT('Ctrl Pts',(45.5770788683399,-1.36138026087697,-4.94950929675383));
#29607=CARTESIAN_POINT('Ctrl Pts',(45.6959878673349,1.16862679740963,-4.99853077429798));
#29608=CARTESIAN_POINT('Ctrl Pts',(45.8148968663299,3.41465549562881,-3.83290051259592));
#29609=CARTESIAN_POINT('Ctrl Pts',(45.9338058653249,4.83091692341755,-1.7358687082569));
#29610=CARTESIAN_POINT('Ctrl Pts',(46.0527148643198,5.0732570714882,0.782982234705375));
#29611=CARTESIAN_POINT('Ctrl Pts',(46.1716238633147,4.08278685910157,3.11156712227454));
#29612=CARTESIAN_POINT('Ctrl Pts',(46.2905328623098,2.10019228390124,4.68403574537074));
#29613=CARTESIAN_POINT('Ctrl Pts',(46.4094418613047,-0.392752697371978,
5.11827547245928));
#29614=CARTESIAN_POINT('Ctrl Pts',(46.5283508602997,-2.79025808479161,4.30876528874866));
#29615=CARTESIAN_POINT('Ctrl Pts',(46.6472598592946,-4.50972586701803,2.45221758773953));
#29616=CARTESIAN_POINT('Ctrl Pts',(46.7661688582895,-5.13332235919528,-0.000223285183078947));
#29617=CARTESIAN_POINT('Ctrl Pts',(46.8850778572845,-4.50951252072361,-2.4526098994148));
#29618=CARTESIAN_POINT('Ctrl Pts',(47.0039868562795,-2.78988323572627,-4.30900800930841));
#29619=CARTESIAN_POINT('Ctrl Pts',(47.1228958552744,-0.392307434515635,
-5.11830962038193));
#29620=CARTESIAN_POINT('Ctrl Pts',(47.2418048542694,2.10059976089411,-4.68385302265156));
#29621=CARTESIAN_POINT('Ctrl Pts',(47.3607138532644,4.08305753260748,-3.11121193085393));
#29622=CARTESIAN_POINT('Ctrl Pts',(47.4796228522593,5.07332516737085,-0.782540886722258));
#29623=CARTESIAN_POINT('Ctrl Pts',(47.5985318512543,4.83076589425792,1.73628896447134));
#29624=CARTESIAN_POINT('Ctrl Pts',(47.7174408502492,3.41432204177779,3.83319755404034));
#29625=CARTESIAN_POINT('Ctrl Pts',(47.8363498492442,1.16819194873676,4.99863241939004));
#29626=CARTESIAN_POINT('Ctrl Pts',(47.9552588482392,-1.36181083538065,4.94939084553952));
#29627=CARTESIAN_POINT('Ctrl Pts',(48.0741678472341,-3.56089119960421,3.69743862124198));
#29628=CARTESIAN_POINT('Ctrl Pts',(48.1930768462291,-4.89466876101785,1.54700233134486));
#29629=CARTESIAN_POINT('Ctrl Pts',(48.311985845224,-5.03903323443671,-0.979358236557413));
#29630=CARTESIAN_POINT('Ctrl Pts',(48.4308948442191,-3.95890379978701,-3.26773303641874));
#29631=CARTESIAN_POINT('Ctrl Pts',(48.549803843214,-1.91675380287157,-4.76204298095343));
#29632=CARTESIAN_POINT('Ctrl Pts',(48.6687128422089,0.591170727707161,-5.09916813450712));
#29633=CARTESIAN_POINT('Ctrl Pts',(48.787621841204,2.9554397352862,-4.19718649387443));
#29634=CARTESIAN_POINT('Ctrl Pts',(48.9065308401988,4.60153170708184,-2.27528117866585));
#29635=CARTESIAN_POINT('Ctrl Pts',(49.0254398391939,5.12944340878129,0.19952145092828));
#29636=CARTESIAN_POINT('Ctrl Pts',(49.1443488381888,4.41089137158125,2.62584001823806));
#29637=CARTESIAN_POINT('Ctrl Pts',(49.2632578371838,2.62048499995396,4.4140748587091));
#29638=CARTESIAN_POINT('Ctrl Pts',(49.3821668361788,0.193296180316791,5.12968177180056));
#29639=CARTESIAN_POINT('Ctrl Pts',(49.5010758351737,-2.28086394993512,4.59876702336206));
#29640=CARTESIAN_POINT('Ctrl Pts',(49.6199848341686,-4.20077014259718,2.95034382781493));
#29641=CARTESIAN_POINT('Ctrl Pts',(49.7388938331637,-5.09988182776401,0.584981910935992));
#29642=CARTESIAN_POINT('Ctrl Pts',(49.8578028321585,-4.75971329002921,-1.92253163562839));
#29643=CARTESIAN_POINT('Ctrl Pts',(49.9767118311536,-3.26292608029717,-3.96286662502565));
#29644=CARTESIAN_POINT('Ctrl Pts',(50.0956208301484,-0.973242113989631,
-5.04021807871213));
#29645=CARTESIAN_POINT('Ctrl Pts',(50.2145298291435,1.55294139183154,-4.89278770502699));
#29646=CARTESIAN_POINT('Ctrl Pts',(50.3334388281384,3.7017574175863,-3.55640134338437));
#29647=CARTESIAN_POINT('Ctrl Pts',(50.4523478271334,4.95103990256707,-1.35580322159434));
#29648=CARTESIAN_POINT('Ctrl Pts',(50.5712568261284,4.99721101353838,1.17425745887403));
#29649=CARTESIAN_POINT('Ctrl Pts',(50.6901658251233,3.82905108905242,3.41897151974029));
#29650=CARTESIAN_POINT('Ctrl Pts',(50.8090748241183,1.73042503934585,4.83286950661864));
#29651=CARTESIAN_POINT('Ctrl Pts',(50.9279838231132,-0.78869732937638,5.07237173689479));
#29652=CARTESIAN_POINT('Ctrl Pts',(51.0468928221082,-3.11616486173899,4.07927873607974));
#29653=CARTESIAN_POINT('Ctrl Pts',(51.1658018211031,-4.68639887675184,2.09491386943815));
#29654=CARTESIAN_POINT('Ctrl Pts',(51.2847108200981,-5.11782973897512,-0.398518773119308));
#29655=CARTESIAN_POINT('Ctrl Pts',(51.403619819093,-4.3056190277905,-2.79511058784905));
#29656=CARTESIAN_POINT('Ctrl Pts',(51.522528818088,-2.44713529959719,-4.51248576524599));
#29657=CARTESIAN_POINT('Ctrl Pts',(51.641437817083,0.00600650252500089,
-5.13331872389581));
#29658=CARTESIAN_POINT('Ctrl Pts',(51.7603468160779,2.45768889968914,-4.5067467712144));
#29659=CARTESIAN_POINT('Ctrl Pts',(51.879255815073,4.312148216043,-2.7850263846104));
#29660=CARTESIAN_POINT('Ctrl Pts',(51.9981648140678,5.11874869712036,-0.386541838905528));
#29661=CARTESIAN_POINT('Ctrl Pts',(52.1170738130629,4.68148279784595,2.10587730879592));
#29662=CARTESIAN_POINT('Ctrl Pts',(52.2359828120578,3.10661131668958,4.08655608392974));
#29663=CARTESIAN_POINT('Ctrl Pts',(52.3548918110528,0.776821967382241,5.07421151952673));
#29664=CARTESIAN_POINT('Ctrl Pts',(52.4738008100477,-1.74172476260393,4.82879083719861));
#29665=CARTESIAN_POINT('Ctrl Pts',(52.5927098090427,-3.83705270620355,3.41003301954189));
#29666=CARTESIAN_POINT('Ctrl Pts',(52.7116188080376,-4.99992345441255,1.16249639376284));
#29667=CARTESIAN_POINT('Ctrl Pts',(52.8305278070326,-4.94789718966368,-1.36725835013145));
#29668=CARTESIAN_POINT('Ctrl Pts',(52.9494368060275,-3.69333647060053,-3.56532538045744));
#29669=CARTESIAN_POINT('Ctrl Pts',(53.0287094720242,-2.25888095216386,-4.45215651437191));
#29670=CARTESIAN_POINT('Ctrl Pts',(53.0683458050225,-1.47892977132682,-4.69770068559963));
#29671=CARTESIAN_POINT('Ctrl Pts',(51.2661584740964,-4.92519062564324,-0.000109311139069327));
#29672=CARTESIAN_POINT('Ctrl Pts',(51.2723425894303,-4.92531381623605,-0.127669621319975));
#29673=CARTESIAN_POINT('Ctrl Pts',(51.2785267047642,-4.92045777626379,-0.255220575265934));
#29674=CARTESIAN_POINT('Ctrl Pts',(51.2847108200981,-4.91055614340714,-0.382378635148));
#29675=CARTESIAN_POINT('Ctrl Pts',(51.3243471530964,-4.84709283524692,-1.19738271136255));
#29676=CARTESIAN_POINT('Ctrl Pts',(51.3639834860947,-4.57635593151871,-1.99624664960581));
#29677=CARTESIAN_POINT('Ctrl Pts',(51.4036198190931,-4.13124019162237,-2.68190781496027));
#29678=CARTESIAN_POINT('Ctrl Pts',(51.4432561520914,-3.68612445172606,-3.3675689803147));
#29679=CARTESIAN_POINT('Ctrl Pts',(51.4828924850897,-3.0666298756616,-3.94002737278036));
#29680=CARTESIAN_POINT('Ctrl Pts',(51.522528818088,-2.34802562060904,-4.32972872878814));
#29681=CARTESIAN_POINT('Ctrl Pts',(51.5621651510864,-1.62942136555644,-4.71943008479595));
#29682=CARTESIAN_POINT('Ctrl Pts',(51.6018014840847,-0.811707431515759,
-4.92637440434587));
#29683=CARTESIAN_POINT('Ctrl Pts',(51.641437817083,0.0057632683653263,-4.92541790534061));
#29684=CARTESIAN_POINT('Ctrl Pts',(51.6810741500813,0.823233968246388,-4.92446140633534));
#29685=CARTESIAN_POINT('Ctrl Pts',(51.7207104830796,1.64046143396783,-4.71560408877485));
#29686=CARTESIAN_POINT('Ctrl Pts',(51.7603468160779,2.35815171955416,-4.32422203222727));
#29687=CARTESIAN_POINT('Ctrl Pts',(51.7999831490763,3.07584200514046,-3.9328399756797));
#29688=CARTESIAN_POINT('Ctrl Pts',(51.8396194820746,3.69399511059172,-3.35893318014506));
#29689=CARTESIAN_POINT('Ctrl Pts',(51.8792558150729,4.13750507683024,-2.67223235809361));
#29690=CARTESIAN_POINT('Ctrl Pts',(51.9188921480713,4.58101504306879,-1.98553153604211));
#29691=CARTESIAN_POINT('Ctrl Pts',(51.9585284810695,4.84988187009458,-1.18603668747381));
#29692=CARTESIAN_POINT('Ctrl Pts',(51.9981648140678,4.9114376337284,-0.370886071906074));
#29693=CARTESIAN_POINT('Ctrl Pts',(52.0378011470662,4.97299339736222,0.444264543661619));
#29694=CARTESIAN_POINT('Ctrl Pts',(52.0774374800645,4.82723809760408,1.2750709262288));
#29695=CARTESIAN_POINT('Ctrl Pts',(52.1170738130628,4.49188186753229,2.02058724670132));
#29696=CARTESIAN_POINT('Ctrl Pts',(52.1567101460612,4.15652563746048,2.76610356717389));
#29697=CARTESIAN_POINT('Ctrl Pts',(52.1963464790595,3.63156847707506,3.42632982555178));
#29698=CARTESIAN_POINT('Ctrl Pts',(52.2359828120578,2.98079167199775,3.92105219400693));
#29699=CARTESIAN_POINT('Ctrl Pts',(52.2756191450561,2.33001486692049,4.41577456246206));
#29700=CARTESIAN_POINT('Ctrl Pts',(52.3152554780544,1.55341841715134,4.7449930409944));
#29701=CARTESIAN_POINT('Ctrl Pts',(52.3548918110528,0.745362403935769,4.86869883320588));
#29702=CARTESIAN_POINT('Ctrl Pts',(52.3945281440511,-0.0626936092798216,
4.99240462541736));
#29703=CARTESIAN_POINT('Ctrl Pts',(52.4341644770494,-0.90220918594187,4.91059773130798));
#29704=CARTESIAN_POINT('Ctrl Pts',(52.4738008100477,-1.67118829820617,4.63323464797717));
#29705=CARTESIAN_POINT('Ctrl Pts',(52.5075338733651,-2.32563887729704,4.39718086236812));
#29706=CARTESIAN_POINT('Ctrl Pts',(52.5412669366826,-2.92899917280827,4.01948372606978));
#29707=CARTESIAN_POINT('Ctrl Pts',(52.575,-3.4289504971169,3.53554284596617));
#29708=CARTESIAN_POINT('',(30.,-2.36248025497576,-3.31498400274172));
#29709=CARTESIAN_POINT('Ctrl Pts',(30.,-2.36248025497577,-3.31498400274171));
#29710=CARTESIAN_POINT('Ctrl Pts',(30.,-2.45083843615591,-3.26474897896515));
#29711=CARTESIAN_POINT('Ctrl Pts',(30.,-2.53718351659932,-3.21123764907035));
#29712=CARTESIAN_POINT('Ctrl Pts',(30.,-2.62132194611034,-3.1545569519088));
#29713=CARTESIAN_POINT('Ctrl Pts',(30.,-2.72544815198244,-3.0844112886736));
#29714=CARTESIAN_POINT('Ctrl Pts',(30.,-2.82619586363277,-3.00941311150835));
#29715=CARTESIAN_POINT('Ctrl Pts',(30.,-2.92335412828235,-2.92992006081671));
#29716=CARTESIAN_POINT('Ctrl Pts',(30.,-2.97900326879923,-2.88438898876629));
#29717=CARTESIAN_POINT('Ctrl Pts',(30.,-3.03347455648341,-2.83738236952648));
#29718=CARTESIAN_POINT('Ctrl Pts',(30.,-3.0867253031436,-2.78896042769935));
#29719=CARTESIAN_POINT('Ctrl Pts',(30.,-3.11397382321371,-2.76418281730958));
#29720=CARTESIAN_POINT('Ctrl Pts',(30.,-3.14090271699396,-2.73903454273245));
#29721=CARTESIAN_POINT('Ctrl Pts',(30.,-3.16750598172609,-2.71352320765771));
#29722=CARTESIAN_POINT('Ctrl Pts',(30.,-3.18459441442187,-2.69713616881892));
#29723=CARTESIAN_POINT('Ctrl Pts',(30.,-3.20154848687735,-2.68059932313958));
#29724=CARTESIAN_POINT('Ctrl Pts',(30.,-3.21836656153023,-2.6639146213908));
#29725=CARTESIAN_POINT('Ctrl Pts',(30.,-3.23304554999825,-2.64935204216473));
#29726=CARTESIAN_POINT('Ctrl Pts',(30.,-3.24761410550802,-2.63468359558042));
#29727=CARTESIAN_POINT('Ctrl Pts',(30.,-3.26207083845536,-2.61991145761989));
#29728=CARTESIAN_POINT('Ctrl Pts',(30.,-3.35252130085124,-2.52748762202905));
#29729=CARTESIAN_POINT('Ctrl Pts',(30.,-3.438603032295,-2.43100190270749));
#29730=CARTESIAN_POINT('Ctrl Pts',(30.,-3.52009387524001,-2.33082934687855));
#29731=CARTESIAN_POINT('Ctrl Pts',(30.,-3.6020913892008,-2.23003396609431));
#29732=CARTESIAN_POINT('Ctrl Pts',(30.,-3.67944139748576,-2.12550525076635));
#29733=CARTESIAN_POINT('Ctrl Pts',(30.,-3.75189019008547,-2.01758014367288));
#29734=CARTESIAN_POINT('Ctrl Pts',(30.,-3.77730845825652,-1.97971520188362));
#29735=CARTESIAN_POINT('Ctrl Pts',(30.,-3.80212313498671,-1.94143182393266));
#29736=CARTESIAN_POINT('Ctrl Pts',(30.,-3.82632224018495,-1.90274343853103));
#29737=CARTESIAN_POINT('Ctrl Pts',(30.,-3.84913245280764,-1.86627554892064));
#29738=CARTESIAN_POINT('Ctrl Pts',(30.,-3.87139572461206,-1.82944780129425));
#29739=CARTESIAN_POINT('Ctrl Pts',(30.,-3.89310152531943,-1.79227102496496));
#29740=CARTESIAN_POINT('Ctrl Pts',(30.,-3.90322370519929,-1.77493418388585));
#29741=CARTESIAN_POINT('Ctrl Pts',(30.,-3.91321999930958,-1.75752936221767));
#29742=CARTESIAN_POINT('Ctrl Pts',(30.,-3.92308811812892,-1.74006061666844));
#29743=CARTESIAN_POINT('Ctrl Pts',(30.,-3.95009373709925,-1.69225471821614));
#29744=CARTESIAN_POINT('Ctrl Pts',(30.,-3.97614326344458,-1.64396368682966));
#29745=CARTESIAN_POINT('Ctrl Pts',(30.,-4.00122119337617,-1.59521508212482));
#29746=CARTESIAN_POINT('Ctrl Pts',(30.,-4.0604952655639,-1.47999311913951));
#29747=CARTESIAN_POINT('Ctrl Pts',(30.,-4.11434404997915,-1.3622175869153));
#29748=CARTESIAN_POINT('Ctrl Pts',(30.,-4.16278065659499,-1.24231808149129));
#29749=CARTESIAN_POINT('Ctrl Pts',(30.,-4.21199575008708,-1.1204915172173));
#29750=CARTESIAN_POINT('Ctrl Pts',(30.,-4.2556236519386,-0.996471551733676));
#29751=CARTESIAN_POINT('Ctrl Pts',(30.,-4.29363802308023,-0.87067295455618));
#29752=CARTESIAN_POINT('Ctrl Pts',(30.,-4.32788619742269,-0.757337598510937));
#29753=CARTESIAN_POINT('Ctrl Pts',(30.,-4.35757766257454,-0.64255774676954));
#29754=CARTESIAN_POINT('Ctrl Pts',(30.,-4.38266244319943,-0.526618832262701));
#29755=CARTESIAN_POINT('Ctrl Pts',(30.,-4.40147602866809,-0.439664646382571));
#29756=CARTESIAN_POINT('Ctrl Pts',(30.,-4.41769777174343,-0.352058102522942));
#29757=CARTESIAN_POINT('Ctrl Pts',(30.,-4.43129498639204,-0.263915679232762));
#29758=CARTESIAN_POINT('Ctrl Pts',(30.,-4.43428278031165,-0.244547639294291));
#29759=CARTESIAN_POINT('Ctrl Pts',(30.,-4.43714381242759,-0.225153716221833));
#29760=CARTESIAN_POINT('Ctrl Pts',(30.,-4.4398776682558,-0.205735132850079));
#29761=CARTESIAN_POINT('Ctrl Pts',(30.,-4.44260800951335,-0.186341513480707));
#29762=CARTESIAN_POINT('Ctrl Pts',(30.,-4.4452104870011,-0.166930236534766));
#29763=CARTESIAN_POINT('Ctrl Pts',(30.,-4.44768398526052,-0.147510908969862));
#29764=CARTESIAN_POINT('Ctrl Pts',(30.,-4.46489551805196,-0.012383911448028));
#29765=CARTESIAN_POINT('Ctrl Pts',(30.,-4.47588310664295,0.123253849694283));
#29766=CARTESIAN_POINT('Ctrl Pts',(30.,-4.48063900854761,0.258956454195002));
#29767=CARTESIAN_POINT('Ctrl Pts',(30.,-4.4838586534793,0.350824245321806));
#29768=CARTESIAN_POINT('Ctrl Pts',(30.,-4.48422143108531,0.442722468953853));
#29769=CARTESIAN_POINT('Ctrl Pts',(30.,-4.48171298305417,0.534519091339923));
#29770=CARTESIAN_POINT('Ctrl Pts',(30.,-4.47802929541655,0.669323591517527));
#29771=CARTESIAN_POINT('Ctrl Pts',(30.,-4.46815627423761,0.803908859886495));
#29772=CARTESIAN_POINT('Ctrl Pts',(30.,-4.45227141268219,0.937896937469047));
#29773=CARTESIAN_POINT('Ctrl Pts',(30.,-4.43625288130477,1.0730125138602));
#29774=CARTESIAN_POINT('Ctrl Pts',(30.,-4.41412086479104,1.2075215698057));
#29775=CARTESIAN_POINT('Ctrl Pts',(30.,-4.38600459470813,1.34103973351968));
#29776=CARTESIAN_POINT('Ctrl Pts',(30.,-4.37816898656248,1.37824936367704));
#29777=CARTESIAN_POINT('Ctrl Pts',(30.,-4.36986829568835,1.41538201582188));
#29778=CARTESIAN_POINT('Ctrl Pts',(30.,-4.36110460428173,1.4524292877219));
#29779=CARTESIAN_POINT('Ctrl Pts',(30.,-4.35581208964338,1.47480264841483));
#29780=CARTESIAN_POINT('Ctrl Pts',(30.,-4.35035070722005,1.49714486882584));
#29781=CARTESIAN_POINT('Ctrl Pts',(30.,-4.34472086140207,1.51945408603399));
#29782=CARTESIAN_POINT('Ctrl Pts',(30.,-4.33978280888481,1.5390219551648));
#29783=CARTESIAN_POINT('Ctrl Pts',(30.,-4.33471469361921,1.55856590682949));
#29784=CARTESIAN_POINT('Ctrl Pts',(30.,-4.32952179802673,1.57806649106293));
#29785=CARTESIAN_POINT('Ctrl Pts',(30.,-4.29379022144892,1.71224723982657));
#29786=CARTESIAN_POINT('Ctrl Pts',(30.,-4.25210778635853,1.84456639657365));
#29787=CARTESIAN_POINT('Ctrl Pts',(30.,-4.20469449786056,1.97463023125887));
#29788=CARTESIAN_POINT('Ctrl Pts',(30.,-4.15669262462677,2.10630866788804));
#29789=CARTESIAN_POINT('Ctrl Pts',(30.,-4.10281668457366,2.23567622712646));
#29790=CARTESIAN_POINT('Ctrl Pts',(30.,-4.04324154822773,2.36232808049223));
#29791=CARTESIAN_POINT('Ctrl Pts',(30.,-3.98429992171791,2.48763314390853));
#29792=CARTESIAN_POINT('Ctrl Pts',(30.,-3.91977942670783,2.61028072798556));
#29793=CARTESIAN_POINT('Ctrl Pts',(30.,-3.84979985529667,2.72987071969418));
#29794=CARTESIAN_POINT('Ctrl Pts',(30.,-3.79916653436002,2.81639937811389));
#29795=CARTESIAN_POINT('Ctrl Pts',(30.,-3.74567425248624,2.90132720096679));
#29796=CARTESIAN_POINT('Ctrl Pts',(30.,-3.68943427790583,2.98455672438395));
#29797=CARTESIAN_POINT('Ctrl Pts',(30.,-3.66455056642679,3.02138212238069));
#29798=CARTESIAN_POINT('Ctrl Pts',(30.,-3.63912878255226,3.05787496526537));
#29799=CARTESIAN_POINT('Ctrl Pts',(30.,-3.61317781345119,3.0940263714018));
#29800=CARTESIAN_POINT('Ctrl Pts',(30.,-3.59843641711917,3.11456210568369));
#29801=CARTESIAN_POINT('Ctrl Pts',(30.,-3.58352425595821,3.1349876603743));
#29802=CARTESIAN_POINT('Ctrl Pts',(30.,-3.56844289678737,3.15530136335054));
#29803=CARTESIAN_POINT('Ctrl Pts',(30.,-3.55715233051782,3.17050909144953));
#29804=CARTESIAN_POINT('Ctrl Pts',(30.,-3.54576672263584,3.1856543120516));
#29805=CARTESIAN_POINT('Ctrl Pts',(30.,-3.5342960342479,3.20072435022002));
#29806=CARTESIAN_POINT('Ctrl Pts',(30.,-3.44911962237923,3.31262798969641));
#29807=CARTESIAN_POINT('Ctrl Pts',(30.,-3.3591351679399,3.42055154611245));
#29808=CARTESIAN_POINT('Ctrl Pts',(30.,-3.26472454399061,3.52427113846828));
#29809=CARTESIAN_POINT('Ctrl Pts',(30.,-3.16830407185099,3.63019875176792));
#29810=CARTESIAN_POINT('Ctrl Pts',(30.,-3.06726666550583,3.73174214688255));
#29811=CARTESIAN_POINT('Ctrl Pts',(30.,-2.96196811198104,3.82864480359171));
#29812=CARTESIAN_POINT('Ctrl Pts',(30.,-2.85628289510497,3.92590329335591));
#29813=CARTESIAN_POINT('Ctrl Pts',(30.,-2.74630470038239,4.01848753401441));
#29814=CARTESIAN_POINT('Ctrl Pts',(30.,-2.63234859559177,4.10611059145895));
#29815=CARTESIAN_POINT('Ctrl Pts',(30.,-2.51936339958007,4.19298709832716));
#29816=CARTESIAN_POINT('Ctrl Pts',(30.,-2.40246723845599,4.27498717097717));
#29817=CARTESIAN_POINT('Ctrl Pts',(30.,-2.28193118961066,4.35179519432719));
#29818=CARTESIAN_POINT('Ctrl Pts',(30.,-2.24443600532371,4.37568788881828));
#29819=CARTESIAN_POINT('Ctrl Pts',(30.,-2.206588376614,4.399077878459));
#29820=CARTESIAN_POINT('Ctrl Pts',(30.,-2.16839587231052,4.42195480991684));
#29821=CARTESIAN_POINT('Ctrl Pts',(30.,-2.36248025497576,-3.31498400274172));
#29822=CARTESIAN_POINT('Ctrl Pts',(30.0337330633174,-1.89383404148126,-3.64828974744648));
#29823=CARTESIAN_POINT('Ctrl Pts',(30.1071024596332,-0.719464415258844,
-4.15646547691744));
#29824=CARTESIAN_POINT('Ctrl Pts',(30.2201081889472,1.26526436571728,-4.04962641418862));
#29825=CARTESIAN_POINT('Ctrl Pts',(30.3390171879422,3.04621666442482,-2.95311080905282));
#29826=CARTESIAN_POINT('Ctrl Pts',(30.4579261869372,4.08693028190598,-1.13899868222102));
#29827=CARTESIAN_POINT('Ctrl Pts',(30.5768351859321,4.13451402698658,0.951899428186699));
#29828=CARTESIAN_POINT('Ctrl Pts',(30.6957441849271,3.17740294051253,2.81148064688808));
#29829=CARTESIAN_POINT('Ctrl Pts',(30.814653183922,1.44817770927032,3.9878689759897));
#29830=CARTESIAN_POINT('Ctrl Pts',(30.933562182917,-0.632957413458418,4.19519723441137));
#29831=CARTESIAN_POINT('Ctrl Pts',(31.052471181912,-2.56028269018139,3.38308567277929));
#29832=CARTESIAN_POINT('Ctrl Pts',(31.1655546772976,-3.80151277967511,1.82894004492933));
#29833=CARTESIAN_POINT('Ctrl Pts',(31.2390018396849,-4.0701317662764,0.576320676525326));
#29834=CARTESIAN_POINT('Ctrl Pts',(31.2728126690739,-4.07067546468071,-8.70709291818372E-5));
#29835=CARTESIAN_POINT('Origin',(27.2271873309261,0.,0.));
#29836=CARTESIAN_POINT('',(30.,2.36230756092327,-3.31488661006749));
#29837=CARTESIAN_POINT('Origin',(30.,0.,0.));
#29838=CARTESIAN_POINT('Ctrl Pts',(30.,2.36230756092327,-3.31488661006749));
#29839=CARTESIAN_POINT('Ctrl Pts',(30.0396363329983,2.91267249451483,-2.92267674082436));
#29840=CARTESIAN_POINT('Ctrl Pts',(30.118908998995,3.81372229645613,-1.85922486464953));
#29841=CARTESIAN_POINT('Ctrl Pts',(30.2378179979899,4.23847383186721,0.18897419945147));
#29842=CARTESIAN_POINT('Ctrl Pts',(30.3567269969849,3.63326524445147,2.1907645291121));
#29843=CARTESIAN_POINT('Ctrl Pts',(30.4756359959799,2.14517067243769,3.66043220391454));
#29844=CARTESIAN_POINT('Ctrl Pts',(30.5945449949748,0.135793758977664,4.24049025960433));
#29845=CARTESIAN_POINT('Ctrl Pts',(30.7134539939698,-1.90658020521281,3.79016095005708));
#29846=CARTESIAN_POINT('Ctrl Pts',(30.8323629929647,-3.48565237567683,2.4187862103776));
#29847=CARTESIAN_POINT('Ctrl Pts',(30.9202741052835,-4.02686901485062,0.970374195636228));
#29848=CARTESIAN_POINT('Ctrl Pts',(30.968548884604,-4.07067913832741,0.147388342502041));
#29849=CARTESIAN_POINT('Ctrl Pts',(30.9771873309261,-4.07052775430868,0.000104499988540334));
#29850=CARTESIAN_POINT('Ctrl Pts',(29.5066541949775,2.85821514250015,-4.01076441581687));
#29851=CARTESIAN_POINT('Ctrl Pts',(29.5462905279758,3.52411547364828,-3.53621986207105));
#29852=CARTESIAN_POINT('Ctrl Pts',(29.6255631939724,4.61431821890341,-2.24952277567846));
#29853=CARTESIAN_POINT('Ctrl Pts',(29.7444721929674,5.12823575038595,0.228644621618519));
#29854=CARTESIAN_POINT('Ctrl Pts',(29.8633811919623,4.39597870751103,2.65066092761991));
#29855=CARTESIAN_POINT('Ctrl Pts',(29.9822901909573,2.59549577736295,4.42884869285811));
#29856=CARTESIAN_POINT('Ctrl Pts',(30.1011991899523,0.16430027342226,5.1306754768582));
#29857=CARTESIAN_POINT('Ctrl Pts',(30.2201081889472,-2.30681918945408,4.58581075519745));
#29858=CARTESIAN_POINT('Ctrl Pts',(30.3390171879422,-4.21737819683287,2.9265500764304));
#29859=CARTESIAN_POINT('Ctrl Pts',(30.4579261869371,-5.10310658405598,0.556150600520288));
#29860=CARTESIAN_POINT('Ctrl Pts',(30.5768351859321,-4.74877129058131,-1.94940347074711));
#29861=CARTESIAN_POINT('Ctrl Pts',(30.6957441849271,-3.24047616811104,-3.98124455736783));
#29862=CARTESIAN_POINT('Ctrl Pts',(30.814653183922,-0.944739698215852,-5.04563850679249));
#29863=CARTESIAN_POINT('Ctrl Pts',(30.933562182917,1.58057019484585,-4.8839323181771));
#29864=CARTESIAN_POINT('Ctrl Pts',(31.052471181912,3.72179874989839,-3.53542258613139));
#29865=CARTESIAN_POINT('Ctrl Pts',(31.1713801809069,4.95862369057364,-1.32779868315432));
#29866=CARTESIAN_POINT('Ctrl Pts',(31.2902891799019,4.99049438067752,1.20248248380908));
#29867=CARTESIAN_POINT('Ctrl Pts',(31.4091981788969,3.80966619055483,3.44055837141513));
#29868=CARTESIAN_POINT('Ctrl Pts',(31.5281071778918,1.70308243813102,4.84257250835442));
#29869=CARTESIAN_POINT('Ctrl Pts',(31.6470161768868,-0.817353331486976,
5.06783305606493));
#29870=CARTESIAN_POINT('Ctrl Pts',(31.7659251758817,-3.13917080911228,4.06160127951951));
#29871=CARTESIAN_POINT('Ctrl Pts',(31.8848341748767,-4.6981642778999,2.06839327767044));
#29872=CARTESIAN_POINT('Ctrl Pts',(32.0037431738716,-5.11549559255233,-0.427437918277657));
#29873=CARTESIAN_POINT('Ctrl Pts',(32.1226521728666,-4.28975251207502,-2.81940094975718));
#29874=CARTESIAN_POINT('Ctrl Pts',(32.2415611718616,-2.42159205236551,-4.52624460934904));
#29875=CARTESIAN_POINT('Ctrl Pts',(32.3604701708566,0.0350195204882076,
-5.13320289526554));
#29876=CARTESIAN_POINT('Ctrl Pts',(32.4793791698515,2.48312128848067,-4.49278388062119));
#29877=CARTESIAN_POINT('Ctrl Pts',(32.5982881688465,4.32782023111487,-2.76061050824488));
#29878=CARTESIAN_POINT('Ctrl Pts',(32.7171971678414,5.12085127205647,-0.357603943776774));
#29879=CARTESIAN_POINT('Ctrl Pts',(32.8361061668364,4.66950647838273,2.1323010058329));
#29880=CARTESIAN_POINT('Ctrl Pts',(32.9550151658313,3.08346342604463,4.10405307365304));
#29881=CARTESIAN_POINT('Ctrl Pts',(33.0739241648263,0.748133356677078,5.07851305125401));
#29882=CARTESIAN_POINT('Ctrl Pts',(33.1928331638213,-1.76899442964414,4.81888545609981));
#29883=CARTESIAN_POINT('Ctrl Pts',(33.3117421628162,-3.85625346897966,3.38826024887523));
#29884=CARTESIAN_POINT('Ctrl Pts',(33.4306511618112,-5.00643615635466,1.134281862444));
#29885=CARTESIAN_POINT('Ctrl Pts',(33.5495601608061,-4.94004608276915,-1.39532900465872));
#29886=CARTESIAN_POINT('Ctrl Pts',(33.6684691598011,-3.67321615246874,-3.58587247798463));
#29887=CARTESIAN_POINT('Ctrl Pts',(33.7873781587961,-1.51378825893625,-4.90504265406851));
#29888=CARTESIAN_POINT('Ctrl Pts',(33.9062871577911,1.01349283479057,-5.0322788679636));
#29889=CARTESIAN_POINT('Ctrl Pts',(34.025196156786,3.2944933932768,-3.93666249668171));
#29890=CARTESIAN_POINT('Ctrl Pts',(34.144105155781,4.77492628281602,-1.88443023877182));
#29891=CARTESIAN_POINT('Ctrl Pts',(34.2630141547759,5.09504371644056,0.625721870070408));
#29892=CARTESIAN_POINT('Ctrl Pts',(34.3819231537709,4.17705659669796,2.98382246775958));
#29893=CARTESIAN_POINT('Ctrl Pts',(34.5008321527659,2.24403740267574,4.61684897592689));
#29894=CARTESIAN_POINT('Ctrl Pts',(34.6197411517608,-0.234286813404278,
5.12797309082153));
#29895=CARTESIAN_POINT('Ctrl Pts',(34.7386501507558,-2.65567892318387,4.39299075665791));
#29896=CARTESIAN_POINT('Ctrl Pts',(34.8575591497507,-4.43173639992282,2.59050396886859));
#29897=CARTESIAN_POINT('Ctrl Pts',(34.9764681487457,-5.13087416381178,0.158520176171834));
#29898=CARTESIAN_POINT('Ctrl Pts',(35.0953771477407,-4.58320051282105,-2.31198429717886));
#29899=CARTESIAN_POINT('Ctrl Pts',(35.2142861467356,-2.92180110406929,-4.22067253401449));
#29900=CARTESIAN_POINT('Ctrl Pts',(35.3331951457306,-0.550398905879517,
-5.10372994735531));
#29901=CARTESIAN_POINT('Ctrl Pts',(35.4521041447255,1.95475119114355,-4.74657203799202));
#29902=CARTESIAN_POINT('Ctrl Pts',(35.5710131437205,3.98489332255382,-3.23598880390381));
#29903=CARTESIAN_POINT('Ctrl Pts',(35.6899221427155,5.04669939211318,-0.939054618629394));
#29904=CARTESIAN_POINT('Ctrl Pts',(35.8088311417105,4.88214866385187,1.58607148488782));
#29905=CARTESIAN_POINT('Ctrl Pts',(35.9277401407054,3.53122725315149,3.72577943761101));
#29906=CARTESIAN_POINT('Ctrl Pts',(36.0466491397003,1.32221143062236,4.96011645668286));
#29907=CARTESIAN_POINT('Ctrl Pts',(36.1655581386953,-1.20810408703707,4.98913648300082));
#29908=CARTESIAN_POINT('Ctrl Pts',(36.2844671376903,-3.44484819405753,3.80578759930478));
#29909=CARTESIAN_POINT('Ctrl Pts',(36.4033761366852,-4.84448815200906,1.69762565843315));
#29910=CARTESIAN_POINT('Ctrl Pts',(36.5222851356802,-5.06690899790788,-0.823062292930284));
#29911=CARTESIAN_POINT('Ctrl Pts',(36.6411941346751,-4.05806207635667,-3.14374466449768));
#29912=CARTESIAN_POINT('Ctrl Pts',(36.7601031336701,-2.06309895753307,-4.70049157243862));
#29913=CARTESIAN_POINT('Ctrl Pts',(36.8790121326651,0.433200824037541,-5.11501078954236));
#29914=CARTESIAN_POINT('Ctrl Pts',(36.9979211316601,2.82423204608698,-4.28657341953556));
#29915=CARTESIAN_POINT('Ctrl Pts',(37.116830130655,4.52896993078687,-2.41649119531078));
#29916=CARTESIAN_POINT('Ctrl Pts',(37.23573912965,5.13316018424025,0.0408026247792082));
#29917=CARTESIAN_POINT('Ctrl Pts',(37.3546481286449,4.48998351578663,2.48818133566934));
#29918=CARTESIAN_POINT('Ctrl Pts',(37.4735571276399,2.75573298334866,4.33092762058931));
#29919=CARTESIAN_POINT('Ctrl Pts',(37.5924661266348,0.351834505657344,5.12125090327671));
#29920=CARTESIAN_POINT('Ctrl Pts',(37.7113751256298,-2.13756037313485,4.66710123916826));
#29921=CARTESIAN_POINT('Ctrl Pts',(37.8302841246247,-4.10752433556602,3.07883779592106));
#29922=CARTESIAN_POINT('Ctrl Pts',(37.9491931236198,-5.07935268326507,0.742411367522402));
#29923=CARTESIAN_POINT('Ctrl Pts',(38.0681021226147,-4.81688942970997,-1.7744223157606));
#29924=CARTESIAN_POINT('Ctrl Pts',(38.1870111216097,-3.38391359491544,-3.86006828352247));
#29925=CARTESIAN_POINT('Ctrl Pts',(38.3059201206046,-1.12864083956594,-5.00771085818741));
#29926=CARTESIAN_POINT('Ctrl Pts',(38.4248291195997,1.40089364617361,-4.93847098595927));
#29927=CARTESIAN_POINT('Ctrl Pts',(38.5437381185945,3.59000846431617,-3.66917387097732));
#29928=CARTESIAN_POINT('Ctrl Pts',(38.6626471175895,4.90674504534453,-1.50826134816256));
#29929=CARTESIAN_POINT('Ctrl Pts',(38.7815561165844,5.03113375661037,1.01916187219467));
#29930=CARTESIAN_POINT('Ctrl Pts',(38.9004651155795,3.93294859258498,3.2989258815117));
#29931=CARTESIAN_POINT('Ctrl Pts',(39.0193741145744,1.87904913788996,4.77704729317024));
#29932=CARTESIAN_POINT('Ctrl Pts',(39.1382831135694,-0.631460777071341,
5.09433350395094));
#29933=CARTESIAN_POINT('Ctrl Pts',(39.2571921125643,-2.98852815433904,4.17369639243061));
#29934=CARTESIAN_POINT('Ctrl Pts',(39.3761011115593,-4.6193708951497,2.2388264922051));
#29935=CARTESIAN_POINT('Ctrl Pts',(39.4950101105542,-5.12771248771455,-0.240047762388298));
#29936=CARTESIAN_POINT('Ctrl Pts',(39.6139191095492,-4.38998288215063,-2.66065861991797));
#29937=CARTESIAN_POINT('Ctrl Pts',(39.7328281085441,-2.58553574319963,-4.43458787788333));
#29938=CARTESIAN_POINT('Ctrl Pts',(39.8517371075391,-0.152687184564566,
-5.13117755701021));
#29939=CARTESIAN_POINT('Ctrl Pts',(39.970646106534,2.31704182252175,-4.58033746598028));
#29940=CARTESIAN_POINT('Ctrl Pts',(40.0895551055291,4.22417001907876,-2.91755367341275));
#29941=CARTESIAN_POINT('Ctrl Pts',(40.208464104524,5.10393106315724,-0.543632473763103));
#29942=CARTESIAN_POINT('Ctrl Pts',(40.327373103519,4.74519592562567,1.95807152784698));
#29943=CARTESIAN_POINT('Ctrl Pts',(40.4462821025139,3.22984460904033,3.99256580976687));
#29944=CARTESIAN_POINT('Ctrl Pts',(40.5651911015089,0.936651920722019,5.03986235081967));
#29945=CARTESIAN_POINT('Ctrl Pts',(40.7237364335022,-2.4427025544272,4.84519165873018));
#29946=CARTESIAN_POINT('Ctrl Pts',(40.9219180984937,-5.62465210210655,1.50291923965302));
#29947=CARTESIAN_POINT('Ctrl Pts',(41.1597360964838,-4.30522090115316,-3.91925381966069));
#29948=CARTESIAN_POINT('Ctrl Pts',(41.3579177614752,0.0566434889063053,
-5.42581509954019));
#29949=CARTESIAN_POINT('Ctrl Pts',(41.5164630934686,3.14760490934904,-4.04599958853725));
#29950=CARTESIAN_POINT('Ctrl Pts',(41.6353720924635,4.70319633240609,-2.0621401995762));
#29951=CARTESIAN_POINT('Ctrl Pts',(41.7542810914585,5.1143250588496,0.441143596986738));
#29952=CARTESIAN_POINT('Ctrl Pts',(41.8731900904534,4.28348653516322,2.82796599468003));
#29953=CARTESIAN_POINT('Ctrl Pts',(41.9920990894484,2.41133830213583,4.53223778943481));
#29954=CARTESIAN_POINT('Ctrl Pts',(42.1110080884434,-0.0465611259332376,
5.13283607483518));
#29955=CARTESIAN_POINT('Ctrl Pts',(42.2299170874384,-2.4932505334136,4.48731526366583));
#29956=CARTESIAN_POINT('Ctrl Pts',(42.3488260864333,-4.33402334229477,2.75078286938043));
#29957=CARTESIAN_POINT('Ctrl Pts',(42.4677350854283,-5.12164712760539,0.34609925976627));
#29958=CARTESIAN_POINT('Ctrl Pts',(42.5866440844232,-4.6646885261814,-2.14283439364853));
#29959=CARTESIAN_POINT('Ctrl Pts',(42.7055530834183,-3.07420903354032,-4.11098167683274));
#29960=CARTESIAN_POINT('Ctrl Pts',(42.8244620824131,-0.736688050284008,
-5.08019023482725));
#29961=CARTESIAN_POINT('Ctrl Pts',(42.9433710814081,1.77984776236949,-4.81488509782371));
#29962=CARTESIAN_POINT('Ctrl Pts',(43.0622800804031,3.86387828041411,-3.3795637496479));
#29963=CARTESIAN_POINT('Ctrl Pts',(43.181189079398,5.00897918721084,-1.12299782088504));
#29964=CARTESIAN_POINT('Ctrl Pts',(43.3000980783931,4.93688958102473,1.40645620742674));
#29965=CARTESIAN_POINT('Ctrl Pts',(43.4190070773879,3.6651270488325,3.59414008495642));
#29966=CARTESIAN_POINT('Ctrl Pts',(43.5379160763829,1.50273227228464,4.90844103429577));
#29967=CARTESIAN_POINT('Ctrl Pts',(43.6568250753779,-1.02482910665101,5.02998250386739));
#29968=CARTESIAN_POINT('Ctrl Pts',(43.7757340743728,-3.30335520321506,3.92922926097933));
#29969=CARTESIAN_POINT('Ctrl Pts',(43.8946430733678,-4.77916020210216,1.87366649485778));
#29970=CARTESIAN_POINT('Ctrl Pts',(44.0135520723628,-5.09362089194941,-0.63720055070383));
#29971=CARTESIAN_POINT('Ctrl Pts',(44.1324610713577,-4.17032277893803,-2.99322672697694));
#29972=CARTESIAN_POINT('Ctrl Pts',(44.2513700703527,-2.23362892033142,-4.62189357159142));
#29973=CARTESIAN_POINT('Ctrl Pts',(44.3702790693477,0.2458406804619,-5.12743217266424));
#29974=CARTESIAN_POINT('Ctrl Pts',(44.4891880683426,2.6655705652185,-4.38699577108576));
#29975=CARTESIAN_POINT('Ctrl Pts',(44.6080970673376,4.43756213047755,-2.58051170670677));
#29976=CARTESIAN_POINT('Ctrl Pts',(44.7270060663325,5.13121832020351,-0.146958775229261));
#29977=CARTESIAN_POINT('Ctrl Pts',(44.8459150653274,4.57797946441693,2.32230539650474));
#29978=CARTESIAN_POINT('Ctrl Pts',(44.9648240643225,2.91228357479588,4.22724528634906));
#29979=CARTESIAN_POINT('Ctrl Pts',(45.0837330633174,0.538897672025354,5.10495716243527));
#29980=CARTESIAN_POINT('Ctrl Pts',(45.2026420623124,-1.96544130958994,4.74215550036467));
#29981=CARTESIAN_POINT('Ctrl Pts',(45.3215510613073,-3.99217460807465,3.22700173997235));
#29982=CARTESIAN_POINT('Ctrl Pts',(45.4404600603023,-5.0488024795639,0.927680900671747));
#29983=CARTESIAN_POINT('Ctrl Pts',(45.5593690592972,-4.8785624992962,-1.59706802346811));
#29984=CARTESIAN_POINT('Ctrl Pts',(45.6782780582923,-3.52282328086189,-3.73372661866722));
#29985=CARTESIAN_POINT('Ctrl Pts',(45.7971870572872,-1.31103183059522,-4.96308310128791));
#29986=CARTESIAN_POINT('Ctrl Pts',(45.9160960562822,1.21934265240026,-4.9864016913164));
#29987=CARTESIAN_POINT('Ctrl Pts',(46.0350050552771,3.45341473367536,-3.79801593050351));
#29988=CARTESIAN_POINT('Ctrl Pts',(46.1539140542721,4.84830098173927,-1.68670564165504));
#29989=CARTESIAN_POINT('Ctrl Pts',(46.272823053267,5.06504159344358,0.834477074467225));
#29990=CARTESIAN_POINT('Ctrl Pts',(46.391732052262,4.05096822025483,3.15288039887499));
#29991=CARTESIAN_POINT('Ctrl Pts',(46.510641051257,2.05250246926194,4.70512826018573));
#29992=CARTESIAN_POINT('Ctrl Pts',(46.6295500502519,-0.444724979258798,
5.11402170741854));
#29993=CARTESIAN_POINT('Ctrl Pts',(46.7484590492469,-2.83388347833368,4.28019891621314));
#29994=CARTESIAN_POINT('Ctrl Pts',(46.8673680482419,-4.53440332512082,2.40628028630458));
#29995=CARTESIAN_POINT('Ctrl Pts',(46.9862770472368,-5.13305521628673,-0.052368670752719));
#29996=CARTESIAN_POINT('Ctrl Pts',(47.1051860462318,-4.4843656929987,-2.4982919490286));
#29997=CARTESIAN_POINT('Ctrl Pts',(47.2240950452266,-2.74596744639791,-4.33712590484156));
#29998=CARTESIAN_POINT('Ctrl Pts',(47.3430040442218,-0.340294297363466,
-5.12203066393659));
#29999=CARTESIAN_POINT('Ctrl Pts',(47.4619130432166,2.14807096237674,-4.66227299412192));
#30000=CARTESIAN_POINT('Ctrl Pts',(47.5808220422116,4.11445121325577,-3.06957481499685));
#30001=CARTESIAN_POINT('Ctrl Pts',(47.6997310412066,5.08101260776241,-0.730964575669896));
#30002=CARTESIAN_POINT('Ctrl Pts',(47.8186400402016,4.81287903290352,1.78527133673356));
#30003=CARTESIAN_POINT('Ctrl Pts',(47.9375490391965,3.37520741733752,3.86768318519946));
#30004=CARTESIAN_POINT('Ctrl Pts',(48.0564580381915,1.11735448350728,5.01024124063013));
#30005=CARTESIAN_POINT('Ctrl Pts',(48.1753670371864,-1.41201754824387,4.93530189295206));
#30006=CARTESIAN_POINT('Ctrl Pts',(48.2942760361814,-3.59826684087623,3.66107553499997));
#30007=CARTESIAN_POINT('Ctrl Pts',(48.4131850351763,-4.91013098435995,1.49720140514004));
#30008=CARTESIAN_POINT('Ctrl Pts',(48.5320940341713,-5.02882469247548,-1.03049529036943));
#30009=CARTESIAN_POINT('Ctrl Pts',(48.6510030331663,-3.92550518611198,-3.30777982413168));
#30010=CARTESIAN_POINT('Ctrl Pts',(48.7699120321612,-1.86828103914462,-4.78126806296179));
#30011=CARTESIAN_POINT('Ctrl Pts',(48.8888210311562,0.642938674940074,-5.09289978218584));
#30012=CARTESIAN_POINT('Ctrl Pts',(49.0077300301511,2.99792316411244,-4.1669479278254));
#30013=CARTESIAN_POINT('Ctrl Pts',(49.1266390291461,4.62440706983327,-2.22842042343719));
#30014=CARTESIAN_POINT('Ctrl Pts',(49.2455480281411,5.12715195221699,0.251617149677375));
#30015=CARTESIAN_POINT('Ctrl Pts',(49.3644570271361,4.38398992365829,2.67051131440959));
#30016=CARTESIAN_POINT('Ctrl Pts',(49.483366026131,2.57551065967751,4.44046654902013));
#30017=CARTESIAN_POINT('Ctrl Pts',(49.602275025126,0.141177791184851,5.13138062928017));
#30018=CARTESIAN_POINT('Ctrl Pts',(49.7211840241209,-2.32746152797901,4.57536022260056));
#30019=CARTESIAN_POINT('Ctrl Pts',(49.8400930231159,-4.23052361648418,2.90751926255194));
#30020=CARTESIAN_POINT('Ctrl Pts',(49.9590020221109,-5.10556105105169,0.533146025334083));
#30021=CARTESIAN_POINT('Ctrl Pts',(50.0779110211058,-4.73993820177943,-1.97078263000154));
#30022=CARTESIAN_POINT('Ctrl Pts',(50.1968200201008,-3.22250206106676,-3.99580765298676));
#30023=CARTESIAN_POINT('Ctrl Pts',(50.3157290190957,-0.921992272398132,
-5.04984441069379));
#30024=CARTESIAN_POINT('Ctrl Pts',(50.4346380180907,1.60256325663182,-4.87676012954613));
#30025=CARTESIAN_POINT('Ctrl Pts',(50.5535470170856,3.73769310112268,-3.51861458127488));
#30026=CARTESIAN_POINT('Ctrl Pts',(50.6724560160806,4.96455697943528,-1.30543953843589));
#30027=CARTESIAN_POINT('Ctrl Pts',(50.7913650150756,4.98502479305234,1.22495963202668));
#30028=CARTESIAN_POINT('Ctrl Pts',(50.9102740140705,3.79412287868718,3.45769140166195));
#30029=CARTESIAN_POINT('Ctrl Pts',(51.0291830130655,1.68124238654991,4.85019822635541));
#30030=CARTESIAN_POINT('Ctrl Pts',(51.1480920120605,-0.840182816358251,
5.06409812942702));
#30031=CARTESIAN_POINT('Ctrl Pts',(51.2670010110554,-3.15744239341537,4.04741381265562));
#30032=CARTESIAN_POINT('Ctrl Pts',(51.3859100100504,-4.70743739387435,2.04719984476848));
#30033=CARTESIAN_POINT('Ctrl Pts',(51.5048190090453,-5.11351793548239,-0.450485277794991));
#30034=CARTESIAN_POINT('Ctrl Pts',(51.6237280080403,-4.27700250438477,-2.83870566917055));
#30035=CARTESIAN_POINT('Ctrl Pts',(51.7426370070352,-2.40117226017362,-4.53710766699985));
#30036=CARTESIAN_POINT('Ctrl Pts',(51.8615460060303,0.0581556126824071,
-5.13300038769059));
#30037=CARTESIAN_POINT('Ctrl Pts',(51.9804550050251,2.50333449393975,-4.48153342508255));
#30038=CARTESIAN_POINT('Ctrl Pts',(52.0993640040202,4.34023276718783,-2.74110900935533));
#30039=CARTESIAN_POINT('Ctrl Pts',(52.2182730030151,5.12237890697843,-0.334464472617914));
#30040=CARTESIAN_POINT('Ctrl Pts',(52.3371820020101,4.65991385425871,2.15320299679786));
#30041=CARTESIAN_POINT('Ctrl Pts',(52.456091001005,3.06480663880283,4.11816046437608));
#30042=CARTESIAN_POINT('Ctrl Pts',(52.5353636670017,1.50529535683805,4.76007633060593));
#30043=CARTESIAN_POINT('Ctrl Pts',(52.575,0.695807839646318,4.87560011181052));
#30044=CARTESIAN_POINT('Ctrl Pts',(29.6711027966516,2.69291261530786,-3.77880514723374));
#30045=CARTESIAN_POINT('Ctrl Pts',(29.71073912965,3.32030114727046,-3.33170548832215));
#30046=CARTESIAN_POINT('Ctrl Pts',(29.7900117956466,4.34745291142099,-2.11942347200215));
#30047=CARTESIAN_POINT('Ctrl Pts',(29.9089207946416,4.83164844421304,0.215421147562834));
#30048=CARTESIAN_POINT('Ctrl Pts',(30.0278297936365,4.14174088649117,2.49736212811731));
#30049=CARTESIAN_POINT('Ctrl Pts',(30.1467387926315,2.44538740905453,4.17270986321025));
#30050=CARTESIAN_POINT('Ctrl Pts',(30.2656477916265,0.154798101940727,4.83394707110692));
#30051=CARTESIAN_POINT('Ctrl Pts',(30.3845567906213,-2.17340619470699,4.32059415348399));
#30052=CARTESIAN_POINT('Ctrl Pts',(30.5034657896164,-3.97346958978086,2.7572954544128));
#30053=CARTESIAN_POINT('Ctrl Pts',(30.6223747886113,-4.80797260259568,0.523986086940263));
#30054=CARTESIAN_POINT('Ctrl Pts',(30.7412837876063,-4.47413000003635,-1.83666132078074));
#30055=CARTESIAN_POINT('Ctrl Pts',(30.8601927866012,-3.05306588820233,-3.75099254557286));
#30056=CARTESIAN_POINT('Ctrl Pts',(30.9791017855962,-0.890101453063521,
-4.75382814441996));
#30057=CARTESIAN_POINT('Ctrl Pts',(31.0980107845912,1.48915921471079,-4.60147410052008));
#30058=CARTESIAN_POINT('Ctrl Pts',(31.2169197835862,3.50655157346604,-3.33095432218219));
#30059=CARTESIAN_POINT('Ctrl Pts',(31.3358287825811,4.67184575868903,-1.25100653596273));
#30060=CARTESIAN_POINT('Ctrl Pts',(31.4547377815761,4.7018732335852,1.1329378961668));
#30061=CARTESIAN_POINT('Ctrl Pts',(31.573646780571,3.58933727279988,3.24157650147442));
#30062=CARTESIAN_POINT('Ctrl Pts',(31.692555779566,1.60458606294434,4.56250630135687));
#30063=CARTESIAN_POINT('Ctrl Pts',(31.8114647785609,-0.770082372315719,
4.77473909014902));
#30064=CARTESIAN_POINT('Ctrl Pts',(31.9303737775559,-2.95761944150577,3.82670190264306));
#30065=CARTESIAN_POINT('Ctrl Pts',(32.0492827765509,-4.42644980240309,1.94876944986877));
#30066=CARTESIAN_POINT('Ctrl Pts',(32.1681917755458,-4.8196451029526,-0.402717397048015));
#30067=CARTESIAN_POINT('Ctrl Pts',(32.2871007745408,-4.04165819589442,-2.65634320954958));
#30068=CARTESIAN_POINT('Ctrl Pts',(32.4060097735358,-2.28154126327945,-4.2644729667982));
#30069=CARTESIAN_POINT('Ctrl Pts',(32.5249187725307,0.0329941952593177,
-4.83632831834477));
#30070=CARTESIAN_POINT('Ctrl Pts',(32.6438277715257,2.33951200651746,-4.232947411857));
#30071=CARTESIAN_POINT('Ctrl Pts',(32.7627367705207,4.07752429964364,-2.60095286497615));
#30072=CARTESIAN_POINT('Ctrl Pts',(32.8816457695156,4.82469104112772,-0.336922213153589));
#30073=CARTESIAN_POINT('Ctrl Pts',(33.0005547685106,4.39944940320316,2.00898112701842));
#30074=CARTESIAN_POINT('Ctrl Pts',(33.1194637675055,2.90513384922194,3.86669853210067));
#30075=CARTESIAN_POINT('Ctrl Pts',(33.2383727665005,0.704865677944022,4.78480141658081));
#30076=CARTESIAN_POINT('Ctrl Pts',(33.3572817654954,-1.66668608851854,4.54018917033078));
#30077=CARTESIAN_POINT('Ctrl Pts',(33.4761907644904,-3.63323021420857,3.1923029979335));
#30078=CARTESIAN_POINT('Ctrl Pts',(33.5950997634854,-4.71689302974857,1.06868160176998));
#30079=CARTESIAN_POINT('Ctrl Pts',(33.7140087624803,-4.65434257158632,-1.31463129674126));
#30080=CARTESIAN_POINT('Ctrl Pts',(33.8329177614753,-3.46077871068974,-3.37848648594147));
#30081=CARTESIAN_POINT('Ctrl Pts',(33.9518267604703,-1.42623955726036,-4.62136353745928));
#30082=CARTESIAN_POINT('Ctrl Pts',(34.0707357594652,0.954878308406255,-4.74124114933924));
#30083=CARTESIAN_POINT('Ctrl Pts',(34.1896447584602,3.10395907147953,-3.70898885178054));
#30084=CARTESIAN_POINT('Ctrl Pts',(34.3085537574551,4.49877233975909,-1.77544576235687));
#30085=CARTESIAN_POINT('Ctrl Pts',(34.4274627564501,4.80037604431206,0.589533759209166));
#30086=CARTESIAN_POINT('Ctrl Pts',(34.546371755445,3.93547995630008,2.81125554398968));
#30087=CARTESIAN_POINT('Ctrl Pts',(34.66528075444,2.11425534104551,4.34983730418886));
#30088=CARTESIAN_POINT('Ctrl Pts',(34.784189753435,-0.22073702781689,4.83140097534898));
#30089=CARTESIAN_POINT('Ctrl Pts',(34.9030987524299,-2.50208991202581,4.1389257413236));
#30090=CARTESIAN_POINT('Ctrl Pts',(35.0220077514249,-4.17543056210665,2.44068429770795));
#30091=CARTESIAN_POINT('Ctrl Pts',(35.1409167504199,-4.83413426716358,0.149352291871387));
#30092=CARTESIAN_POINT('Ctrl Pts',(35.2598257494149,-4.31813487233336,-2.17827258266522));
#30093=CARTESIAN_POINT('Ctrl Pts',(35.3787347484098,-2.75282113497098,-3.97657340167505));
#30094=CARTESIAN_POINT('Ctrl Pts',(35.4976437474048,-0.518567036838953,
-4.80855991419017));
#30095=CARTESIAN_POINT('Ctrl Pts',(35.6165527463997,1.84169976015662,-4.47205793941574));
#30096=CARTESIAN_POINT('Ctrl Pts',(35.7354617453947,3.75443028741865,-3.04883804702151));
#30097=CARTESIAN_POINT('Ctrl Pts',(35.8543707443897,4.75482767430874,-0.884745165389519));
#30098=CARTESIAN_POINT('Ctrl Pts',(35.9732797433846,4.59979360237901,1.49434234215777));
#30099=CARTESIAN_POINT('Ctrl Pts',(36.0921887423796,3.32700162284231,3.51030204137153));
#30100=CARTESIAN_POINT('Ctrl Pts',(36.2110977413745,1.24574241759582,4.67325219189535));
#30101=CARTESIAN_POINT('Ctrl Pts',(36.3300067403695,-1.13823437858544,4.70059386880629));
#30102=CARTESIAN_POINT('Ctrl Pts',(36.4489157393644,-3.24561822574471,3.58568299669183));
#30103=CARTESIAN_POINT('Ctrl Pts',(36.5678247383594,-4.5643111553328,1.59944487162223));
#30104=CARTESIAN_POINT('Ctrl Pts',(36.6867337373544,-4.77386847413717,-0.775461160658975));
#30105=CARTESIAN_POINT('Ctrl Pts',(36.8056427363493,-3.82336738639071,-2.96192877171846));
#30106=CARTESIAN_POINT('Ctrl Pts',(36.9245517353443,-1.9437813223918,-4.42864249977205));
#30107=CARTESIAN_POINT('Ctrl Pts',(37.0434607343393,0.408147009882566,-4.81918833812686));
#30108=CARTESIAN_POINT('Ctrl Pts',(37.1623697333342,2.66089490338775,-4.03866296356309));
#30109=CARTESIAN_POINT('Ctrl Pts',(37.2812787323291,4.26704067150719,-2.27673541010649));
#30110=CARTESIAN_POINT('Ctrl Pts',(37.4001877313242,4.83628807747657,0.0384428384595121));
#30111=CARTESIAN_POINT('Ctrl Pts',(37.5190967303191,4.23030900382455,2.34427941002946));
#30112=CARTESIAN_POINT('Ctrl Pts',(37.6380057293141,2.59635742772959,4.08045197579788));
#30113=CARTESIAN_POINT('Ctrl Pts',(37.756914728309,0.33148644575315,4.82506756000429));
#30114=CARTESIAN_POINT('Ctrl Pts',(37.875823727304,-2.01393632312853,4.39718326902481));
#30115=CARTESIAN_POINT('Ctrl Pts',(37.9947327262989,-3.86996903642957,2.90077573862057));
#30116=CARTESIAN_POINT('Ctrl Pts',(38.1136417252939,-4.78559248916355,0.6994746153364));
#30117=CARTESIAN_POINT('Ctrl Pts',(38.2325507242889,-4.53830858248917,-1.67180005729582));
#30118=CARTESIAN_POINT('Ctrl Pts',(38.3514597232838,-3.18820772913842,-3.6368244020829));
#30119=CARTESIAN_POINT('Ctrl Pts',(38.4703687222788,-1.0633668228208,-4.71809401024689));
#30120=CARTESIAN_POINT('Ctrl Pts',(38.5892777212738,1.31987411178072,-4.65285856920785));
#30121=CARTESIAN_POINT('Ctrl Pts',(38.7081867202687,3.38238327089769,-3.4569702112311));
#30122=CARTESIAN_POINT('Ctrl Pts',(38.8270957192637,4.62296747233291,-1.42103229083564));
#30123=CARTESIAN_POINT('Ctrl Pts',(38.9460047182586,4.74016226456139,0.960219481684352));
#30124=CARTESIAN_POINT('Ctrl Pts',(39.0649137172536,3.70548973827946,3.10813521039484));
#30125=CARTESIAN_POINT('Ctrl Pts',(39.1838227162485,1.77037587302855,4.50077068322006));
#30126=CARTESIAN_POINT('Ctrl Pts',(39.3027317152435,-0.59494076123329,4.79970690637895));
#30127=CARTESIAN_POINT('Ctrl Pts',(39.4216407142385,-2.81568908104751,3.93231408668901));
#30128=CARTESIAN_POINT('Ctrl Pts',(39.5405497132334,-4.35221337028301,2.10934579930564));
#30129=CARTESIAN_POINT('Ctrl Pts',(39.6594587122284,-4.83115544400883,-0.226164797044103));
#30130=CARTESIAN_POINT('Ctrl Pts',(39.7783677112234,-4.13609182477006,-2.50678161208584));
#30131=CARTESIAN_POINT('Ctrl Pts',(39.8972767102183,-2.43600340529342,-4.17811712717936));
#30132=CARTESIAN_POINT('Ctrl Pts',(40.0161857092132,-0.143856646546919,
-4.83442011386536));
#30133=CARTESIAN_POINT('Ctrl Pts',(40.1350947082083,2.18303761018033,-4.31543740745708));
#30134=CARTESIAN_POINT('Ctrl Pts',(40.2540037072032,3.97986861256082,-2.74881935098085));
#30135=CARTESIAN_POINT('Ctrl Pts',(40.3729127061982,4.80874939862473,-0.512191935771164));
#30136=CARTESIAN_POINT('Ctrl Pts',(40.4918217051931,4.47076141337881,1.84482806791161));
#30137=CARTESIAN_POINT('Ctrl Pts',(40.6107307041881,3.04304919662576,3.76165904263012));
#30138=CARTESIAN_POINT('Ctrl Pts',(40.7296397031831,0.88248142554386,4.74838604768767));
#30139=CARTESIAN_POINT('Ctrl Pts',(40.8881850351763,-2.30143085677862,4.56497397532002));
#30140=CARTESIAN_POINT('Ctrl Pts',(41.086366700168,-5.29935496361248,1.41599913878779));
#30141=CARTESIAN_POINT('Ctrl Pts',(41.3241846981578,-4.05623198338425,-3.69258699130876));
#30142=CARTESIAN_POINT('Ctrl Pts',(41.5223663631495,0.0533675592095104,
-5.11201753591534));
#30143=CARTESIAN_POINT('Ctrl Pts',(41.6809116951428,2.96556576247672,-3.81200252265534));
#30144=CARTESIAN_POINT('Ctrl Pts',(41.7998206941377,4.43119083216643,-1.94287801341456));
#30145=CARTESIAN_POINT('Ctrl Pts',(41.9187296931327,4.81854226610599,0.415630419076423));
#30146=CARTESIAN_POINT('Ctrl Pts',(42.0376386921276,4.03575460661519,2.66441290212816));
#30147=CARTESIAN_POINT('Ctrl Pts',(42.1565476911226,2.27188053027963,4.27011953623197));
#30148=CARTESIAN_POINT('Ctrl Pts',(42.2754566901176,-0.0438683014249705,
4.83598271267297));
#30149=CARTESIAN_POINT('Ctrl Pts',(42.3943656891125,-2.34905543488218,4.22779506787547));
#30150=CARTESIAN_POINT('Ctrl Pts',(42.5132746881075,-4.08336865897898,2.59169359954044));
#30151=CARTESIAN_POINT('Ctrl Pts',(42.6321836871024,-4.82544086902409,0.326082893101593));
#30152=CARTESIAN_POINT('Ctrl Pts',(42.7510926860974,-4.39491009331357,-2.01890532499388));
#30153=CARTESIAN_POINT('Ctrl Pts',(42.8700016850924,-2.89641467691355,-3.87322642520138));
#30154=CARTESIAN_POINT('Ctrl Pts',(42.9889106840873,-0.694082301453685,
-4.78638160161846));
#30155=CARTESIAN_POINT('Ctrl Pts',(43.1078196830823,1.67691172765244,-4.53642016949271));
#30156=CARTESIAN_POINT('Ctrl Pts',(43.2267286820773,3.64041405093096,-3.18410945360226));
#30157=CARTESIAN_POINT('Ctrl Pts',(43.3456376810722,4.7192889865021,-1.05805016349441));
#30158=CARTESIAN_POINT('Ctrl Pts',(43.4645466800672,4.65136862352993,1.32511496686864));
#30159=CARTESIAN_POINT('Ctrl Pts',(43.5834556790621,3.45315743372404,3.3862759426488));
#30160=CARTESIAN_POINT('Ctrl Pts',(43.7023646780571,1.41582298452372,4.62456537515495));
#30161=CARTESIAN_POINT('Ctrl Pts',(43.8212736770521,-0.965558956286676,
4.73907759357604));
#30162=CARTESIAN_POINT('Ctrl Pts',(43.940182676047,-3.11230836591239,3.70198551116498));
#30163=CARTESIAN_POINT('Ctrl Pts',(44.059091675042,-4.50276139379784,1.76530453073892));
#30164=CARTESIAN_POINT('Ctrl Pts',(44.1780006740369,-4.79903550770774,-0.600348579768053));
#30165=CARTESIAN_POINT('Ctrl Pts',(44.2969096730319,-3.92913558336424,-2.82011591559274));
#30166=CARTESIAN_POINT('Ctrl Pts',(44.4158186720268,-2.10444882473593,-4.35459014980295));
#30167=CARTESIAN_POINT('Ctrl Pts',(44.5347276710218,0.231622686454836,-4.83089134074941));
#30168=CARTESIAN_POINT('Ctrl Pts',(44.6536366700168,2.51140947906087,-4.13327747082228));
#30169=CARTESIAN_POINT('Ctrl Pts',(44.7725456690117,4.1809193663156,-2.43126992982818));
#30170=CARTESIAN_POINT('Ctrl Pts',(44.8914546680067,4.83445851955282,-0.138459535064545));
#30171=CARTESIAN_POINT('Ctrl Pts',(45.0103636670017,4.31321577897907,2.18799676968153));
#30172=CARTESIAN_POINT('Ctrl Pts',(45.1292726659966,2.74385404419261,3.98276602427223));
#30173=CARTESIAN_POINT('Ctrl Pts',(45.2481816649916,0.507730967406337,4.80971615429307));
#30174=CARTESIAN_POINT('Ctrl Pts',(45.3670906639865,-1.85177162437543,4.46789682861769));
#30175=CARTESIAN_POINT('Ctrl Pts',(45.4859996629815,-3.76129046576673,3.04037074255735));
#30176=CARTESIAN_POINT('Ctrl Pts',(45.6049086619765,-4.75680913142263,0.874029237076196));
#30177=CARTESIAN_POINT('Ctrl Pts',(45.7238176609714,-4.59641484070745,-1.50470290495351));
#30178=CARTESIAN_POINT('Ctrl Pts',(45.8427266599664,-3.31908368739342,-3.51778960373314));
#30179=CARTESIAN_POINT('Ctrl Pts',(45.9616356589614,-1.2352093805618,-4.67604726304423));
#30180=CARTESIAN_POINT('Ctrl Pts',(46.0805446579563,1.1488229707437,-4.69801724155464));
#30181=CARTESIAN_POINT('Ctrl Pts',(46.1994536569513,3.2536893265738,-3.57836079597794));
#30182=CARTESIAN_POINT('Ctrl Pts',(46.3183626559463,4.56790347318454,-1.58915640505304));
#30183=CARTESIAN_POINT('Ctrl Pts',(46.4372716549412,4.77210906947758,0.786215777673183));
#30184=CARTESIAN_POINT('Ctrl Pts',(46.5561806539362,3.81668379763501,2.97053614839524));
#30185=CARTESIAN_POINT('Ctrl Pts',(46.6750896529311,1.9337976733239,4.43301102848837));
#30186=CARTESIAN_POINT('Ctrl Pts',(46.7939986519261,-0.419004675043817,
4.81825645875599));
#30187=CARTESIAN_POINT('Ctrl Pts',(46.9129076509211,-2.66998815297085,4.03265712440913));
#30188=CARTESIAN_POINT('Ctrl Pts',(47.031816649916,-4.27215982993872,2.26711504064315));
#30189=CARTESIAN_POINT('Ctrl Pts',(47.150725648911,-4.83618918025851,-0.049339971655738));
#30190=CARTESIAN_POINT('Ctrl Pts',(47.2696346479059,-4.22501608320733,-2.35380528436229));
#30191=CARTESIAN_POINT('Ctrl Pts',(47.3885436469008,-2.58715667259437,-4.08629178736698));
#30192=CARTESIAN_POINT('Ctrl Pts',(47.5074526458959,-0.320613655935554,
-4.82580222384631));
#30193=CARTESIAN_POINT('Ctrl Pts',(47.6263616448908,2.02383904106705,-4.39263426156847));
#30194=CARTESIAN_POINT('Ctrl Pts',(47.7452706438858,3.87649530383263,-2.8920484745965));
#30195=CARTESIAN_POINT('Ctrl Pts',(47.8641796428807,4.78715641328979,-0.688689839296955));
#30196=CARTESIAN_POINT('Ctrl Pts',(47.9830886418758,4.53453012369092,1.68202163404398));
#30197=CARTESIAN_POINT('Ctrl Pts',(48.1019976408707,3.18000506619605,3.64399890217051));
#30198=CARTESIAN_POINT('Ctrl Pts',(48.2209066398657,1.05273320390273,4.72047805009758));
#30199=CARTESIAN_POINT('Ctrl Pts',(48.3398156388606,-1.33035467210349,4.64987275809402));
#30200=CARTESIAN_POINT('Ctrl Pts',(48.4587246378556,-3.39016403102658,3.44934023586916));
#30201=CARTESIAN_POINT('Ctrl Pts',(48.5776336368505,-4.62615758834401,1.41061199054156));
#30202=CARTESIAN_POINT('Ctrl Pts',(48.6965426358455,-4.73798674325583,-0.97089744091966));
#30203=CARTESIAN_POINT('Ctrl Pts',(48.8154516348404,-3.69847681511145,-3.11647709250932));
#30204=CARTESIAN_POINT('Ctrl Pts',(48.9343606338354,-1.76023053843739,-4.50474734825446));
#30205=CARTESIAN_POINT('Ctrl Pts',(49.0532696328304,0.605754844298045,-4.79835610273556));
#30206=CARTESIAN_POINT('Ctrl Pts',(49.1721786318254,2.8245407381406,-3.92595591399616));
#30207=CARTESIAN_POINT('Ctrl Pts',(49.2910876308202,4.35695828193666,-2.09954155698525));
#30208=CARTESIAN_POINT('Ctrl Pts',(49.4099966298153,4.83062732662176,0.23706507831365));
#30209=CARTESIAN_POINT('Ctrl Pts',(49.5289056288102,4.13044546411404,2.51606448407709));
#30210=CARTESIAN_POINT('Ctrl Pts',(49.6478146278052,2.42655811424978,4.18365581019525));
#30211=CARTESIAN_POINT('Ctrl Pts',(49.7667236268001,0.133012889488217,4.83461144161723));
#30212=CARTESIAN_POINT('Ctrl Pts',(49.8856326257951,-2.19285470052332,4.31074801886369));
#30213=CARTESIAN_POINT('Ctrl Pts',(50.0045416247901,-3.98585475487434,2.7393652720375));
#30214=CARTESIAN_POINT('Ctrl Pts',(50.123450623785,-4.81028511750694,0.502311962481408));
#30215=CARTESIAN_POINT('Ctrl Pts',(50.24235962278,-4.46580776567652,-1.85680403390435));
#30216=CARTESIAN_POINT('Ctrl Pts',(50.361268621775,-3.03613129888863,-3.76471339650777));
#30217=CARTESIAN_POINT('Ctrl Pts',(50.4801776207699,-0.868669605950452,
-4.75779080332068));
#30218=CARTESIAN_POINT('Ctrl Pts',(50.5990866197649,1.50988032581682,-4.59471670953278));
#30219=CARTESIAN_POINT('Ctrl Pts',(50.7179956187599,3.52152668793086,-3.31511839449318));
#30220=CARTESIAN_POINT('Ctrl Pts',(50.8369046177548,4.67743590065847,-1.22994051403022));
#30221=CARTESIAN_POINT('Ctrl Pts',(50.9558136167497,4.69671997507175,1.15411509696296));
#30222=CARTESIAN_POINT('Ctrl Pts',(51.0747226157447,3.57469289561859,3.25771865697702));
#30223=CARTESIAN_POINT('Ctrl Pts',(51.1936316147397,1.58400911282353,4.56969099221527));
#30224=CARTESIAN_POINT('Ctrl Pts',(51.3125406137346,-0.791591532664319,
4.77122016992817));
#30225=CARTESIAN_POINT('Ctrl Pts',(51.4314496127296,-2.97483430372514,3.81333495628239));
#30226=CARTESIAN_POINT('Ctrl Pts',(51.5503586117245,-4.43518661532507,1.92880172176646));
#30227=CARTESIAN_POINT('Ctrl Pts',(51.6692676107195,-4.81778182205635,-0.424431831441317));
#30228=CARTESIAN_POINT('Ctrl Pts',(51.7881766097145,-4.02964557443573,-2.67453145635796));
#30229=CARTESIAN_POINT('Ctrl Pts',(51.9070856087094,-2.26230243301161,-4.27470776842447));
#30230=CARTESIAN_POINT('Ctrl Pts',(52.0259946077044,0.0547922305479365,
-4.83613752262923));
#30231=CARTESIAN_POINT('Ctrl Pts',(52.1449036066994,2.35855619782664,-4.22234761718183));
#30232=CARTESIAN_POINT('Ctrl Pts',(52.2638126056944,4.08921896687908,-2.58257921927111));
#30233=CARTESIAN_POINT('Ctrl Pts',(52.3827216046893,4.82613032653762,-0.315120994319956));
#30234=CARTESIAN_POINT('Ctrl Pts',(52.5016306036843,4.39041156062324,2.02867426848899));
#30235=CARTESIAN_POINT('Ctrl Pts',(52.6205396026792,2.8875560619597,3.87999003345837));
#30236=CARTESIAN_POINT('Ctrl Pts',(52.6998122686759,1.41823783518537,4.48478122234856));
#30237=CARTESIAN_POINT('Ctrl Pts',(52.7394486016742,0.655566364250171,4.59362378047095));
#30238=CARTESIAN_POINT('Ctrl Pts',(29.8355513983258,2.52761008811556,-3.54684587865062));
#30239=CARTESIAN_POINT('Ctrl Pts',(29.8751877313241,3.11648682089265,-3.12719111457326));
#30240=CARTESIAN_POINT('Ctrl Pts',(29.9544603973208,4.08058760393856,-1.98932416832584));
#30241=CARTESIAN_POINT('Ctrl Pts',(30.0733693963157,4.53506113804012,0.202197673507152));
#30242=CARTESIAN_POINT('Ctrl Pts',(30.1922783953107,3.88750306547132,2.34406332861471));
#30243=CARTESIAN_POINT('Ctrl Pts',(30.3111873943056,2.29527904074611,3.9165710335624));
#30244=CARTESIAN_POINT('Ctrl Pts',(30.4300963933006,0.145295930459194,4.53721866535562));
#30245=CARTESIAN_POINT('Ctrl Pts',(30.5490053922956,-2.0399931999599,4.05537755177054));
#30246=CARTESIAN_POINT('Ctrl Pts',(30.6679143912905,-3.72956098272885,2.5880408323952));
#30247=CARTESIAN_POINT('Ctrl Pts',(30.7868233902855,-4.51283862113539,0.491821573360237));
#30248=CARTESIAN_POINT('Ctrl Pts',(30.9057323892805,-4.19948870949138,-1.72391917081437));
#30249=CARTESIAN_POINT('Ctrl Pts',(31.0246413882754,-2.86565560829363,-3.5207405337779));
#30250=CARTESIAN_POINT('Ctrl Pts',(31.1435503872704,-0.835463207911184,
-4.46201778204743));
#30251=CARTESIAN_POINT('Ctrl Pts',(31.2624593862653,1.39774823457573,-4.31901588286307));
#30252=CARTESIAN_POINT('Ctrl Pts',(31.3813683852603,3.29130439703369,-3.12648605823298));
#30253=CARTESIAN_POINT('Ctrl Pts',(31.5002773842552,4.38506782680442,-1.17421438877115));
#30254=CARTESIAN_POINT('Ctrl Pts',(31.6191863832503,4.41325208649288,1.06339330852454));
#30255=CARTESIAN_POINT('Ctrl Pts',(31.7380953822452,3.36900835504494,3.0425946315337));
#30256=CARTESIAN_POINT('Ctrl Pts',(31.8570043812402,1.50608968775765,4.28244009435932));
#30257=CARTESIAN_POINT('Ctrl Pts',(31.9759133802351,-0.722811413144461,
4.48164512423311));
#30258=CARTESIAN_POINT('Ctrl Pts',(32.0948223792301,-2.77606807389926,3.5918025257666));
#30259=CARTESIAN_POINT('Ctrl Pts',(32.213731378225,-4.15473532690629,1.8291456220671));
#30260=CARTESIAN_POINT('Ctrl Pts',(32.33264037722,-4.52379461335287,-0.377996875818372));
#30261=CARTESIAN_POINT('Ctrl Pts',(32.451549376215,-3.79356387971383,-2.49328546934199));
#30262=CARTESIAN_POINT('Ctrl Pts',(32.5704583752099,-2.14149047419338,-4.00270132424737));
#30263=CARTESIAN_POINT('Ctrl Pts',(32.6893673742049,0.0309688700304269,
-4.539453741424));
#30264=CARTESIAN_POINT('Ctrl Pts',(32.8082763731999,2.19590272455425,-3.9731109430928));
#30265=CARTESIAN_POINT('Ctrl Pts',(32.9271853721948,3.82722836817241,-2.44129522170742));
#30266=CARTESIAN_POINT('Ctrl Pts',(33.0460943711898,4.52853081019897,-0.316240482530403));
#30267=CARTESIAN_POINT('Ctrl Pts',(33.1650033701847,4.12939232802359,1.88566124820393));
#30268=CARTESIAN_POINT('Ctrl Pts',(33.2839123691797,2.72680427239924,3.62934399054829));
#30269=CARTESIAN_POINT('Ctrl Pts',(33.4028213681747,0.66159799921097,4.49108978190761));
#30270=CARTESIAN_POINT('Ctrl Pts',(33.5217303671696,-1.56437774739295,4.26149288456175));
#30271=CARTESIAN_POINT('Ctrl Pts',(33.6406393661646,-3.41020695943747,2.99634574699176));
#30272=CARTESIAN_POINT('Ctrl Pts',(33.7595483651595,-4.42734990314248,1.00308134109595));
#30273=CARTESIAN_POINT('Ctrl Pts',(33.8784573641545,-4.36863906040348,-1.23393358882379));
#30274=CARTESIAN_POINT('Ctrl Pts',(33.9973663631495,-3.24834126891074,-3.17110049389832));
#30275=CARTESIAN_POINT('Ctrl Pts',(34.1162753621444,-1.33869085558447,-4.33768442085004));
#30276=CARTESIAN_POINT('Ctrl Pts',(34.2351843611394,0.896263782021944,-4.45020343071488));
#30277=CARTESIAN_POINT('Ctrl Pts',(34.3540933601343,2.91342474968224,-3.48131520687938));
#30278=CARTESIAN_POINT('Ctrl Pts',(34.4730023591293,4.22261839670216,-1.66646128594193));
#30279=CARTESIAN_POINT('Ctrl Pts',(34.5919113581243,4.50570837218357,0.553345648347923));
#30280=CARTESIAN_POINT('Ctrl Pts',(34.7108203571193,3.69390331590221,2.63868862021977));
#30281=CARTESIAN_POINT('Ctrl Pts',(34.8297293561142,1.98447327941527,4.08282563245083));
#30282=CARTESIAN_POINT('Ctrl Pts',(34.9486383551092,-0.207187242229502,
4.53482885987642));
#30283=CARTESIAN_POINT('Ctrl Pts',(35.0675473541041,-2.34850090086774,3.88486072598929));
#30284=CARTESIAN_POINT('Ctrl Pts',(35.1864563530991,-3.91912472429048,2.29086462654731));
#30285=CARTESIAN_POINT('Ctrl Pts',(35.305365352094,-4.53739437051538,0.140184407570935));
#30286=CARTESIAN_POINT('Ctrl Pts',(35.424274351089,-4.05306923184566,-2.04456086815158));
#30287=CARTESIAN_POINT('Ctrl Pts',(35.543183350084,-2.58384116587268,-3.73247426933561));
#30288=CARTESIAN_POINT('Ctrl Pts',(35.6620923490789,-0.486735167798389,
-4.51338988102501));
#30289=CARTESIAN_POINT('Ctrl Pts',(35.7810013480739,1.72864832916969,-4.19754384083949));
#30290=CARTESIAN_POINT('Ctrl Pts',(35.8999103470689,3.52396725228349,-2.8616872901392));
#30291=CARTESIAN_POINT('Ctrl Pts',(36.0188193460638,4.46295595650429,-0.830435712149652));
#30292=CARTESIAN_POINT('Ctrl Pts',(36.1377283450588,4.31743854090615,1.40261319942774));
#30293=CARTESIAN_POINT('Ctrl Pts',(36.2566373440538,3.12277599253313,3.29482464513204));
#30294=CARTESIAN_POINT('Ctrl Pts',(36.3755463430487,1.16927340456928,4.38638792710784));
#30295=CARTESIAN_POINT('Ctrl Pts',(36.4944553420437,-1.06836467013381,4.41205125461175));
#30296=CARTESIAN_POINT('Ctrl Pts',(36.6133643410386,-3.04638825743189,3.3655783940789));
#30297=CARTESIAN_POINT('Ctrl Pts',(36.7322733400336,-4.28413415865655,1.5012640848113));
#30298=CARTESIAN_POINT('Ctrl Pts',(36.8511823390286,-4.48082795036645,-0.727860028387663));
#30299=CARTESIAN_POINT('Ctrl Pts',(36.9700913380235,-3.58867269642476,-2.78011287893923));
#30300=CARTESIAN_POINT('Ctrl Pts',(37.0890003370185,-1.82446368725053,-4.15679342710547));
#30301=CARTESIAN_POINT('Ctrl Pts',(37.2079093360134,0.383093195727588,-4.52336588671137));
#30302=CARTESIAN_POINT('Ctrl Pts',(37.3268183350084,2.49755776068852,-3.79075250759061));
#30303=CARTESIAN_POINT('Ctrl Pts',(37.4457273340033,4.00511141222751,-2.13697962490221));
#30304=CARTESIAN_POINT('Ctrl Pts',(37.5646363329983,4.5394159707129,0.036083052139815));
#30305=CARTESIAN_POINT('Ctrl Pts',(37.6835453319933,3.97063449186246,2.20037748438958));
#30306=CARTESIAN_POINT('Ctrl Pts',(37.8024543309883,2.43698187211053,3.82997633100645));
#30307=CARTESIAN_POINT('Ctrl Pts',(37.9213633299832,0.31113838584895,4.52888421673187));
#30308=CARTESIAN_POINT('Ctrl Pts',(38.0402723289782,-1.8903122731222,4.12726529888137));
#30309=CARTESIAN_POINT('Ctrl Pts',(38.1591813279731,-3.63241373729313,2.72271368132007));
#30310=CARTESIAN_POINT('Ctrl Pts',(38.2780903269681,-4.49183229506202,0.6565378631504));
#30311=CARTESIAN_POINT('Ctrl Pts',(38.3969993259631,-4.25972773526838,-1.56917779883104));
#30312=CARTESIAN_POINT('Ctrl Pts',(38.515908324958,-2.9925018633614,-3.41358052064332));
#30313=CARTESIAN_POINT('Ctrl Pts',(38.634817323953,-0.998092806075667,-4.42847716230638));
#30314=CARTESIAN_POINT('Ctrl Pts',(38.753726322948,1.23885457738782,-4.36724615245642));
#30315=CARTESIAN_POINT('Ctrl Pts',(38.8726353219429,3.17475807747922,-3.24476655148489));
#30316=CARTESIAN_POINT('Ctrl Pts',(38.9915443209379,4.33918989932127,-1.33380323350872));
#30317=CARTESIAN_POINT('Ctrl Pts',(39.1104533199328,4.44919077251242,0.901277091174026));
#30318=CARTESIAN_POINT('Ctrl Pts',(39.2293623189278,3.47803088397395,2.91734453927799));
#30319=CARTESIAN_POINT('Ctrl Pts',(39.3482713179227,1.66170260816715,4.22449407326989));
#30320=CARTESIAN_POINT('Ctrl Pts',(39.4671803169177,-0.558420745395243,
4.50508030880696));
#30321=CARTESIAN_POINT('Ctrl Pts',(39.5860893159126,-2.64285000775597,3.69093178094741));
#30322=CARTESIAN_POINT('Ctrl Pts',(39.7049983149076,-4.08505584541632,1.97986510640618));
#30323=CARTESIAN_POINT('Ctrl Pts',(39.8239073139026,-4.53459840030311,-0.212281831699906));
#30324=CARTESIAN_POINT('Ctrl Pts',(39.9428163128976,-3.88220076738949,-2.35290460425372));
#30325=CARTESIAN_POINT('Ctrl Pts',(40.0617253118925,-2.2864710673872,-3.92164637647539));
#30326=CARTESIAN_POINT('Ctrl Pts',(40.1806343108875,-0.135026108529271,
-4.5376626707205));
#30327=CARTESIAN_POINT('Ctrl Pts',(40.2995433098824,2.0490333978389,-4.05053734893388));
#30328=CARTESIAN_POINT('Ctrl Pts',(40.4184523088774,3.73556720604287,-2.58008502854894));
#30329=CARTESIAN_POINT('Ctrl Pts',(40.5373613078723,4.51356773409222,-0.480751397779228));
#30330=CARTESIAN_POINT('Ctrl Pts',(40.6562703068674,4.19632690113196,1.73158460797626));
#30331=CARTESIAN_POINT('Ctrl Pts',(40.7751793058622,2.8562537842112,3.53075227549335));
#30332=CARTESIAN_POINT('Ctrl Pts',(40.8940883048572,0.828310930365704,4.45690974455567));
#30333=CARTESIAN_POINT('Ctrl Pts',(41.0526336368505,-2.16015915913004,4.28475629190986));
#30334=CARTESIAN_POINT('Ctrl Pts',(41.2508153018422,-4.9740578251184,1.32907903792256));
#30335=CARTESIAN_POINT('Ctrl Pts',(41.488633299832,-3.80724306561534,-3.46592016295684));
#30336=CARTESIAN_POINT('Ctrl Pts',(41.6868149648236,0.0500916295127203,
-4.79821997229049));
#30337=CARTESIAN_POINT('Ctrl Pts',(41.845360296817,2.7835266156044,-3.57800545677343));
#30338=CARTESIAN_POINT('Ctrl Pts',(41.9642692958118,4.15918533192678,-1.82361582725293));
#30339=CARTESIAN_POINT('Ctrl Pts',(42.0831782948069,4.52275947336236,0.390117241166111));
#30340=CARTESIAN_POINT('Ctrl Pts',(42.2020872938018,3.78802267806716,2.5008598095763));
#30341=CARTESIAN_POINT('Ctrl Pts',(42.3209962927968,2.13242275842343,4.00800128302914));
#30342=CARTESIAN_POINT('Ctrl Pts',(42.4399052917917,-0.0411754769167031,
4.53912935051075));
#30343=CARTESIAN_POINT('Ctrl Pts',(42.5588142907867,-2.20486033635077,3.96827487208511));
#30344=CARTESIAN_POINT('Ctrl Pts',(42.6777232897817,-3.8327139756632,2.43260432970045));
#30345=CARTESIAN_POINT('Ctrl Pts',(42.7966322887766,-4.52923461044278,0.306066526436917));
#30346=CARTESIAN_POINT('Ctrl Pts',(42.9155412877716,-4.12513166044574,-1.89497625633923));
#30347=CARTESIAN_POINT('Ctrl Pts',(43.0344502867665,-2.71862032028679,-3.63547117357001));
#30348=CARTESIAN_POINT('Ctrl Pts',(43.1533592857615,-0.651476552623365,
-4.49257296840967));
#30349=CARTESIAN_POINT('Ctrl Pts',(43.2722682847565,1.57397569293539,-4.25795524116172));
#30350=CARTESIAN_POINT('Ctrl Pts',(43.3911772837514,3.4169498214478,-2.98865515755662));
#30351=CARTESIAN_POINT('Ctrl Pts',(43.5100862827464,4.42959878579337,-0.993102506103781));
#30352=CARTESIAN_POINT('Ctrl Pts',(43.6289952817414,4.36584766603513,1.24377372631055));
#30353=CARTESIAN_POINT('Ctrl Pts',(43.7479042807363,3.24118781861557,3.17841180034119));
#30354=CARTESIAN_POINT('Ctrl Pts',(43.8668132797312,1.32891369676281,4.34068971601413));
#30355=CARTESIAN_POINT('Ctrl Pts',(43.9857222787263,-0.906288805922349,
4.44817268328468));
#30356=CARTESIAN_POINT('Ctrl Pts',(44.1046312777211,-2.92126152860971,3.47474176135063));
#30357=CARTESIAN_POINT('Ctrl Pts',(44.2235402767162,-4.22636258549353,1.65694256662005));
#30358=CARTESIAN_POINT('Ctrl Pts',(44.3424492757111,-4.50445012346606,-0.563496608832273));
#30359=CARTESIAN_POINT('Ctrl Pts',(44.4613582747061,-3.68794838779045,-2.64700510420854));
#30360=CARTESIAN_POINT('Ctrl Pts',(44.580267273701,-1.97526872914043,-4.08728672801447));
#30361=CARTESIAN_POINT('Ctrl Pts',(44.699176272696,0.217404692447769,-4.53435050883458));
#30362=CARTESIAN_POINT('Ctrl Pts',(44.818085271691,2.35724839290324,-3.8795591705588));
#30363=CARTESIAN_POINT('Ctrl Pts',(44.9369942706859,3.92427660215364,-2.28202815294958));
#30364=CARTESIAN_POINT('Ctrl Pts',(45.0559032696809,4.53769871890213,-0.129960294899828));
#30365=CARTESIAN_POINT('Ctrl Pts',(45.1748122686759,4.04845209354121,2.05368814285831));
#30366=CARTESIAN_POINT('Ctrl Pts',(45.2937212676708,2.57542451358934,3.7382867621954));
#30367=CARTESIAN_POINT('Ctrl Pts',(45.4126302666658,0.476564262787324,4.51447514615088));
#30368=CARTESIAN_POINT('Ctrl Pts',(45.5315392656607,-1.73810193916093,4.1936381568707));
#30369=CARTESIAN_POINT('Ctrl Pts',(45.6504482646557,-3.5304063234588,2.85373974514235));
#30370=CARTESIAN_POINT('Ctrl Pts',(45.7693572636506,-4.46481578328136,0.820377573480641));
#30371=CARTESIAN_POINT('Ctrl Pts',(45.8882662626457,-4.31426718211871,-1.41233778643891));
#30372=CARTESIAN_POINT('Ctrl Pts',(46.0071752616405,-3.11534409392495,-3.30185258879907));
#30373=CARTESIAN_POINT('Ctrl Pts',(46.1260842606356,-1.15938693052836,-4.38901142480054));
#30374=CARTESIAN_POINT('Ctrl Pts',(46.2449932596305,1.07830328908713,-4.40963279179289));
#30375=CARTESIAN_POINT('Ctrl Pts',(46.3639022586255,3.05396391947226,-3.35870566145235));
#30376=CARTESIAN_POINT('Ctrl Pts',(46.4828112576204,4.28750596462981,-1.49160716845105));
#30377=CARTESIAN_POINT('Ctrl Pts',(46.6017202566154,4.47917654551159,0.737954480879145));
#30378=CARTESIAN_POINT('Ctrl Pts',(46.7206292556103,3.58239937501518,2.78819189791547));
#30379=CARTESIAN_POINT('Ctrl Pts',(46.8395382546053,1.81509287738585,4.160893796791));
#30380=CARTESIAN_POINT('Ctrl Pts',(46.9584472536003,-0.393284370828836,
4.52249121009344));
#30381=CARTESIAN_POINT('Ctrl Pts',(47.0773562525952,-2.50609282760802,3.78511533260512));
#30382=CARTESIAN_POINT('Ctrl Pts',(47.1962652515902,-4.00991633475661,2.12794979498173));
#30383=CARTESIAN_POINT('Ctrl Pts',(47.3151742505851,-4.53932314423028,-0.0463112725587562));
#30384=CARTESIAN_POINT('Ctrl Pts',(47.4340832495801,-3.96566647341596,-2.20931861969599));
#30385=CARTESIAN_POINT('Ctrl Pts',(47.5529922485751,-2.42834589879083,-3.83545766989239));
#30386=CARTESIAN_POINT('Ctrl Pts',(47.67190124757,-0.300933014507645,-4.52957378375604));
#30387=CARTESIAN_POINT('Ctrl Pts',(47.790810246565,1.89960711975736,-4.12299552901502));
#30388=CARTESIAN_POINT('Ctrl Pts',(47.90971924556,3.63853939440949,-2.71452213419616));
#30389=CARTESIAN_POINT('Ctrl Pts',(48.0286282445549,4.49330021881717,-0.646415102924012));
#30390=CARTESIAN_POINT('Ctrl Pts',(48.1475372435499,4.25618121447832,1.5787719313544));
#30391=CARTESIAN_POINT('Ctrl Pts',(48.2664462425448,2.98480271505459,3.42031461914156));
#30392=CARTESIAN_POINT('Ctrl Pts',(48.3853552415398,0.988111924298174,4.43071485956504));
#30393=CARTESIAN_POINT('Ctrl Pts',(48.5042642405347,-1.24869179596311,4.36444362323597));
#30394=CARTESIAN_POINT('Ctrl Pts',(48.6231732395298,-3.18206122117694,3.23760493673836));
#30395=CARTESIAN_POINT('Ctrl Pts',(48.7420822385247,-4.34218419232808,1.32402257594309));
#30396=CARTESIAN_POINT('Ctrl Pts',(48.8609912375196,-4.44714879403618,-0.911299591469888));
#30397=CARTESIAN_POINT('Ctrl Pts',(48.9799002365147,-3.47144844411091,-2.92517436088697));
#30398=CARTESIAN_POINT('Ctrl Pts',(49.0988092355095,-1.65218003773015,-4.22822663354714));
#30399=CARTESIAN_POINT('Ctrl Pts',(49.2177182345046,0.568571013656015,-4.50381242328528));
#30400=CARTESIAN_POINT('Ctrl Pts',(49.3366272334995,2.65115831216877,-3.68496390016692));
#30401=CARTESIAN_POINT('Ctrl Pts',(49.4555362324945,4.08950949404005,-1.97066269053332));
#30402=CARTESIAN_POINT('Ctrl Pts',(49.5744452314894,4.53410270102655,0.222513006949929));
#30403=CARTESIAN_POINT('Ctrl Pts',(49.6933542304844,3.8769010045698,2.36161765374458));
#30404=CARTESIAN_POINT('Ctrl Pts',(49.8122632294793,2.27760556882206,3.92684507137038));
#30405=CARTESIAN_POINT('Ctrl Pts',(49.9311722284743,0.124847987791581,4.53784225395429));
#30406=CARTESIAN_POINT('Ctrl Pts',(50.0500812274693,-2.05824787306763,4.04613581512682));
#30407=CARTESIAN_POINT('Ctrl Pts',(50.1689902264642,-3.74118589326448,2.57121128152305));
#30408=CARTESIAN_POINT('Ctrl Pts',(50.2878992254592,-4.5150091839622,0.471477899628734));
#30409=CARTESIAN_POINT('Ctrl Pts',(50.4068082244542,-4.19167732957359,-1.74282543780715));
#30410=CARTESIAN_POINT('Ctrl Pts',(50.5257172234491,-2.84976053671051,-3.53361914002879));
#30411=CARTESIAN_POINT('Ctrl Pts',(50.6446262224441,-0.815346939502767,
-4.46573719594757));
#30412=CARTESIAN_POINT('Ctrl Pts',(50.763535221439,1.41719739500182,-4.31267328951943));
#30413=CARTESIAN_POINT('Ctrl Pts',(50.882444220434,3.30536027473904,-3.11162220771148));
#30414=CARTESIAN_POINT('Ctrl Pts',(51.001353219429,4.39031482188165,-1.15444148962456));
#30415=CARTESIAN_POINT('Ctrl Pts',(51.1202622184239,4.40841515709115,1.08327056189923));
#30416=CARTESIAN_POINT('Ctrl Pts',(51.2391712174189,3.35526291255,3.05774591229208));
#30417=CARTESIAN_POINT('Ctrl Pts',(51.3580802164139,1.48677583909716,4.28918375807513));
#30418=CARTESIAN_POINT('Ctrl Pts',(51.4769892154088,-0.74300024897039,4.47834221042933));
#30419=CARTESIAN_POINT('Ctrl Pts',(51.5958982144038,-2.7922262140349,3.57925609990917));
#30420=CARTESIAN_POINT('Ctrl Pts',(51.7148072133987,-4.1629358367758,1.81040359876443));
#30421=CARTESIAN_POINT('Ctrl Pts',(51.8337162123937,-4.52204570863031,-0.398378385087645));
#30422=CARTESIAN_POINT('Ctrl Pts',(51.9526252113887,-3.7822886444867,-2.51035724354537));
#30423=CARTESIAN_POINT('Ctrl Pts',(52.0715342103836,-2.12343260584961,-4.01230786984909));
#30424=CARTESIAN_POINT('Ctrl Pts',(52.1904432093786,0.0514288484134658,
-4.53927465756786));
#30425=CARTESIAN_POINT('Ctrl Pts',(52.3093522083735,2.21377790171352,-3.96316180928111));
#30426=CARTESIAN_POINT('Ctrl Pts',(52.4282612073685,3.83820516657033,-2.42404942918688));
#30427=CARTESIAN_POINT('Ctrl Pts',(52.5471702063634,4.5298817460968,-0.295777516022001));
#30428=CARTESIAN_POINT('Ctrl Pts',(52.6660792053584,4.12090926698776,1.90414554018012));
#30429=CARTESIAN_POINT('Ctrl Pts',(52.7849882043534,2.71030548511656,3.64181960254066));
#30430=CARTESIAN_POINT('Ctrl Pts',(52.86426087035,1.33118031353268,4.20948611409119));
#30431=CARTESIAN_POINT('Ctrl Pts',(52.9038972033484,0.615324888854025,4.31164744913139));
#30432=CARTESIAN_POINT('Ctrl Pts',(30.,2.36230756092327,-3.31488661006749));
#30433=CARTESIAN_POINT('Ctrl Pts',(30.0396363329983,2.91267249451483,-2.92267674082436));
#30434=CARTESIAN_POINT('Ctrl Pts',(30.118908998995,3.81372229645613,-1.85922486464953));
#30435=CARTESIAN_POINT('Ctrl Pts',(30.2378179979899,4.23847383186721,0.18897419945147));
#30436=CARTESIAN_POINT('Ctrl Pts',(30.3567269969849,3.63326524445147,2.1907645291121));
#30437=CARTESIAN_POINT('Ctrl Pts',(30.4756359959799,2.14517067243769,3.66043220391454));
#30438=CARTESIAN_POINT('Ctrl Pts',(30.5945449949748,0.135793758977664,4.24049025960433));
#30439=CARTESIAN_POINT('Ctrl Pts',(30.7134539939698,-1.90658020521281,3.79016095005708));
#30440=CARTESIAN_POINT('Ctrl Pts',(30.8323629929647,-3.48565237567683,2.4187862103776));
#30441=CARTESIAN_POINT('Ctrl Pts',(30.9512719919597,-4.21770463967511,0.459657059780211));
#30442=CARTESIAN_POINT('Ctrl Pts',(31.0701809909547,-3.92484741894642,-1.611177020848));
#30443=CARTESIAN_POINT('Ctrl Pts',(31.1890899899496,-2.67824532838493,-3.29048852198293));
#30444=CARTESIAN_POINT('Ctrl Pts',(31.3079989889446,-0.780824962758849,
-4.1702074196749));
#30445=CARTESIAN_POINT('Ctrl Pts',(31.4269079879395,1.30633725444068,-4.03655766520605));
#30446=CARTESIAN_POINT('Ctrl Pts',(31.5458169869345,3.07605722060134,-2.92201779428377));
#30447=CARTESIAN_POINT('Ctrl Pts',(31.6647259859295,4.09828989491981,-1.09742224157957));
#30448=CARTESIAN_POINT('Ctrl Pts',(31.7836349849244,4.12463093940056,0.993848720882264));
#30449=CARTESIAN_POINT('Ctrl Pts',(31.9025439839194,3.14867943729,2.84361276159299));
#30450=CARTESIAN_POINT('Ctrl Pts',(32.0214529829143,1.40759331257097,4.00237388736178));
#30451=CARTESIAN_POINT('Ctrl Pts',(32.1403619819093,-0.675540453973202,
4.18855115831721));
#30452=CARTESIAN_POINT('Ctrl Pts',(32.2592709809043,-2.59451670629275,3.35690314889015));
#30453=CARTESIAN_POINT('Ctrl Pts',(32.3781799798992,-3.88302085140948,1.70952179426543));
#30454=CARTESIAN_POINT('Ctrl Pts',(32.4970889788942,-4.22794412375315,-0.353276354588732));
#30455=CARTESIAN_POINT('Ctrl Pts',(32.6159979778891,-3.54546956353323,-2.33022772913439));
#30456=CARTESIAN_POINT('Ctrl Pts',(32.7349069768841,-2.00143968510732,-3.74092968169653));
#30457=CARTESIAN_POINT('Ctrl Pts',(32.8538159758791,0.0289435448015357,
-4.24257916450323));
#30458=CARTESIAN_POINT('Ctrl Pts',(32.972724974874,2.05229344259103,-3.71327447432861));
#30459=CARTESIAN_POINT('Ctrl Pts',(33.091633973869,3.57693243670117,-2.28163757843869));
#30460=CARTESIAN_POINT('Ctrl Pts',(33.2105429728639,4.23237057927023,-0.295558751907219));
#30461=CARTESIAN_POINT('Ctrl Pts',(33.3294519718589,3.85933525284402,1.76234136938946));
#30462=CARTESIAN_POINT('Ctrl Pts',(33.4483609708539,2.54847469557654,3.39198944899592));
#30463=CARTESIAN_POINT('Ctrl Pts',(33.5672699698489,0.618330320477916,4.19737814723441));
#30464=CARTESIAN_POINT('Ctrl Pts',(33.6861789688438,-1.46206940626736,3.98279659879273));
#30465=CARTESIAN_POINT('Ctrl Pts',(33.8050879678388,-3.18718370466638,2.80038849605003));
#30466=CARTESIAN_POINT('Ctrl Pts',(33.9239969668337,-4.13780677653638,0.937481080421928));
#30467=CARTESIAN_POINT('Ctrl Pts',(34.0429059658287,-4.08293554922066,-1.15323588090632));
#30468=CARTESIAN_POINT('Ctrl Pts',(34.1618149648236,-3.03590382713174,-2.96371450185516));
#30469=CARTESIAN_POINT('Ctrl Pts',(34.2807239638186,-1.25114215390858,-4.05400530424081));
#30470=CARTESIAN_POINT('Ctrl Pts',(34.3996329628135,0.837649255637629,-4.15916571209051));
#30471=CARTESIAN_POINT('Ctrl Pts',(34.5185419618086,2.72289042788497,-3.25364156197822));
#30472=CARTESIAN_POINT('Ctrl Pts',(34.6374509608034,3.94646445364522,-1.55747680952698));
#30473=CARTESIAN_POINT('Ctrl Pts',(34.7563599597985,4.21104070005508,0.517157537486679));
#30474=CARTESIAN_POINT('Ctrl Pts',(34.8752689587934,3.45232667550434,2.46612169644987));
#30475=CARTESIAN_POINT('Ctrl Pts',(34.9941779577884,1.85469121778504,3.8158139607128));
#30476=CARTESIAN_POINT('Ctrl Pts',(35.1130869567833,-0.193637456642115,
4.23825674440386));
#30477=CARTESIAN_POINT('Ctrl Pts',(35.2319959557783,-2.19491188970968,3.63079571065499));
#30478=CARTESIAN_POINT('Ctrl Pts',(35.3509049547733,-3.66281888647431,2.14104495538666));
#30479=CARTESIAN_POINT('Ctrl Pts',(35.4698139537682,-4.24065447386718,0.131016523270486));
#30480=CARTESIAN_POINT('Ctrl Pts',(35.5887229527632,-3.78800359135796,-1.91084915363794));
#30481=CARTESIAN_POINT('Ctrl Pts',(35.7076319517581,-2.41486119677437,-3.48837513699617));
#30482=CARTESIAN_POINT('Ctrl Pts',(35.8265409507531,-0.454903298757822,
-4.21821984785987));
#30483=CARTESIAN_POINT('Ctrl Pts',(35.9454499497481,1.61559689818276,-3.92302974226322));
#30484=CARTESIAN_POINT('Ctrl Pts',(36.064358948743,3.29350421714833,-2.6745365332569));
#30485=CARTESIAN_POINT('Ctrl Pts',(36.183267947738,4.17108423869985,-0.776126258909775));
#30486=CARTESIAN_POINT('Ctrl Pts',(36.3021769467329,4.03508347943329,1.31088405669769));
#30487=CARTESIAN_POINT('Ctrl Pts',(36.4210859457279,2.91855036222394,3.07934724889256));
#30488=CARTESIAN_POINT('Ctrl Pts',(36.5399949447229,1.09280439154274,4.09952366232033));
#30489=CARTESIAN_POINT('Ctrl Pts',(36.6589039437179,-0.998494961682174,
4.12350864041721));
#30490=CARTESIAN_POINT('Ctrl Pts',(36.7778129427128,-2.84715828911907,3.14547379146596));
#30491=CARTESIAN_POINT('Ctrl Pts',(36.8967219417078,-4.0039571619803,1.40308329800038));
#30492=CARTESIAN_POINT('Ctrl Pts',(37.0156309407027,-4.18778742659573,-0.680258896116352));
#30493=CARTESIAN_POINT('Ctrl Pts',(37.1345399396977,-3.35397800645881,-2.59829698616001));
#30494=CARTESIAN_POINT('Ctrl Pts',(37.2534489386926,-1.70514605210925,-3.88494435443889));
#30495=CARTESIAN_POINT('Ctrl Pts',(37.3723579376876,0.358039381572612,-4.22754343529587));
#30496=CARTESIAN_POINT('Ctrl Pts',(37.4912669366826,2.3342206179893,-3.54284205161814));
#30497=CARTESIAN_POINT('Ctrl Pts',(37.6101759356776,3.74318215294784,-1.99722383969792));
#30498=CARTESIAN_POINT('Ctrl Pts',(37.7290849346725,4.24254386394922,0.0337232658201172));
#30499=CARTESIAN_POINT('Ctrl Pts',(37.8479939336675,3.71095997990038,2.05647555874971));
#30500=CARTESIAN_POINT('Ctrl Pts',(37.9669029326624,2.27760631649146,3.57950068621502));
#30501=CARTESIAN_POINT('Ctrl Pts',(38.0858119316574,0.290790325944755,4.23270087345946));
#30502=CARTESIAN_POINT('Ctrl Pts',(38.2047209306524,-1.76668822311588,3.85734732873792));
#30503=CARTESIAN_POINT('Ctrl Pts',(38.3236299296473,-3.39485843815668,2.54465162401958));
#30504=CARTESIAN_POINT('Ctrl Pts',(38.4425389286423,-4.19807210096051,0.613601110964395));
#30505=CARTESIAN_POINT('Ctrl Pts',(38.5614479276372,-3.98114688804759,-1.46655554036626));
#30506=CARTESIAN_POINT('Ctrl Pts',(38.6803569266322,-2.79679599758437,-3.19033663920374));
#30507=CARTESIAN_POINT('Ctrl Pts',(38.7992659256271,-0.932818789330533,
-4.13886031436587));
#30508=CARTESIAN_POINT('Ctrl Pts',(38.9181749246222,1.15783504299492,-4.081633735705));
#30509=CARTESIAN_POINT('Ctrl Pts',(39.037083923617,2.96713288406074,-3.03256289173867));
#30510=CARTESIAN_POINT('Ctrl Pts',(39.1559929226121,4.05541232630964,-1.24657417618181));
#30511=CARTESIAN_POINT('Ctrl Pts',(39.274901921607,4.15821928046345,0.8423347006637));
#30512=CARTESIAN_POINT('Ctrl Pts',(39.393810920602,3.25057202966842,2.72655386816114));
#30513=CARTESIAN_POINT('Ctrl Pts',(39.5127199195969,1.55302934330574,3.94821746331971));
#30514=CARTESIAN_POINT('Ctrl Pts',(39.631628918592,-0.521900729557193,4.21045371123498));
#30515=CARTESIAN_POINT('Ctrl Pts',(39.7505379175868,-2.47001093446444,3.44954947520581));
#30516=CARTESIAN_POINT('Ctrl Pts',(39.8694469165819,-3.81789832054964,1.85038441350672));
#30517=CARTESIAN_POINT('Ctrl Pts',(39.9883559155767,-4.23804135659737,-0.198398866355711));
#30518=CARTESIAN_POINT('Ctrl Pts',(40.1072649145718,-3.62830971000893,-2.19902759642159));
#30519=CARTESIAN_POINT('Ctrl Pts',(40.2261739135667,-2.13693872948098,-3.66517562577142));
#30520=CARTESIAN_POINT('Ctrl Pts',(40.3450829125617,-0.126195570511627,
-4.24090522757565));
#30521=CARTESIAN_POINT('Ctrl Pts',(40.4639919115566,1.91502918549748,-3.78563729041068));
#30522=CARTESIAN_POINT('Ctrl Pts',(40.5829009105516,3.49126579952493,-2.41135070611703));
#30523=CARTESIAN_POINT('Ctrl Pts',(40.7018099095465,4.21838606955971,-0.449310859787289));
#30524=CARTESIAN_POINT('Ctrl Pts',(40.8207189085415,3.92189238888511,1.61834114804089));
#30525=CARTESIAN_POINT('Ctrl Pts',(40.9396279075364,2.66945837179664,3.2998455083566));
#30526=CARTESIAN_POINT('Ctrl Pts',(41.0585369065315,0.774140435187547,4.16543344142367));
#30527=CARTESIAN_POINT('Ctrl Pts',(41.2170822385247,-2.01888746148146,4.0045386084997));
#30528=CARTESIAN_POINT('Ctrl Pts',(41.4152639035163,-4.64876068662433,1.24215893705732));
#30529=CARTESIAN_POINT('Ctrl Pts',(41.6530819015062,-3.55825414784644,-3.23925333460491));
#30530=CARTESIAN_POINT('Ctrl Pts',(41.8512635664978,0.0468156998159277,
-4.48442240866564));
#30531=CARTESIAN_POINT('Ctrl Pts',(42.0098088984911,2.60148746873208,-3.34400839089152));
#30532=CARTESIAN_POINT('Ctrl Pts',(42.1287178974861,3.88717983168713,-1.70435364109129));
#30533=CARTESIAN_POINT('Ctrl Pts',(42.247626896481,4.22697668061874,0.364604063255797));
#30534=CARTESIAN_POINT('Ctrl Pts',(42.366535895476,3.54029074951913,2.33730671702443));
#30535=CARTESIAN_POINT('Ctrl Pts',(42.485444894471,1.99296498656723,3.7458830298263));
#30536=CARTESIAN_POINT('Ctrl Pts',(42.6043538934659,-0.0384826524084342,
4.24227598834855));
#30537=CARTESIAN_POINT('Ctrl Pts',(42.7232628924609,-2.06066523781936,3.70875467629474));
#30538=CARTESIAN_POINT('Ctrl Pts',(42.8421718914558,-3.58205929234741,2.27351505986046));
#30539=CARTESIAN_POINT('Ctrl Pts',(42.9610808904508,-4.23302835186148,0.28605015977224));
#30540=CARTESIAN_POINT('Ctrl Pts',(43.0799898894457,-3.85535322757791,-1.77104718768459));
#30541=CARTESIAN_POINT('Ctrl Pts',(43.1988988884408,-2.54082596366002,-3.39771592193865));
#30542=CARTESIAN_POINT('Ctrl Pts',(43.3178078874356,-0.608870803793044,
-4.19876433520088));
#30543=CARTESIAN_POINT('Ctrl Pts',(43.4367168864306,1.47103965821834,-3.97949031283073));
#30544=CARTESIAN_POINT('Ctrl Pts',(43.5556258854256,3.19348559196464,-2.79320086151097));
#30545=CARTESIAN_POINT('Ctrl Pts',(43.6745348844206,4.13990858508463,-0.928154848713153));
#30546=CARTESIAN_POINT('Ctrl Pts',(43.7934438834155,4.08032670854032,1.16243248575246));
#30547=CARTESIAN_POINT('Ctrl Pts',(43.9123528824105,3.0292182035071,2.97054765803357));
#30548=CARTESIAN_POINT('Ctrl Pts',(44.0312618814054,1.2420044090019,4.05681405687331));
#30549=CARTESIAN_POINT('Ctrl Pts',(44.1501708804004,-0.847018655558019,
4.15726777299333));
#30550=CARTESIAN_POINT('Ctrl Pts',(44.2690798793954,-2.73021469130703,3.24749801153628));
#30551=CARTESIAN_POINT('Ctrl Pts',(44.3879888783904,-3.94996377718922,1.54858060250118));
#30552=CARTESIAN_POINT('Ctrl Pts',(44.5068978773853,-4.20986473922438,-0.526644637896498));
#30553=CARTESIAN_POINT('Ctrl Pts',(44.6258068763802,-3.44676119221666,-2.47389429282434));
#30554=CARTESIAN_POINT('Ctrl Pts',(44.7447158753752,-1.84608863354493,-3.819983306226));
#30555=CARTESIAN_POINT('Ctrl Pts',(44.8636248743702,0.203186698440704,-4.23780967691975));
#30556=CARTESIAN_POINT('Ctrl Pts',(44.9825338733652,2.20308730674562,-3.62584087029532));
#30557=CARTESIAN_POINT('Ctrl Pts',(45.1014428723601,3.66763383799168,-2.13278637607099));
#30558=CARTESIAN_POINT('Ctrl Pts',(45.2203518713551,4.24093891825145,-0.12146105473511));
#30559=CARTESIAN_POINT('Ctrl Pts',(45.33926087035,3.78368840810334,1.91937951603509));
#30560=CARTESIAN_POINT('Ctrl Pts',(45.458169869345,2.40699498298607,3.49380750011858));
#30561=CARTESIAN_POINT('Ctrl Pts',(45.5770788683399,0.445397558168305,4.21923413800868));
#30562=CARTESIAN_POINT('Ctrl Pts',(45.6959878673349,-1.62443225394642,3.91937948512372));
#30563=CARTESIAN_POINT('Ctrl Pts',(45.8148968663298,-3.29952218115088,2.66710874772735));
#30564=CARTESIAN_POINT('Ctrl Pts',(45.9338058653249,-4.17282243514008,0.766725909885086));
#30565=CARTESIAN_POINT('Ctrl Pts',(46.0527148643198,-4.03211952352997,-1.31997266792431));
#30566=CARTESIAN_POINT('Ctrl Pts',(46.1716238633148,-2.91160450045647,-3.085915573865));
#30567=CARTESIAN_POINT('Ctrl Pts',(46.2905328623097,-1.08356448049494,-4.10197558655686));
#30568=CARTESIAN_POINT('Ctrl Pts',(46.4094418613047,1.00778360743057,-4.12124834203113));
#30569=CARTESIAN_POINT('Ctrl Pts',(46.5283508602997,2.85423851237071,-3.13905052692677));
#30570=CARTESIAN_POINT('Ctrl Pts',(46.6472598592946,4.00710845607509,-1.39405793184905));
#30571=CARTESIAN_POINT('Ctrl Pts',(46.7661688582896,4.18624402154559,0.689693184085104));
#30572=CARTESIAN_POINT('Ctrl Pts',(46.8850778572845,3.34811495239536,2.60584764743572));
#30573=CARTESIAN_POINT('Ctrl Pts',(47.0039868562795,1.6963880814478,3.88877656509363));
#30574=CARTESIAN_POINT('Ctrl Pts',(47.1228958552745,-0.367564066613851,
4.22672596143089));
#30575=CARTESIAN_POINT('Ctrl Pts',(47.2418048542694,-2.34219750224519,3.5375735408011));
#30576=CARTESIAN_POINT('Ctrl Pts',(47.3607138532643,-3.7476728395745,1.98878454932031));
#30577=CARTESIAN_POINT('Ctrl Pts',(47.4796228522594,-4.24245710820207,-0.0432825734617755));
#30578=CARTESIAN_POINT('Ctrl Pts',(47.5985318512543,-3.70631686362458,-2.06483195502968));
#30579=CARTESIAN_POINT('Ctrl Pts',(47.7174408502492,-2.2695351249873,-3.58462355241781));
#30580=CARTESIAN_POINT('Ctrl Pts',(47.8363498492442,-0.281252373079731,
-4.23334534366577));
#30581=CARTESIAN_POINT('Ctrl Pts',(47.9552588482392,1.77537519844767,-3.85335679646156));
#30582=CARTESIAN_POINT('Ctrl Pts',(48.0741678472341,3.40058348498636,-2.53699579379582));
#30583=CARTESIAN_POINT('Ctrl Pts',(48.1930768462292,4.19944402434456,-0.604140366551068));
#30584=CARTESIAN_POINT('Ctrl Pts',(48.311985845224,3.97783230526572,1.47552222866482));
#30585=CARTESIAN_POINT('Ctrl Pts',(48.4308948442191,2.78960036391312,3.19663033611261));
#30586=CARTESIAN_POINT('Ctrl Pts',(48.549803843214,0.923490644693623,4.14095166903249));
#30587=CARTESIAN_POINT('Ctrl Pts',(48.6687128422089,-1.16702891982273,4.07901448837793));
#30588=CARTESIAN_POINT('Ctrl Pts',(48.787621841204,-2.97395841132729,3.02586963760755));
#30589=CARTESIAN_POINT('Ctrl Pts',(48.9065308401988,-4.05821079631214,1.23743316134462));
#30590=CARTESIAN_POINT('Ctrl Pts',(49.0254398391939,-4.15631084481653,-0.851701742020117));
#30591=CARTESIAN_POINT('Ctrl Pts',(49.1443488381888,-3.24442007311038,-2.73387162926461));
#30592=CARTESIAN_POINT('Ctrl Pts',(49.2632578371838,-1.54412953702292,-3.95170591883982));
#30593=CARTESIAN_POINT('Ctrl Pts',(49.3821668361787,0.531387183013984,-4.209268743835));
#30594=CARTESIAN_POINT('Ctrl Pts',(49.5010758351737,2.47777588619694,-3.44397188633769));
#30595=CARTESIAN_POINT('Ctrl Pts',(49.6199848341686,3.82206070614344,-1.84178382408138));
#30596=CARTESIAN_POINT('Ctrl Pts',(49.7388938331636,4.23757807543132,0.207960935586202));
#30597=CARTESIAN_POINT('Ctrl Pts',(49.8578028321586,3.62335654502556,2.20717082341209));
#30598=CARTESIAN_POINT('Ctrl Pts',(49.9767118311535,2.12865302339433,3.6700343325455));
#30599=CARTESIAN_POINT('Ctrl Pts',(50.0956208301485,0.11668308609495,4.24107306629136));
#30600=CARTESIAN_POINT('Ctrl Pts',(50.2145298291435,-1.92364104561195,3.78152361138994));
#30601=CARTESIAN_POINT('Ctrl Pts',(50.3334388281384,-3.49651703165463,2.40305729100861));
#30602=CARTESIAN_POINT('Ctrl Pts',(50.4523478271334,-4.21973325041745,0.440643836776059));
#30603=CARTESIAN_POINT('Ctrl Pts',(50.5712568261283,-3.91754689347067,-1.62884684170996));
#30604=CARTESIAN_POINT('Ctrl Pts',(50.6901658251233,-2.66338977453238,-3.3025248835498));
#30605=CARTESIAN_POINT('Ctrl Pts',(50.8090748241182,-0.762024273055086,
-4.17368358857445));
#30606=CARTESIAN_POINT('Ctrl Pts',(50.9279838231132,1.32451446418683,-4.03062986950608));
#30607=CARTESIAN_POINT('Ctrl Pts',(51.0468928221082,3.08919386154722,-2.90812602092978));
#30608=CARTESIAN_POINT('Ctrl Pts',(51.1658018211032,4.10319374310485,-1.07894246521889));
#30609=CARTESIAN_POINT('Ctrl Pts',(51.2847108200981,4.12011033911056,1.01242602683551));
#30610=CARTESIAN_POINT('Ctrl Pts',(51.4036198190931,3.13583292948141,2.85777316760714));
#30611=CARTESIAN_POINT('Ctrl Pts',(51.522528818088,1.38954256537078,4.00867652393499));
#30612=CARTESIAN_POINT('Ctrl Pts',(51.641437817083,-0.694408965276457,4.18546425093048));
#30613=CARTESIAN_POINT('Ctrl Pts',(51.760346816078,-2.60961812434468,3.34517724353594));
#30614=CARTESIAN_POINT('Ctrl Pts',(51.8792558150729,-3.89068505822652,1.6920054757624));
#30615=CARTESIAN_POINT('Ctrl Pts',(51.9981648140678,-4.22630959520428,-0.372324938733972));
#30616=CARTESIAN_POINT('Ctrl Pts',(52.1170738130629,-3.53493171453767,-2.34618303073278));
#30617=CARTESIAN_POINT('Ctrl Pts',(52.2359828120577,-1.98456277868761,-3.74990797127371));
#30618=CARTESIAN_POINT('Ctrl Pts',(52.3548918110528,0.0480654662789952,
-4.24241179250651));
#30619=CARTESIAN_POINT('Ctrl Pts',(52.4738008100477,2.06899960560041,-3.70397600138038));
#30620=CARTESIAN_POINT('Ctrl Pts',(52.5927098090427,3.58719136626157,-2.26551963910266));
#30621=CARTESIAN_POINT('Ctrl Pts',(52.7116188080376,4.23363316565599,-0.276434037724044));
#30622=CARTESIAN_POINT('Ctrl Pts',(52.8305278070326,3.85140697335228,1.77961681187126));
#30623=CARTESIAN_POINT('Ctrl Pts',(52.9494368060276,2.53305490827344,3.40364917162295));
#30624=CARTESIAN_POINT('Ctrl Pts',(53.0287094720242,1.24412279188,3.93419100583381));
#30625=CARTESIAN_POINT('Ctrl Pts',(53.0683458050225,0.575083413457878,4.02967111779183));
#30626=CARTESIAN_POINT('Ctrl Pts',(30.,2.16858287139687,4.42210505377543));
#30627=CARTESIAN_POINT('Ctrl Pts',(30.,2.2732454182619,4.35954462947136));
#30628=CARTESIAN_POINT('Ctrl Pts',(30.,2.37542044069574,4.2931492164828));
#30629=CARTESIAN_POINT('Ctrl Pts',(30.,2.47486624462474,4.22298839050188));
#30630=CARTESIAN_POINT('Ctrl Pts',(30.,2.59306037040875,4.13960028196972));
#30631=CARTESIAN_POINT('Ctrl Pts',(30.,2.70740050030899,4.05089352415537));
#30632=CARTESIAN_POINT('Ctrl Pts',(30.,2.81758790810149,3.95719317214126));
#30633=CARTESIAN_POINT('Ctrl Pts',(30.,2.88224739785667,3.9022085139803));
#30634=CARTESIAN_POINT('Ctrl Pts',(30.,2.94547615811346,3.84550365503418));
#30635=CARTESIAN_POINT('Ctrl Pts',(30.,3.0072068344334,3.78713968990326));
#30636=CARTESIAN_POINT('Ctrl Pts',(30.,3.05048740679948,3.74621958393636));
#30637=CARTESIAN_POINT('Ctrl Pts',(30.,3.0930314592166,3.70448384550322));
#30638=CARTESIAN_POINT('Ctrl Pts',(30.,3.13481409779582,3.66195276571105));
#30639=CARTESIAN_POINT('Ctrl Pts',(30.,3.15648070225866,3.6398980531661));
#30640=CARTESIAN_POINT('Ctrl Pts',(30.,3.17794569554624,3.61762598377252));
#30641=CARTESIAN_POINT('Ctrl Pts',(30.,3.19918545149066,3.59516091321901));
#30642=CARTESIAN_POINT('Ctrl Pts',(30.,3.29689976460728,3.49180949317459));
#30643=CARTESIAN_POINT('Ctrl Pts',(30.,3.38992792611207,3.38429928307111));
#30644=CARTESIAN_POINT('Ctrl Pts',(30.,3.4779844422932,3.27294397186865));
#30645=CARTESIAN_POINT('Ctrl Pts',(30.,3.56533657345243,3.16247941829234));
#30646=CARTESIAN_POINT('Ctrl Pts',(30.,3.64779665226775,3.048230362205));
#30647=CARTESIAN_POINT('Ctrl Pts',(30.,3.72504020840627,2.93048074794443));
#30648=CARTESIAN_POINT('Ctrl Pts',(30.,3.77864078809121,2.84877234535969));
#30649=CARTESIAN_POINT('Ctrl Pts',(30.,3.82972856206389,2.7653778884916));
#30650=CARTESIAN_POINT('Ctrl Pts',(30.,3.87818055748462,2.6803883971215));
#30651=CARTESIAN_POINT('Ctrl Pts',(30.,3.8882281341706,2.66276397474986));
#30652=CARTESIAN_POINT('Ctrl Pts',(30.,3.89816232090752,2.64507095382542));
#30653=CARTESIAN_POINT('Ctrl Pts',(30.,3.90798195189534,2.62731013620557));
#30654=CARTESIAN_POINT('Ctrl Pts',(30.,3.91756757094579,2.60997257719348));
#30655=CARTESIAN_POINT('Ctrl Pts',(30.,3.92703895771373,2.59257958603053));
#30656=CARTESIAN_POINT('Ctrl Pts',(30.,3.93639534143115,2.57513213522472));
#30657=CARTESIAN_POINT('Ctrl Pts',(30.,3.96367452270595,2.52426289047277));
#30658=CARTESIAN_POINT('Ctrl Pts',(30.,3.98997638010842,2.47293046891162));
#30659=CARTESIAN_POINT('Ctrl Pts',(30.,4.01528229489678,2.42115592843892));
#30660=CARTESIAN_POINT('Ctrl Pts',(30.,4.0761489236766,2.29662607992116));
#30661=CARTESIAN_POINT('Ctrl Pts',(30.,4.13125736838721,2.16953959103647));
#30662=CARTESIAN_POINT('Ctrl Pts',(30.,4.18054374041445,2.04031320922016));
#30663=CARTESIAN_POINT('Ctrl Pts',(30.,4.22997372079626,1.91071029354067));
#30664=CARTESIAN_POINT('Ctrl Pts',(30.,4.27354775694774,1.77895417121864));
#30665=CARTESIAN_POINT('Ctrl Pts',(30.,4.3111501113001,1.6454556625514));
#30666=CARTESIAN_POINT('Ctrl Pts',(30.,4.34817396593327,1.51401098405268));
#30667=CARTESIAN_POINT('Ctrl Pts',(30.,4.37940842315398,1.38087635322608));
#30668=CARTESIAN_POINT('Ctrl Pts',(30.,4.4046931579437,1.24644647155864));
#30669=CARTESIAN_POINT('Ctrl Pts',(30.,4.42089890441132,1.16028632006437));
#30670=CARTESIAN_POINT('Ctrl Pts',(30.,4.43465955561036,1.07359417600813));
#30671=CARTESIAN_POINT('Ctrl Pts',(30.,4.44592197371389,0.986476687916269));
#30672=CARTESIAN_POINT('Ctrl Pts',(30.,4.44839086637678,0.967379214781952));
#30673=CARTESIAN_POINT('Ctrl Pts',(30.,4.45073967281179,0.948261313176081));
#30674=CARTESIAN_POINT('Ctrl Pts',(30.,4.45296777758924,0.929124127526741));
#30675=CARTESIAN_POINT('Ctrl Pts',(30.,4.45503255715034,0.911389741700035));
#30676=CARTESIAN_POINT('Ctrl Pts',(30.,4.45699251705267,0.893648784711569));
#30677=CARTESIAN_POINT('Ctrl Pts',(30.,4.45884747035307,0.875902588838401));
#30678=CARTESIAN_POINT('Ctrl Pts',(30.,4.47288215368143,0.741633850477624));
#30679=CARTESIAN_POINT('Ctrl Pts',(30.,4.4809109307611,0.607056772754871));
#30680=CARTESIAN_POINT('Ctrl Pts',(30.,4.48284622078689,0.472553103246923));
#30681=CARTESIAN_POINT('Ctrl Pts',(30.,4.4841564920511,0.381488564733919));
#30682=CARTESIAN_POINT('Ctrl Pts',(30.,4.48267253782096,0.290457568449046));
#30683=CARTESIAN_POINT('Ctrl Pts',(30.,4.47835364427375,0.199579870531098));
#30684=CARTESIAN_POINT('Ctrl Pts',(30.,4.47194672265211,0.0647661083135189));
#30685=CARTESIAN_POINT('Ctrl Pts',(30.,4.45930307443608,-0.0697114630799221));
#30686=CARTESIAN_POINT('Ctrl Pts',(30.,4.44051793519591,-0.203434213073621));
#30687=CARTESIAN_POINT('Ctrl Pts',(30.,4.42188441330993,-0.336077668988553));
#30688=CARTESIAN_POINT('Ctrl Pts',(30.,4.39720776531948,-0.467979164954463));
#30689=CARTESIAN_POINT('Ctrl Pts',(30.,4.36653661631927,-0.598704850027088));
#30690=CARTESIAN_POINT('Ctrl Pts',(30.,4.35826921191622,-0.633941942199734));
#30691=CARTESIAN_POINT('Ctrl Pts',(30.,4.34956603093133,-0.669093426449049));
#30692=CARTESIAN_POINT('Ctrl Pts',(30.,4.34042752155899,-0.704150383578858));
#30693=CARTESIAN_POINT('Ctrl Pts',(30.,4.33455297624871,-0.726686190536959));
#30694=CARTESIAN_POINT('Ctrl Pts',(30.,4.32849853352323,-0.749182931588532));
#30695=CARTESIAN_POINT('Ctrl Pts',(30.,4.32226426812988,-0.771638192356437));
#30696=CARTESIAN_POINT('Ctrl Pts',(30.,4.31754067405252,-0.788652151512211));
#30697=CARTESIAN_POINT('Ctrl Pts',(30.,4.31271393090463,-0.80564179080815));
#30698=CARTESIAN_POINT('Ctrl Pts',(30.,4.3077879772602,-0.822593202800587));
#30699=CARTESIAN_POINT('Ctrl Pts',(30.,4.27100671946256,-0.949166512160226));
#30700=CARTESIAN_POINT('Ctrl Pts',(30.,4.22864672526021,-1.07379766426646));
#30701=CARTESIAN_POINT('Ctrl Pts',(30.,4.1808305106355,-1.19610739677557));
#30702=CARTESIAN_POINT('Ctrl Pts',(30.,4.13354228297351,-1.31706658439766));
#30703=CARTESIAN_POINT('Ctrl Pts',(30.,4.08091725186588,-1.43575600239369));
#30704=CARTESIAN_POINT('Ctrl Pts',(30.,4.02303011908695,-1.55178410876982));
#30705=CARTESIAN_POINT('Ctrl Pts',(30.,3.96819820087205,-1.66168838859898));
#30706=CARTESIAN_POINT('Ctrl Pts',(30.,3.90864442065182,-1.76920516529743));
#30707=CARTESIAN_POINT('Ctrl Pts',(30.,3.84440013420362,-1.87397285765276));
#30708=CARTESIAN_POINT('Ctrl Pts',(30.,3.79893603048459,-1.94811438050221));
#30709=CARTESIAN_POINT('Ctrl Pts',(30.,3.75112211275763,-2.02087850788643));
#30710=CARTESIAN_POINT('Ctrl Pts',(30.,3.70103315780837,-2.09216345552501));
#30711=CARTESIAN_POINT('Ctrl Pts',(30.,3.67453247022062,-2.12987835951916));
#30712=CARTESIAN_POINT('Ctrl Pts',(30.,3.64739487281119,-2.16717906849915));
#30713=CARTESIAN_POINT('Ctrl Pts',(30.,3.61963092738038,-2.20404946355424));
#30714=CARTESIAN_POINT('Ctrl Pts',(30.,3.60474871618731,-2.22381297329565));
#30715=CARTESIAN_POINT('Ctrl Pts',(30.,3.58968653441096,-2.24345283054055));
#30716=CARTESIAN_POINT('Ctrl Pts',(30.,3.57444597381909,-2.26296646152855));
#30717=CARTESIAN_POINT('Ctrl Pts',(30.,3.56382219475439,-2.27656888140787));
#30718=CARTESIAN_POINT('Ctrl Pts',(30.,3.55311488934063,-2.29010588184238));
#30719=CARTESIAN_POINT('Ctrl Pts',(30.,3.54232950699003,-2.30357088580617));
#30720=CARTESIAN_POINT('Ctrl Pts',(30.,3.46063422988411,-2.40556330427549));
#30721=CARTESIAN_POINT('Ctrl Pts',(30.,3.37438073686154,-2.50353329208469));
#30722=CARTESIAN_POINT('Ctrl Pts',(30.,3.28388555158297,-2.59720218594732));
#30723=CARTESIAN_POINT('Ctrl Pts',(30.,3.19548605035865,-2.68870189913318));
#30724=CARTESIAN_POINT('Ctrl Pts',(30.,3.10303822337506,-2.77609776168811));
#30725=CARTESIAN_POINT('Ctrl Pts',(30.,3.00680578566741,-2.85908852120383));
#30726=CARTESIAN_POINT('Ctrl Pts',(30.,2.90715127912884,-2.94503046950951));
#30727=CARTESIAN_POINT('Ctrl Pts',(30.,2.80343761470821,-3.02624930319516));
#30728=CARTESIAN_POINT('Ctrl Pts',(30.,2.69593400653002,-3.10235578897998));
#30729=CARTESIAN_POINT('Ctrl Pts',(30.,2.59557657777575,-3.17340318314957));
#30730=CARTESIAN_POINT('Ctrl Pts',(30.,2.49191560602939,-3.23999516173219));
#30731=CARTESIAN_POINT('Ctrl Pts',(30.,2.38515991446318,-3.30176482420669));
#30732=CARTESIAN_POINT('Ctrl Pts',(30.,2.37755813215443,-3.3061632737931));
#30733=CARTESIAN_POINT('Ctrl Pts',(30.,2.36994065609269,-3.3105372499843));
#30734=CARTESIAN_POINT('Ctrl Pts',(30.,2.36230756092333,-3.31488661006745));
#30735=CARTESIAN_POINT('Ctrl Pts',(52.575,0.695807839646318,4.87560011181051));
#30736=CARTESIAN_POINT('Ctrl Pts',(52.5353636670017,1.50529535683805,4.76007633060593));
#30737=CARTESIAN_POINT('Ctrl Pts',(52.4957273340033,2.28505099782045,4.439118397491));
#30738=CARTESIAN_POINT('Ctrl Pts',(52.456091001005,2.94078002088763,3.95114651967049));
#30739=CARTESIAN_POINT('Ctrl Pts',(52.4164546680067,3.5965090439548,3.46317464184999));
#30740=CARTESIAN_POINT('Ctrl Pts',(52.3768183350084,4.12821144910675,2.80818881932393));
#30741=CARTESIAN_POINT('Ctrl Pts',(52.3371820020101,4.47114016046936,2.06608466315826));
#30742=CARTESIAN_POINT('Ctrl Pts',(52.2975456690118,4.81406887183195,1.3239805069926));
#30743=CARTESIAN_POINT('Ctrl Pts',(52.2579093360134,4.96822388940519,0.494758017187346));
#30744=CARTESIAN_POINT('Ctrl Pts',(52.2182730030151,4.91494370822671,-0.320960650504854));
#30745=CARTESIAN_POINT('Ctrl Pts',(52.1786366700168,4.86166352704823,-1.13667931819705));
#30746=CARTESIAN_POINT('Ctrl Pts',(52.1390003370185,4.60094814711803,-1.93889416377618));
#30747=CARTESIAN_POINT('Ctrl Pts',(52.0993640040202,4.16444074494492,-2.63007232252029));
#30748=CARTESIAN_POINT('Ctrl Pts',(52.0597276710218,3.72793334277182,-3.32125048126438));
#30749=CARTESIAN_POINT('Ctrl Pts',(52.0200913380235,3.11563391835576,-3.90139195317348));
#30750=CARTESIAN_POINT('Ctrl Pts',(51.9804550050252,2.40195439260487,-4.30004051622935));
#30751=CARTESIAN_POINT('Ctrl Pts',(51.9408186720269,1.68827486685394,-4.69868907928524));
#30752=CARTESIAN_POINT('Ctrl Pts',(51.9011823390286,0.873215239768212,-4.91584473348791));
#30753=CARTESIAN_POINT('Ctrl Pts',(51.8615460060302,0.0557974474159643,
-4.9251071071408));
#30754=CARTESIAN_POINT('Ctrl Pts',(51.8219096730319,-0.76162034493626,-4.93436948079368));
#30755=CARTESIAN_POINT('Ctrl Pts',(51.7822733400336,-1.58139630255493,-4.73573857389677));
#30756=CARTESIAN_POINT('Ctrl Pts',(51.7426370070352,-2.30392265539945,-4.3533561208101));
#30757=CARTESIAN_POINT('Ctrl Pts',(51.7030006740369,-3.02644900824399,-3.97097366772342));
#30758=CARTESIAN_POINT('Ctrl Pts',(51.6633643410386,-3.65172575631444,-3.40483966844693));
#30759=CARTESIAN_POINT('Ctrl Pts',(51.6237280080403,-4.1037833688659,-2.72373593691276));
#30760=CARTESIAN_POINT('Ctrl Pts',(51.584091675042,-4.55584098141733,-2.04263220537863));
#30761=CARTESIAN_POINT('Ctrl Pts',(51.5444553420437,-4.83467945844985,-1.24655874158681));
#30762=CARTESIAN_POINT('Ctrl Pts',(51.5048190090453,-4.90641860669811,-0.432241155930334));
#30763=CARTESIAN_POINT('Ctrl Pts',(51.4978265146648,-4.91907456029036,-0.288582277548382));
#30764=CARTESIAN_POINT('Ctrl Pts',(51.4908340202842,-4.92528502287894,-0.14435559277112));
#30765=CARTESIAN_POINT('Ctrl Pts',(51.4838415259036,-4.9251402971202,-0.000116503725961781));
#30766=CARTESIAN_POINT('Origin',(41.25,0.,0.));
#30767=CARTESIAN_POINT('Origin',(52.575,0.,0.));
#30768=CARTESIAN_POINT('Ctrl Pts',(-53.0683458050225,-1.79217368492195,
3.65473442716065));
#30769=CARTESIAN_POINT('Ctrl Pts',(-53.0287094720242,-2.39896296820851,
3.35718290666791));
#30770=CARTESIAN_POINT('Ctrl Pts',(-52.9494368060276,-3.46086376985422,
2.45430560800941));
#30771=CARTESIAN_POINT('Ctrl Pts',(-52.8305278070326,-4.21283755893848,
0.502366005806227));
#30772=CARTESIAN_POINT('Ctrl Pts',(-52.7116188080376,-3.94100158787114,
-1.57116901649836));
#30773=CARTESIAN_POINT('Ctrl Pts',(-52.5927098090427,-2.71153766019247,
-3.26314029666967));
#30774=CARTESIAN_POINT('Ctrl Pts',(-52.4738008100477,-0.823144024575674,
-4.16204656282918));
#30775=CARTESIAN_POINT('Ctrl Pts',(-52.3548918110528,1.26526436602798,-4.04962642367063));
#30776=CARTESIAN_POINT('Ctrl Pts',(-52.2359828120578,3.04621665534188,-2.95311079097194));
#30777=CARTESIAN_POINT('Ctrl Pts',(-52.1170738130628,4.08693027247079,-1.13899868529834));
#30778=CARTESIAN_POINT('Ctrl Pts',(-51.9981648140679,4.13451401645655,0.951899429035897));
#30779=CARTESIAN_POINT('Ctrl Pts',(-51.8792558150729,3.17740293277235,2.81148063819688));
#30780=CARTESIAN_POINT('Ctrl Pts',(-51.760346816078,1.44817770563431,3.98786896704909));
#30781=CARTESIAN_POINT('Ctrl Pts',(-51.641437817083,-0.632957411871854,
4.19519722352873));
#30782=CARTESIAN_POINT('Ctrl Pts',(-51.522528818088,-2.56028268385088,3.38308566467023));
#30783=CARTESIAN_POINT('Ctrl Pts',(-51.403619819093,-3.86545481878031,1.74887812750191));
#30784=CARTESIAN_POINT('Ctrl Pts',(-51.2847108200981,-4.23131463624997,
-0.310309743601171));
#30785=CARTESIAN_POINT('Ctrl Pts',(-51.1658018211031,-3.56895759144185,
-2.29409186145612));
#30786=CARTESIAN_POINT('Ctrl Pts',(-51.0468928221082,-2.03933759109846,
-3.72040560679174));
#30787=CARTESIAN_POINT('Ctrl Pts',(-50.9279838231133,-0.0141549843878351,
-4.24265428344519));
#30788=CARTESIAN_POINT('Ctrl Pts',(-50.8090748241182,2.01446730968869,-3.73393052561418));
#30789=CARTESIAN_POINT('Ctrl Pts',(-50.6901658251233,3.55357051600268,-2.31785510914493));
#30790=CARTESIAN_POINT('Ctrl Pts',(-50.5712568261283,4.22914985879238,-0.338536836715756));
#30791=CARTESIAN_POINT('Ctrl Pts',(-50.4523478271334,3.87703837313768,1.72304647947545));
#30792=CARTESIAN_POINT('Ctrl Pts',(-50.3334388281384,2.58279976746683,3.36592648157085));
#30793=CARTESIAN_POINT('Ctrl Pts',(-50.2145298291435,0.660936291289855,
4.19088044882765));
#30794=CARTESIAN_POINT('Ctrl Pts',(-50.0956208301485,-1.42153586209668,
3.99744312162439));
#30795=CARTESIAN_POINT('Ctrl Pts',(-49.9767118311536,-3.15857230942583,
2.83262010934112));
#30796=CARTESIAN_POINT('Ctrl Pts',(-49.8578028321586,-4.1280701494123,0.979465445678941));
#30797=CARTESIAN_POINT('Ctrl Pts',(-49.7388938331636,-4.09443970767262,
-1.11170103804332));
#30798=CARTESIAN_POINT('Ctrl Pts',(-49.6199848341687,-3.06585324049081,
-2.93272222099405));
#30799=CARTESIAN_POINT('Ctrl Pts',(-49.5010758351736,-1.29225906223574,
-4.04108676395591));
#30800=CARTESIAN_POINT('Ctrl Pts',(-49.3821668361788,0.795356333133346,
-4.167460140312));
#30801=CARTESIAN_POINT('Ctrl Pts',(-49.2632578371837,2.68969874550031,-3.28113339811124));
#30802=CARTESIAN_POINT('Ctrl Pts',(-49.1443488381888,3.93043964837605,-1.59748548920479));
#30803=CARTESIAN_POINT('Ctrl Pts',(-49.0254398391938,4.216076827669,0.474354193550262));
#30804=CARTESIAN_POINT('Ctrl Pts',(-48.9065308401989,3.47719994816421,2.43092497585451));
#30805=CARTESIAN_POINT('Ctrl Pts',(-48.7876218412039,1.89335738663818,3.79677672825371));
#30806=CARTESIAN_POINT('Ctrl Pts',(-48.6687128422089,-0.150574338398622,
4.24000508093589));
#30807=CARTESIAN_POINT('Ctrl Pts',(-48.549803843214,-2.15791623528735,3.65290476733649));
#30808=CARTESIAN_POINT('Ctrl Pts',(-48.430894844219,-3.64088070474142,2.17814219269265));
#30809=CARTESIAN_POINT('Ctrl Pts',(-48.3119858452241,-4.23910478143669,
0.174087247513894));
#30810=CARTESIAN_POINT('Ctrl Pts',(-48.1930768462291,-3.80721896620666,
-1.87227120393991));
#30811=CARTESIAN_POINT('Ctrl Pts',(-48.0741678472342,-2.45017226913454,
-3.46366447123714));
#30812=CARTESIAN_POINT('Ctrl Pts',(-47.9552588482392,-0.497729416154917,
-4.21338120113056));
#30813=CARTESIAN_POINT('Ctrl Pts',(-47.8363498492442,1.57566255733915,-3.93923891419978));
#30814=CARTESIAN_POINT('Ctrl Pts',(-47.7174408502492,3.26616576767762,-2.70785466666829));
#30815=CARTESIAN_POINT('Ctrl Pts',(-47.5985318512543,4.16298497174054,-0.818456988979114));
#30816=CARTESIAN_POINT('Ctrl Pts',(-47.4796228522594,4.04819153105236,1.26982717157192));
#30817=CARTESIAN_POINT('Ctrl Pts',(-47.3607138532644,2.94968045290301,3.04954110375778));
#30818=CARTESIAN_POINT('Ctrl Pts',(-47.2418048542694,1.13439185468392,4.08821120268671));
#30819=CARTESIAN_POINT('Ctrl Pts',(-47.1228958552744,-0.956555952514039,
4.13343881380338));
#30820=CARTESIAN_POINT('Ctrl Pts',(-47.0039868562795,-2.81505898666,3.17423354833433));
#30821=CARTESIAN_POINT('Ctrl Pts',(-46.8850778572845,-3.9894977529893,1.44368396702315));
#30822=CARTESIAN_POINT('Ctrl Pts',(-46.7661688582896,-4.19448157280151,
-0.637683348673077));
#30823=CARTESIAN_POINT('Ctrl Pts',(-46.6472598592946,-3.38019901859953,
-2.5640924929505));
#30824=CARTESIAN_POINT('Ctrl Pts',(-46.5283508602997,-1.74452217827771,
-3.8674226672609));
#30825=CARTESIAN_POINT('Ctrl Pts',(-46.4094418613047,0.315076609054344,
-4.23096235485186));
#30826=CARTESIAN_POINT('Ctrl Pts',(-46.2905328623097,2.29811122813968,-3.56637077444897));
#30827=CARTESIAN_POINT('Ctrl Pts',(-46.1716238633148,3.72270079080243,-2.03514484494512));
#30828=CARTESIAN_POINT('Ctrl Pts',(-46.0527148643198,4.2426675363842,-0.00937515104479359));
#30829=CARTESIAN_POINT('Ctrl Pts',(-45.9338058653248,3.7316586343443,2.01867272098968));
#30830=CARTESIAN_POINT('Ctrl Pts',(-45.8148968663299,2.31385014354139,3.5561795836249));
#30831=CARTESIAN_POINT('Ctrl Pts',(-45.6959878673349,0.333772012288686,
4.22952857438387));
#30832=CARTESIAN_POINT('Ctrl Pts',(-45.57707886834,-1.7274133029682,3.87509470833104));
#30833=CARTESIAN_POINT('Ctrl Pts',(-45.458169869345,-3.36883415789558,2.57900603610148));
#30834=CARTESIAN_POINT('Ctrl Pts',(-45.33926087035,-4.19162240778749,0.656214376839717));
#30835=CARTESIAN_POINT('Ctrl Pts',(-45.2203518713551,-3.99583906574759,
-1.42603852628503));
#30836=CARTESIAN_POINT('Ctrl Pts',(-45.1014428723601,-2.82905982713036,
-3.16176156781322));
#30837=CARTESIAN_POINT('Ctrl Pts',(-44.9825338733652,-0.974814091813329,
-4.12917100710215));
#30838=CARTESIAN_POINT('Ctrl Pts',(-44.8636248743702,1.11631317618967,-4.09318465336435));
#30839=CARTESIAN_POINT('Ctrl Pts',(-44.7447158753752,2.93617438620888,-3.06254725647695));
#30840=CARTESIAN_POINT('Ctrl Pts',(-44.6258068763803,4.04254007317222,-1.28770550464645));
#30841=CARTESIAN_POINT('Ctrl Pts',(-44.5068978773853,4.16656143857104,0.800050934283993));
#30842=CARTESIAN_POINT('Ctrl Pts',(-44.3879888783903,3.27810106806685,2.69339360894175));
#30843=CARTESIAN_POINT('Ctrl Pts',(-44.2690798793954,1.59305639924211,3.93223688581989));
#30844=CARTESIAN_POINT('Ctrl Pts',(-44.1501708804004,-0.479103780509667,
4.21553976710139));
#30845=CARTESIAN_POINT('Ctrl Pts',(-44.0312618814054,-2.4348408745219,3.47445897688703));
#30846=CARTESIAN_POINT('Ctrl Pts',(-43.9123528824105,-3.79890742291198,
1.88907880356681));
#30847=CARTESIAN_POINT('Ctrl Pts',(-43.7934438834155,-4.23983270028836,
-0.155351305015692));
#30848=CARTESIAN_POINT('Ctrl Pts',(-43.6745348844206,-3.65047141713449,
-2.16202982679776));
#30849=CARTESIAN_POINT('Ctrl Pts',(-43.5556258854256,-2.17403874853064,
-3.64333320102936));
#30850=CARTESIAN_POINT('Ctrl Pts',(-43.4367168864307,-0.169311716792706,
-4.23929645182126));
#30851=CARTESIAN_POINT('Ctrl Pts',(-43.3178078874356,1.87656008092686,-3.80511075431245));
#30852=CARTESIAN_POINT('Ctrl Pts',(-43.1988988884407,3.46642105478168,-2.44626147372541));
#30853=CARTESIAN_POINT('Ctrl Pts',(-43.0799898894457,4.21394248881074,-0.492996289805673));
#30854=CARTESIAN_POINT('Ctrl Pts',(-42.9610808904508,3.9374548435202,1.58012754509629));
#30855=CARTESIAN_POINT('Ctrl Pts',(-42.8421718914559,2.70418603569597,3.26915855205306));
#30856=CARTESIAN_POINT('Ctrl Pts',(-42.7232628924609,0.813740892457039,
4.16401580837881));
#30857=CARTESIAN_POINT('Ctrl Pts',(-42.6043538934659,-1.2743362201606,4.04653615170507));
#30858=CARTESIAN_POINT('Ctrl Pts',(-42.485444894471,-3.05296381848078,2.94668618241789));
#30859=CARTESIAN_POINT('Ctrl Pts',(-42.366535895476,-4.08928414300699,1.12890118224142));
#30860=CARTESIAN_POINT('Ctrl Pts',(-42.247626896481,-4.13276248524086,-0.959449239315854));
#30861=CARTESIAN_POINT('Ctrl Pts',(-42.1287178974861,-3.17025358567157,
-2.82214018180611));
#30862=CARTESIAN_POINT('Ctrl Pts',(-42.0098088984911,-1.44080606975949,
-3.98424622002752));
#30863=CARTESIAN_POINT('Ctrl Pts',(-41.8512635664978,1.34123824569469,-4.27940453375867));
#30864=CARTESIAN_POINT('Ctrl Pts',(-41.6530819015062,4.38508519896316,-1.98115288915087));
#30865=CARTESIAN_POINT('Ctrl Pts',(-41.4152639035164,4.03738586191726,2.61791030678041));
#30866=CARTESIAN_POINT('Ctrl Pts',(-41.2170822385246,0.682605700869055,
4.43241160683543));
#30867=CARTESIAN_POINT('Ctrl Pts',(-41.0585369065315,-2.02344112387514,
3.7223414795892));
#30868=CARTESIAN_POINT('Ctrl Pts',(-40.9396279075364,-3.55851407251,2.3134304828493));
#30869=CARTESIAN_POINT('Ctrl Pts',(-40.8207189085415,-4.23003625048233,
0.327203181285681));
#30870=CARTESIAN_POINT('Ctrl Pts',(-40.7018099095465,-3.87307886616663,
-1.73087341477296));
#30871=CARTESIAN_POINT('Ctrl Pts',(-40.5829009105516,-2.57524274258496,
-3.37219103126866));
#30872=CARTESIAN_POINT('Ctrl Pts',(-40.4639919115566,-0.651474730133847,
-4.1921317137068));
#30873=CARTESIAN_POINT('Ctrl Pts',(-40.3450829125617,1.43053090860402,-3.99434390257198));
#30874=CARTESIAN_POINT('Ctrl Pts',(-40.2261739135667,3.1649510603171,-2.82543882253934));
#30875=CARTESIAN_POINT('Ctrl Pts',(-40.1072649145718,4.13026449432683,-0.970190141382548));
#30876=CARTESIAN_POINT('Ctrl Pts',(-39.9883559155767,4.09192547196896,1.12093825548876));
#30877=CARTESIAN_POINT('Ctrl Pts',(-39.8694469165819,3.0592368484789,2.93961562653621));
#30878=CARTESIAN_POINT('Ctrl Pts',(-39.7505379175868,1.28315058440506,4.04399186048308));
#30879=CARTESIAN_POINT('Ctrl Pts',(-39.6316289185919,-0.804744661503545,
4.16565563790974));
#30880=CARTESIAN_POINT('Ctrl Pts',(-39.5127199195969,-2.69708497226697,
3.27506548731581));
#30881=CARTESIAN_POINT('Ctrl Pts',(-39.393810920602,-3.93402919418496,1.58862482625052));
#30882=CARTESIAN_POINT('Ctrl Pts',(-39.274901921607,-4.21499728287336,-0.48385251861988));
#30883=CARTESIAN_POINT('Ctrl Pts',(-39.155992922612,-3.47171371609164,-2.43875382264022));
#30884=CARTESIAN_POINT('Ctrl Pts',(-39.0370839236171,-1.88479759517879,
-3.80103318737441));
#30885=CARTESIAN_POINT('Ctrl Pts',(-38.9181749246221,0.160127626810078,
-4.23965506894654));
#30886=CARTESIAN_POINT('Ctrl Pts',(-38.7992659256272,2.16614156389975,-3.64803321565397));
#30887=CARTESIAN_POINT('Ctrl Pts',(-38.6803569266322,3.6457792997346,-2.16993295812935));
#30888=CARTESIAN_POINT('Ctrl Pts',(-38.5614479276372,4.23948627792256,-0.164535157769628));
#30889=CARTESIAN_POINT('Ctrl Pts',(-38.4425389286423,3.80299065872691,1.88084495893092));
#30890=CARTESIAN_POINT('Ctrl Pts',(-38.3236299296473,2.44236164439116,3.46917646169672));
#30891=CARTESIAN_POINT('Ctrl Pts',(-38.2047209306524,0.488234469363121,
4.21449199984978));
#30892=CARTESIAN_POINT('Ctrl Pts',(-38.0858119316573,-1.58453453732273,
3.93567859708109));
#30893=CARTESIAN_POINT('Ctrl Pts',(-37.9669029326625,-3.27225887423897,
2.70048839604023));
#30894=CARTESIAN_POINT('Ctrl Pts',(-37.8479939336674,-4.16481856926941,
0.809074782002492));
#30895=CARTESIAN_POINT('Ctrl Pts',(-37.7290849346726,-4.04532005215358,
-1.2789454224014));
#30896=CARTESIAN_POINT('Ctrl Pts',(-37.6101759356775,-2.94280167197283,
-3.05617964738425));
#30897=CARTESIAN_POINT('Ctrl Pts',(-37.4912669366826,-1.12517732754963,
-4.09075686143469));
#30898=CARTESIAN_POINT('Ctrl Pts',(-37.3723579376876,0.965867079610468,
-4.13127298810448));
#30899=CARTESIAN_POINT('Ctrl Pts',(-37.2534489386927,2.82220409351303,-3.1678825376449));
#30900=CARTESIAN_POINT('Ctrl Pts',(-37.1345399396977,3.99274056611069,-1.43469107806466));
#30901=CARTESIAN_POINT('Ctrl Pts',(-37.0156309407027,4.19303408291871,0.647132828117663));
#30902=CARTESIAN_POINT('Ctrl Pts',(-36.8967219417077,3.37441296829128,2.57170232281563));
#30903=CARTESIAN_POINT('Ctrl Pts',(-36.7778129427128,1.73580358791025,3.87134364555039));
#30904=CARTESIAN_POINT('Ctrl Pts',(-36.6589039437178,-0.324609106740258,
4.23024167696931));
#30905=CARTESIAN_POINT('Ctrl Pts',(-36.5399949447229,-2.3061412194985,3.56118356638298));
#30906=CARTESIAN_POINT('Ctrl Pts',(-36.4210859457279,-3.72727697385935,
2.02675160734717));
#30907=CARTESIAN_POINT('Ctrl Pts',(-36.302176946733,-4.24267789063578,-0.00018454463676528));
#30908=CARTESIAN_POINT('Ctrl Pts',(-36.183267947738,-3.72710064368882,-2.02707585195046));
#30909=CARTESIAN_POINT('Ctrl Pts',(-36.064358948743,-2.30583140769797,-3.56138417430919));
#30910=CARTESIAN_POINT('Ctrl Pts',(-35.9454499497481,-0.324241098120267,
-4.23026990014066));
#30911=CARTESIAN_POINT('Ctrl Pts',(-35.8265409507531,1.73614036661006,-3.87119262568701));
#30912=CARTESIAN_POINT('Ctrl Pts',(-35.7076319517581,3.37463667925653,-2.5714087580085));
#30913=CARTESIAN_POINT('Ctrl Pts',(-35.5887229527632,4.19309036399278,-0.646768055130456));
#30914=CARTESIAN_POINT('Ctrl Pts',(-35.4698139537682,3.99261574089381,1.43503841875865));
#30915=CARTESIAN_POINT('Ctrl Pts',(-35.3509049547733,2.82192849475196,3.16812804164435));
#30916=CARTESIAN_POINT('Ctrl Pts',(-35.2319959557783,0.96550767828667,4.13135699751496));
#30917=CARTESIAN_POINT('Ctrl Pts',(-35.1130869567833,-1.12553319628343,
4.09065896180682));
#30918=CARTESIAN_POINT('Ctrl Pts',(-34.9941779577884,-2.94306753139286,
3.05592362852992));
#30919=CARTESIAN_POINT('Ctrl Pts',(-34.8752689587934,-4.04543129795022,
1.27859349728957));
#30920=CARTESIAN_POINT('Ctrl Pts',(-34.7563599597985,-4.16474816852819,
-0.809437094830369));
#30921=CARTESIAN_POINT('Ctrl Pts',(-34.6374509608035,-3.27202393444525,
-2.70077305417611));
#30922=CARTESIAN_POINT('Ctrl Pts',(-34.5185419618086,-1.5841921492944,-3.93581642761199));
#30923=CARTESIAN_POINT('Ctrl Pts',(-34.3996329628135,0.488601104807327,
-4.21444951068671));
#30924=CARTESIAN_POINT('Ctrl Pts',(-34.2807239638187,2.44266343405159,-3.46896397584259));
#30925=CARTESIAN_POINT('Ctrl Pts',(-34.1618149648236,3.80315426747452,-1.88051411468693));
#30926=CARTESIAN_POINT('Ctrl Pts',(-34.0429059658287,4.2394719479716,0.164903972384525));
#30927=CARTESIAN_POINT('Ctrl Pts',(-33.9239969668337,3.64559051443191,2.17025010513313));
#30928=CARTESIAN_POINT('Ctrl Pts',(-33.8050879678388,2.1658241961235,3.64822165845675));
#30929=CARTESIAN_POINT('Ctrl Pts',(-33.6861789688438,0.159758802036821,
4.23966895440156));
#30930=CARTESIAN_POINT('Ctrl Pts',(-33.5672699698489,-1.88512826096029,
3.80086926340264));
#30931=CARTESIAN_POINT('Ctrl Pts',(-33.4483609708539,-3.47192585240921,
2.43845167947057));
#30932=CARTESIAN_POINT('Ctrl Pts',(-33.3294519718589,-4.21503937635071,
0.483486063466008));
#30933=CARTESIAN_POINT('Ctrl Pts',(-33.210542972864,-3.93389094398069,-1.58896751339184));
#30934=CARTESIAN_POINT('Ctrl Pts',(-33.091633973869,-2.69680011715167,-3.27529919943904));
#30935=CARTESIAN_POINT('Ctrl Pts',(-32.9727249748741,-0.804382135063499,
-4.16572743931235));
#30936=CARTESIAN_POINT('Ctrl Pts',(-32.853815975879,1.28350211569609,-4.04387660995158));
#30937=CARTESIAN_POINT('Ctrl Pts',(-32.7349069768842,3.05949310273849,-2.93935667663218));
#30938=CARTESIAN_POINT('Ctrl Pts',(-32.6159979778891,4.09202190325118,-1.12056791874808));
#30939=CARTESIAN_POINT('Ctrl Pts',(-32.4970889788942,4.13018220918936,0.970520807006677));
#30940=CARTESIAN_POINT('Ctrl Pts',(-32.3781799798992,3.16470099886364,2.82577127648086));
#30941=CARTESIAN_POINT('Ctrl Pts',(-32.2592709809043,1.43019189953828,3.99435437116099));
#30942=CARTESIAN_POINT('Ctrl Pts',(-32.1403619819093,-0.651856339348117,
4.19230235613684));
#30943=CARTESIAN_POINT('Ctrl Pts',(-32.0214529829143,-2.57550234280079,
3.37151351350433));
#30944=CARTESIAN_POINT('Ctrl Pts',(-31.9025439839194,-3.87329676764037,
1.73144099180317));
#30945=CARTESIAN_POINT('Ctrl Pts',(-31.7836349849244,-4.22987327936596,
-0.329374753772751));
#30946=CARTESIAN_POINT('Ctrl Pts',(-31.6647259859294,-3.55858318971203,
-2.31015180080996));
#30947=CARTESIAN_POINT('Ctrl Pts',(-31.5458169869345,-2.02255110907419,
-3.72955802299772));
#30948=CARTESIAN_POINT('Ctrl Pts',(-31.4269079879395,0.00496435902457082,
-4.24267488557468));
#30949=CARTESIAN_POINT('Ctrl Pts',(-31.3079989889446,2.03127363286532,-3.72481475967269));
#30950=CARTESIAN_POINT('Ctrl Pts',(-31.1890899899496,3.56397954706214,-2.30181723085673));
#30951=CARTESIAN_POINT('Ctrl Pts',(-31.0701809909547,4.23063279613937,-0.319475851207252));
#30952=CARTESIAN_POINT('Ctrl Pts',(-30.9512719919596,3.86923364069296,1.74050225247754));
#30953=CARTESIAN_POINT('Ctrl Pts',(-30.8323629929648,2.56760636218215,3.37752821215737));
#30954=CARTESIAN_POINT('Ctrl Pts',(-30.7134539939697,0.642041383293453,
4.19382295160038));
#30955=CARTESIAN_POINT('Ctrl Pts',(-30.5945449949749,-1.43953109436157,
3.99098332553759));
#30956=CARTESIAN_POINT('Ctrl Pts',(-30.4756359959798,-3.17131430799793,
2.8183836925229));
#30957=CARTESIAN_POINT('Ctrl Pts',(-30.3567269969849,-4.13242405408636,
0.960800203588555));
#30958=CARTESIAN_POINT('Ctrl Pts',(-30.2378179979899,-4.08942441038536,
-1.1300353505695));
#30959=CARTESIAN_POINT('Ctrl Pts',(-30.118908998995,-3.05253333388674,-2.94673281729211));
#30960=CARTESIAN_POINT('Ctrl Pts',(-30.0396363329983,-1.86695937376294,
-3.67969605923881));
#30961=CARTESIAN_POINT('Ctrl Pts',(-30.,-1.22233170237264,-3.88263769354994));
#30962=CARTESIAN_POINT('Ctrl Pts',(-52.9038972033484,-1.91758108071817,
3.91047455474603));
#30963=CARTESIAN_POINT('Ctrl Pts',(-52.86426087035,-2.56683045838858,3.59210185960144));
#30964=CARTESIAN_POINT('Ctrl Pts',(-52.7849882043534,-3.70303779363018,
2.62604570071254));
#30965=CARTESIAN_POINT('Ctrl Pts',(-52.6660792053585,-4.50763096630964,
0.537519078889939));
#30966=CARTESIAN_POINT('Ctrl Pts',(-52.5471702063634,-4.21677326676694,
-1.68111160541844));
#30967=CARTESIAN_POINT('Ctrl Pts',(-52.4282612073685,-2.90127757180321,
-3.49147861575446));
#30968=CARTESIAN_POINT('Ctrl Pts',(-52.3093522083735,-0.880743547074977,
-4.45328586905181));
#30969=CARTESIAN_POINT('Ctrl Pts',(-52.1904432093786,1.35380126982937,-4.33299912800889));
#30970=CARTESIAN_POINT('Ctrl Pts',(-52.0715342103836,3.25937573751765,-3.15975478809644));
#30971=CARTESIAN_POINT('Ctrl Pts',(-51.9526252113886,4.37291331450708,-1.21870014511799));
#30972=CARTESIAN_POINT('Ctrl Pts',(-51.8337162123937,4.42382673209854,1.01850861399359));
#30973=CARTESIAN_POINT('Ctrl Pts',(-51.7148072133987,3.39974177779992,3.00821406204645));
#30974=CARTESIAN_POINT('Ctrl Pts',(-51.5958982144038,1.5495139746811,4.26692019190625));
#30975=CARTESIAN_POINT('Ctrl Pts',(-51.4769892154088,-0.677248621669522,
4.48875624801429));
#30976=CARTESIAN_POINT('Ctrl Pts',(-51.3580802164138,-2.73943852493104,
3.61981716370482));
#30977=CARTESIAN_POINT('Ctrl Pts',(-51.2391712174189,-4.13594011073033,
1.87125591564839));
#30978=CARTESIAN_POINT('Ctrl Pts',(-51.1202622184239,-4.52740097754102,
-0.332023675215382));
#30979=CARTESIAN_POINT('Ctrl Pts',(-51.001353219429,-3.81869548292833,-2.45462099347217));
#30980=CARTESIAN_POINT('Ctrl Pts',(-50.882444220434,-2.1820402870485,-3.98074107671791));
#30981=CARTESIAN_POINT('Ctrl Pts',(-50.7635352214391,-0.0151454797536541,
-4.53953411681569));
#30982=CARTESIAN_POINT('Ctrl Pts',(-50.6446262224441,2.1554297071115,-3.9952124020534));
#30983=CARTESIAN_POINT('Ctrl Pts',(-50.5257172234491,3.80223169652302,-2.48004707497751));
#30984=CARTESIAN_POINT('Ctrl Pts',(-50.4068082244542,4.52508471972987,-0.36222595983527));
#30985=CARTESIAN_POINT('Ctrl Pts',(-50.2878992254591,4.14833422457659,1.84361669744306));
#30986=CARTESIAN_POINT('Ctrl Pts',(-50.1689902264643,2.76353124200318,3.60145726636404));
#30987=CARTESIAN_POINT('Ctrl Pts',(-50.0500812274693,0.707185323833562,
4.48413740690186));
#30988=CARTESIAN_POINT('Ctrl Pts',(-49.9311722284743,-1.52100786751463,
4.27716429817339));
#30989=CARTESIAN_POINT('Ctrl Pts',(-49.8122632294794,-3.37959348114136,
3.03083276818174));
#30990=CARTESIAN_POINT('Ctrl Pts',(-49.6933542304844,-4.41693195530615,
1.04800356330028));
#30991=CARTESIAN_POINT('Ctrl Pts',(-49.5744452314894,-4.38094822261397,
-1.18949234435358));
#30992=CARTESIAN_POINT('Ctrl Pts',(-49.4555362324945,-3.28038639317473,
-3.13793952745429));
#30993=CARTESIAN_POINT('Ctrl Pts',(-49.3366272334995,-1.38268492053985,
-4.32386190540457));
#30994=CARTESIAN_POINT('Ctrl Pts',(-49.2177182345045,0.851011411269701,
-4.45907826174644));
#30995=CARTESIAN_POINT('Ctrl Pts',(-49.0988092355096,2.87791047854129,-3.51073078489306));
#30996=CARTESIAN_POINT('Ctrl Pts',(-48.9799002365147,4.20547225530699,-1.70926957392212));
#30997=CARTESIAN_POINT('Ctrl Pts',(-48.8609912375196,4.51109690294586,0.507547139411817));
#30998=CARTESIAN_POINT('Ctrl Pts',(-48.7420822385247,3.72051709640205,2.60102900827211));
#30999=CARTESIAN_POINT('Ctrl Pts',(-48.6231732395297,2.02584511434425,4.06245626920221));
#31000=CARTESIAN_POINT('Ctrl Pts',(-48.5042642405348,-0.161110781273072,
4.53669953629844));
#31001=CARTESIAN_POINT('Ctrl Pts',(-48.3853552415398,-2.3089164746562,3.9085168644326));
#31002=CARTESIAN_POINT('Ctrl Pts',(-48.2664462425448,-3.89565141777433,
2.33055774390717));
#31003=CARTESIAN_POINT('Ctrl Pts',(-48.1475372435499,-4.53573623832059,
0.186269006757307));
#31004=CARTESIAN_POINT('Ctrl Pts',(-48.0286282445549,-4.07362920300179,
-2.00328342551518));
#31005=CARTESIAN_POINT('Ctrl Pts',(-47.9097192455599,-2.62162313135259,
-3.70603447415832));
#31006=CARTESIAN_POINT('Ctrl Pts',(-47.7908102465651,-0.532558043768616,
-4.50821264987691));
#31007=CARTESIAN_POINT('Ctrl Pts',(-47.67190124757,1.68591958188536,-4.21488724996391));
#31008=CARTESIAN_POINT('Ctrl Pts',(-47.5529922485751,3.49471579416743,-2.89733686072048));
#31009=CARTESIAN_POINT('Ctrl Pts',(-47.4340832495801,4.45428994314883,-0.875728536052195));
#31010=CARTESIAN_POINT('Ctrl Pts',(-47.3151742505852,4.33146382874587,1.35868335779866));
#31011=CARTESIAN_POINT('Ctrl Pts',(-47.1962652515901,3.15608441204037,3.26293281428972));
#31012=CARTESIAN_POINT('Ctrl Pts',(-47.0773562525953,1.21377095142287,4.37428387784502));
#31013=CARTESIAN_POINT('Ctrl Pts',(-46.9584472536002,-1.02349097781175,
4.4226762921144));
#31014=CARTESIAN_POINT('Ctrl Pts',(-46.8395382546053,-3.01204280552752,
3.39635061561123));
#31015=CARTESIAN_POINT('Ctrl Pts',(-46.7206292556103,-4.26866295218099,
1.54470578660482));
#31016=CARTESIAN_POINT('Ctrl Pts',(-46.6017202566154,-4.48799051961058,
-0.682305256009673));
#31017=CARTESIAN_POINT('Ctrl Pts',(-46.4828112576204,-3.61672852450737,
-2.7435149255121));
#31018=CARTESIAN_POINT('Ctrl Pts',(-46.3639022586255,-1.86659515877466,
-4.13804565945467));
#31019=CARTESIAN_POINT('Ctrl Pts',(-46.2449932596305,0.33712410219086,-4.52702404524379));
#31020=CARTESIAN_POINT('Ctrl Pts',(-46.1260842606355,2.45892161543405,-3.81592765335548));
#31021=CARTESIAN_POINT('Ctrl Pts',(-46.0071752616406,3.98319686628377,-2.17755415338436));
#31022=CARTESIAN_POINT('Ctrl Pts',(-45.8882662626456,4.53954829712943,-0.0100311774599003));
#31023=CARTESIAN_POINT('Ctrl Pts',(-45.7693572636507,3.99278153513842,2.15992939216729));
#31024=CARTESIAN_POINT('Ctrl Pts',(-45.6504482646557,2.47576186181158,3.80502333371354));
#31025=CARTESIAN_POINT('Ctrl Pts',(-45.5315392656607,0.357127716706735,
4.52548993595379));
#31026=CARTESIAN_POINT('Ctrl Pts',(-45.4126302666659,-1.84828908951253,
4.14625455177934));
#31027=CARTESIAN_POINT('Ctrl Pts',(-45.2937212676707,-3.60456840740805,
2.75947204419623));
#31028=CARTESIAN_POINT('Ctrl Pts',(-45.1748122686759,-4.48493128445738,
0.702132993308606));
#31029=CARTESIAN_POINT('Ctrl Pts',(-45.0559032696808,-4.27544799844884,
-1.52582560573556));
#31030=CARTESIAN_POINT('Ctrl Pts',(-44.936994270686,-3.02702335513946,-3.38300590795949));
#31031=CARTESIAN_POINT('Ctrl Pts',(-44.8180852716909,-1.04302673083841,
-4.41810984553875));
#31032=CARTESIAN_POINT('Ctrl Pts',(-44.699176272696,1.1944272169753,-4.37960534585094));
#31033=CARTESIAN_POINT('Ctrl Pts',(-44.580267273701,3.14163325801131,-3.27684907285165));
#31034=CARTESIAN_POINT('Ctrl Pts',(-44.4613582747062,4.32541690996749,-1.37781272765106));
#31035=CARTESIAN_POINT('Ctrl Pts',(-44.342449275711,4.45811667333,0.856034517246394));
#31036=CARTESIAN_POINT('Ctrl Pts',(-44.2235402767162,3.50748626748243,2.88186389013902));
#31037=CARTESIAN_POINT('Ctrl Pts',(-44.1046312777212,1.70453055828503,4.20739525448328));
#31038=CARTESIAN_POINT('Ctrl Pts',(-43.9857222787262,-0.51262907883053,
4.51052226155237));
#31039=CARTESIAN_POINT('Ctrl Pts',(-43.8668132797313,-2.60521892204093,
3.71758432559523));
#31040=CARTESIAN_POINT('Ctrl Pts',(-43.7479042807363,-4.06473605926936,
2.02126713732172));
#31041=CARTESIAN_POINT('Ctrl Pts',(-43.6289952817413,-4.53651509331103,
-0.166222016241634));
#31042=CARTESIAN_POINT('Ctrl Pts',(-43.5100862827464,-3.90591324049294,
-2.3133179148294));
#31043=CARTESIAN_POINT('Ctrl Pts',(-43.3911772837514,-2.32616716114331,
-3.89827552754776));
#31044=CARTESIAN_POINT('Ctrl Pts',(-43.2722682847565,-0.181159308161473,
-4.53594132084483));
#31045=CARTESIAN_POINT('Ctrl Pts',(-43.1533592857615,2.00787241677026,-4.07137346893065));
#31046=CARTESIAN_POINT('Ctrl Pts',(-43.0344502867666,3.70898394970129,-2.61743867794264));
#31047=CARTESIAN_POINT('Ctrl Pts',(-42.9155412877716,4.50881321367573,-0.527493716791647));
#31048=CARTESIAN_POINT('Ctrl Pts',(-42.7966322887766,4.21297833889654,1.69069700726593));
#31049=CARTESIAN_POINT('Ctrl Pts',(-42.6777232897817,2.8934115172095,3.49791799870001));
#31050=CARTESIAN_POINT('Ctrl Pts',(-42.5588142907867,0.870682430564956,
4.45539291260512));
#31051=CARTESIAN_POINT('Ctrl Pts',(-42.4399052917917,-1.36350792716849,
4.32969261418979));
#31052=CARTESIAN_POINT('Ctrl Pts',(-42.3209962927968,-3.26659503355605,
3.15288061740756));
#31053=CARTESIAN_POINT('Ctrl Pts',(-42.2020872938018,-4.37543189718947,
1.20789606904693));
#31054=CARTESIAN_POINT('Ctrl Pts',(-42.0831782948068,-4.4219526374448,-1.02658672242564));
#31055=CARTESIAN_POINT('Ctrl Pts',(-41.9642692958119,-3.39209215496744,
-3.01961950747069));
#31056=CARTESIAN_POINT('Ctrl Pts',(-41.8453602968169,-1.54162650841238,
-4.26304394307656));
#31057=CARTESIAN_POINT('Ctrl Pts',(-41.6868149648237,1.43509142351444,-4.57885596676009));
#31058=CARTESIAN_POINT('Ctrl Pts',(-41.488633299832,4.69193163900032,-2.11978410921226));
#31059=CARTESIAN_POINT('Ctrl Pts',(-41.2508153018422,4.31990203265866,2.8010986421318));
#31060=CARTESIAN_POINT('Ctrl Pts',(-41.0526336368504,0.730371050858233,
4.7425697133777));
#31061=CARTESIAN_POINT('Ctrl Pts',(-40.8940883048573,-2.16503146415692,
3.98281241225996));
#31062=CARTESIAN_POINT('Ctrl Pts',(-40.7751793058622,-3.80752117851334,
2.47531283535268));
#31063=CARTESIAN_POINT('Ctrl Pts',(-40.6562703068674,-4.52603313669918,
0.35009923159964));
#31064=CARTESIAN_POINT('Ctrl Pts',(-40.5373613078723,-4.14409765101203,
-1.85199132272229));
#31065=CARTESIAN_POINT('Ctrl Pts',(-40.4184523088774,-2.75544541412728,
-3.60816017807445));
#31066=CARTESIAN_POINT('Ctrl Pts',(-40.2995433098824,-0.697061689712906,
-4.48547622907039));
#31067=CARTESIAN_POINT('Ctrl Pts',(-40.1806343108875,1.5306323426131,-4.27384821119483));
#31068=CARTESIAN_POINT('Ctrl Pts',(-40.0617253118924,3.38641858527642,-3.02314897066693));
#31069=CARTESIAN_POINT('Ctrl Pts',(-39.9428163128976,4.41927984955773,-1.03807921936737));
#31070=CARTESIAN_POINT('Ctrl Pts',(-39.8239073139026,4.37825805320775,1.19937593630724));
#31071=CARTESIAN_POINT('Ctrl Pts',(-39.7049983149076,3.27330701897601,3.14531529921155));
#31072=CARTESIAN_POINT('Ctrl Pts',(-39.5860893159126,1.37293907675853,4.32697028612962));
#31073=CARTESIAN_POINT('Ctrl Pts',(-39.4671803169177,-0.861056688138638,
4.4571474892461));
#31074=CARTESIAN_POINT('Ctrl Pts',(-39.3482713179227,-2.88581355669983,
3.50423827189687));
#31075=CARTESIAN_POINT('Ctrl Pts',(-39.2293623189278,-4.20931297966839,
1.69978888586903));
#31076=CARTESIAN_POINT('Ctrl Pts',(-39.1104533199328,-4.50994181697772,
-0.517710110001807));
#31077=CARTESIAN_POINT('Ctrl Pts',(-38.9915443209379,-3.71464696511105,
-2.60940567879596));
#31078=CARTESIAN_POINT('Ctrl Pts',(-38.8726353219429,-2.01668635127596,
-4.0670105741501));
#31079=CARTESIAN_POINT('Ctrl Pts',(-38.7537263229479,0.171332561266035,
-4.53632503221188));
#31080=CARTESIAN_POINT('Ctrl Pts',(-38.634817323953,2.31771737083191,-3.90330442580641));
#31081=CARTESIAN_POINT('Ctrl Pts',(-38.515908324958,3.90089279206749,-2.32177406796203));
#31082=CARTESIAN_POINT('Ctrl Pts',(-38.396999325963,4.53614443003203,-0.176048509308297));
#31083=CARTESIAN_POINT('Ctrl Pts',(-38.2780903269681,4.06910501960659,2.01245712921353));
#31084=CARTESIAN_POINT('Ctrl Pts',(-38.1591813279731,2.6132659579589,3.71193216628008));
#31085=CARTESIAN_POINT('Ctrl Pts',(-38.0402723289782,0.522398687851519,
4.50940117676266));
#31086=CARTESIAN_POINT('Ctrl Pts',(-37.9213633299832,-1.69541237887717,
4.21107779957103));
#31087=CARTESIAN_POINT('Ctrl Pts',(-37.8024543309883,-3.50123526600386,
2.88945513513179));
#31088=CARTESIAN_POINT('Ctrl Pts',(-37.6835453319932,-4.45625184670795,
0.865689808921497));
#31089=CARTESIAN_POINT('Ctrl Pts',(-37.5646363329983,-4.32839141804354,
-1.36843965844462));
#31090=CARTESIAN_POINT('Ctrl Pts',(-37.4457273340033,-3.14872428825265,
-3.27003589016275));
#31091=CARTESIAN_POINT('Ctrl Pts',(-37.3268183350084,-1.20391163753542,
-4.37700766912383));
#31092=CARTESIAN_POINT('Ctrl Pts',(-37.2079093360134,1.03345365124596,-4.42035891271123));
#31093=CARTESIAN_POINT('Ctrl Pts',(-37.0890003370185,3.0196878914008,-3.38955519279929));
#31094=CARTESIAN_POINT('Ctrl Pts',(-36.9700913380235,4.27213268122689,-1.53508362002973));
#31095=CARTESIAN_POINT('Ctrl Pts',(-36.8511823390285,4.48644174158915,0.692415963000866));
#31096=CARTESIAN_POINT('Ctrl Pts',(-36.7322733400336,3.61053759519256,2.7516572534012));
#31097=CARTESIAN_POINT('Ctrl Pts',(-36.6133643410387,1.85726648484098,4.14224100829228));
#31098=CARTESIAN_POINT('Ctrl Pts',(-36.4944553420436,-0.347323636626779,
4.52625293790943));
#31099=CARTESIAN_POINT('Ctrl Pts',(-36.3755463430487,-2.46751350562725,
3.81037747028294));
#31100=CARTESIAN_POINT('Ctrl Pts',(-36.2566373440537,-3.98809326785784,
2.1685735987879));
#31101=CARTESIAN_POINT('Ctrl Pts',(-36.1377283450588,-4.53955937592,-0.000197458152042056));
#31102=CARTESIAN_POINT('Ctrl Pts',(-36.0188193460638,-3.98790459897951,
-2.1689205324149));
#31103=CARTESIAN_POINT('Ctrl Pts',(-35.8999103470689,-2.46718201473872,
-3.81059211575349));
#31104=CARTESIAN_POINT('Ctrl Pts',(-35.7810013480739,-0.346929876594992,
-4.52628313599787));
#31105=CARTESIAN_POINT('Ctrl Pts',(-35.662092349079,1.85762682963819,-4.14207942081043));
#31106=CARTESIAN_POINT('Ctrl Pts',(-35.543183350084,3.61077696033784,-2.75134314638983));
#31107=CARTESIAN_POINT('Ctrl Pts',(-35.424274351089,4.4865019609327,-0.69202566501534));
#31108=CARTESIAN_POINT('Ctrl Pts',(-35.3053653520941,4.27199912136254,1.53545526589692));
#31109=CARTESIAN_POINT('Ctrl Pts',(-35.1864563530991,3.01939300760999,3.38981787594685));
#31110=CARTESIAN_POINT('Ctrl Pts',(-35.0675473541041,1.03306910080612,4.42044880068217));
#31111=CARTESIAN_POINT('Ctrl Pts',(-34.9486383551092,-1.20429240819219,
4.3769029189672));
#31112=CARTESIAN_POINT('Ctrl Pts',(-34.8297293561142,-3.14900875119183,
3.2697619563831));
#31113=CARTESIAN_POINT('Ctrl Pts',(-34.7108203571192,-4.32851044826741,
1.36806310736485));
#31114=CARTESIAN_POINT('Ctrl Pts',(-34.5919113581243,-4.45617651967321,
-0.866077474597983));
#31115=CARTESIAN_POINT('Ctrl Pts',(-34.4730023591293,-3.50098388629258,
-2.8897597122274));
#31116=CARTESIAN_POINT('Ctrl Pts',(-34.3540933601343,-1.69504603223854,
-4.21122527479655));
#31117=CARTESIAN_POINT('Ctrl Pts',(-34.2351843611394,0.52279097861952,-4.50935571441941));
#31118=CARTESIAN_POINT('Ctrl Pts',(-34.1162753621444,2.61358886535788,-3.71170481172332));
#31119=CARTESIAN_POINT('Ctrl Pts',(-33.9973663631495,4.06928007688015,-2.01210313413584));
#31120=CARTESIAN_POINT('Ctrl Pts',(-33.8784573641545,4.53612909734241,0.176443131734507));
#31121=CARTESIAN_POINT('Ctrl Pts',(-33.7595483651596,3.90069079650883,2.32211340733482));
#31122=CARTESIAN_POINT('Ctrl Pts',(-33.6406393661646,2.31737779523808,3.90350605489873));
#31123=CARTESIAN_POINT('Ctrl Pts',(-33.5217303671696,0.170937927970636,
4.53633988930195));
#31124=CARTESIAN_POINT('Ctrl Pts',(-33.4028213681746,-2.01704015540326,
4.06683517959457));
#31125=CARTESIAN_POINT('Ctrl Pts',(-33.2839123691797,-3.71487394567241,
2.60908239315094));
#31126=CARTESIAN_POINT('Ctrl Pts',(-33.1650033701847,-4.50998685594713,
0.517318012139963));
#31127=CARTESIAN_POINT('Ctrl Pts',(-33.0460943711898,-4.20916505540284,
-1.70015555255108));
#31128=CARTESIAN_POINT('Ctrl Pts',(-32.9271853721948,-2.88550876884117,
-3.50448833803139));
#31129=CARTESIAN_POINT('Ctrl Pts',(-32.8082763731999,-0.86066879390247,
-4.45722431495354));
#31130=CARTESIAN_POINT('Ctrl Pts',(-32.6893673742049,1.37331520645988,-4.32684697093947));
#31131=CARTESIAN_POINT('Ctrl Pts',(-32.57045837521,3.27358120463341,-3.14503822928193));
#31132=CARTESIAN_POINT('Ctrl Pts',(-32.451549376215,4.37836123227121,-1.19897968524445));
#31133=CARTESIAN_POINT('Ctrl Pts',(-32.33264037722,4.41919180651584,1.03843302332628));
#31134=CARTESIAN_POINT('Ctrl Pts',(-32.213731378225,3.3861510257669,3.02350468808081));
#31135=CARTESIAN_POINT('Ctrl Pts',(-32.0948223792301,1.53026961138005,4.27385941232357));
#31136=CARTESIAN_POINT('Ctrl Pts',(-31.9759133802351,-0.697470002040879,
4.48565881220849));
#31137=CARTESIAN_POINT('Ctrl Pts',(-31.8570043812402,-2.75572317987429,
3.60743525098863));
#31138=CARTESIAN_POINT('Ctrl Pts',(-31.7380953822452,-4.1443308001465,1.85259861596859));
#31139=CARTESIAN_POINT('Ctrl Pts',(-31.6191863832503,-4.52585876167512,
-0.352422759922571));
#31140=CARTESIAN_POINT('Ctrl Pts',(-31.5002773842552,-3.80759513219323,
-2.4718047274604));
#31141=CARTESIAN_POINT('Ctrl Pts',(-31.3813683852603,-2.16407917054937,
-3.99053393346338));
#31142=CARTESIAN_POINT('Ctrl Pts',(-31.2624593862654,0.00531174016416774,
-4.53955616057968));
#31143=CARTESIAN_POINT('Ctrl Pts',(-31.1435503872704,2.1734120531481,-3.98545876017553));
#31144=CARTESIAN_POINT('Ctrl Pts',(-31.0246413882754,3.81336909977593,-2.46288694577852));
#31145=CARTESIAN_POINT('Ctrl Pts',(-30.9057323892805,4.52667142565262,-0.341831181417046));
#31146=CARTESIAN_POINT('Ctrl Pts',(-30.7868233902855,4.1399833557953,1.86229393857194));
#31147=CARTESIAN_POINT('Ctrl Pts',(-30.6679143912906,2.747274677826,3.6138708283215));
#31148=CARTESIAN_POINT('Ctrl Pts',(-30.5490053922956,0.68696824420526,4.48728581137539));
#31149=CARTESIAN_POINT('Ctrl Pts',(-30.4300963933006,-1.54026231658092,
4.27025247770333));
#31150=CARTESIAN_POINT('Ctrl Pts',(-30.3111873943057,-3.39322710136354,
3.01560015776149));
#31151=CARTESIAN_POINT('Ctrl Pts',(-30.1922783953107,-4.42159052456228,
1.02803222045517));
#31152=CARTESIAN_POINT('Ctrl Pts',(-30.0733693963157,-4.37558197978096,
-1.20910960083043));
#31153=CARTESIAN_POINT('Ctrl Pts',(-29.9544603973208,-3.26613442579243,
-3.15293051555816));
#31154=CARTESIAN_POINT('Ctrl Pts',(-29.8751877313241,-1.99759989989656,
-3.93718287761652));
#31155=CARTESIAN_POINT('Ctrl Pts',(-29.8355513983258,-1.30786439202401,
-4.15432535756651));
#31156=CARTESIAN_POINT('Ctrl Pts',(-52.7394486016742,-2.0429884765144,4.16621468233141));
#31157=CARTESIAN_POINT('Ctrl Pts',(-52.6998122686759,-2.73469794856865,
3.82702081253498));
#31158=CARTESIAN_POINT('Ctrl Pts',(-52.6205396026792,-3.94521181740615,
2.79778579341567));
#31159=CARTESIAN_POINT('Ctrl Pts',(-52.5016306036842,-4.80242437368079,
0.572672151973649));
#31160=CARTESIAN_POINT('Ctrl Pts',(-52.3827216046893,-4.49254494566273,
-1.79105419433853));
#31161=CARTESIAN_POINT('Ctrl Pts',(-52.2638126056943,-3.09101748341397,
-3.71981693483926));
#31162=CARTESIAN_POINT('Ctrl Pts',(-52.1449036066994,-0.938343069574278,
-4.74452517527442));
#31163=CARTESIAN_POINT('Ctrl Pts',(-52.0259946077044,1.44233817363076,-4.61637183234714));
#31164=CARTESIAN_POINT('Ctrl Pts',(-51.9070856087094,3.47253481969342,-3.36639878522093));
#31165=CARTESIAN_POINT('Ctrl Pts',(-51.7881766097145,4.65889635654337,-1.29840160493764));
#31166=CARTESIAN_POINT('Ctrl Pts',(-51.6692676107195,4.71313944774054,1.08511779895128));
#31167=CARTESIAN_POINT('Ctrl Pts',(-51.5503586117246,3.62208062282748,3.20494748589602));
#31168=CARTESIAN_POINT('Ctrl Pts',(-51.4314496127296,1.65085024372788,4.54597141676343));
#31169=CARTESIAN_POINT('Ctrl Pts',(-51.3125406137347,-0.721539831467189,
4.78231527249984));
#31170=CARTESIAN_POINT('Ctrl Pts',(-51.1936316147397,-2.91859436601119,
3.85654866273941));
#31171=CARTESIAN_POINT('Ctrl Pts',(-51.0747226157447,-4.40642540268035,
1.99363370379486));
#31172=CARTESIAN_POINT('Ctrl Pts',(-50.9558136167498,-4.82348731883206,
-0.353737606829587));
#31173=CARTESIAN_POINT('Ctrl Pts',(-50.8369046177547,-4.06843337441483,
-2.61515012548823));
#31174=CARTESIAN_POINT('Ctrl Pts',(-50.7179956187599,-2.32474298299854,
-4.24107654664407));
#31175=CARTESIAN_POINT('Ctrl Pts',(-50.5990866197648,-0.0161359751194769,
-4.8364139501862));
#31176=CARTESIAN_POINT('Ctrl Pts',(-50.4801776207699,2.29639210453432,-4.25649427849261));
#31177=CARTESIAN_POINT('Ctrl Pts',(-50.3612686217749,4.05089287704335,-2.64223904081009));
#31178=CARTESIAN_POINT('Ctrl Pts',(-50.24235962278,4.82101958066735,-0.385915082954782));
#31179=CARTESIAN_POINT('Ctrl Pts',(-50.123450623785,4.4196300760155,1.96418691541067));
#31180=CARTESIAN_POINT('Ctrl Pts',(-50.00454162479,2.94426271653953,3.83698805115724));
#31181=CARTESIAN_POINT('Ctrl Pts',(-49.8856326257952,0.753434356377266,
4.77739436497606));
#31182=CARTESIAN_POINT('Ctrl Pts',(-49.7667236268001,-1.62047987293258,
4.5568854747224));
#31183=CARTESIAN_POINT('Ctrl Pts',(-49.6478146278053,-3.60061465285689,
3.22904542702235));
#31184=CARTESIAN_POINT('Ctrl Pts',(-49.5289056288102,-4.70579376119999,
1.11654168092161));
#31185=CARTESIAN_POINT('Ctrl Pts',(-49.4099966298152,-4.66745673755532,
-1.26728365066384));
#31186=CARTESIAN_POINT('Ctrl Pts',(-49.2910876308203,-3.49491954585864,
-3.34315683391453));
#31187=CARTESIAN_POINT('Ctrl Pts',(-49.1721786318254,-1.47311077884397,
-4.60663704685322));
#31188=CARTESIAN_POINT('Ctrl Pts',(-49.0532696328303,0.90666648940606,-4.75069638318088));
#31189=CARTESIAN_POINT('Ctrl Pts',(-48.9343606338354,3.06612221158225,-3.74032817167489));
#31190=CARTESIAN_POINT('Ctrl Pts',(-48.8154516348404,4.48050486223793,-1.82105365863946));
#31191=CARTESIAN_POINT('Ctrl Pts',(-48.6965426358454,4.8061169782227,0.540740085273374));
#31192=CARTESIAN_POINT('Ctrl Pts',(-48.5776336368505,3.9638342446399,2.7711330406897));
#31193=CARTESIAN_POINT('Ctrl Pts',(-48.4587246378556,2.15833284205031,4.32813581015072));
#31194=CARTESIAN_POINT('Ctrl Pts',(-48.3398156388606,-0.171647224147517,
4.83339399166099));
#31195=CARTESIAN_POINT('Ctrl Pts',(-48.2209066398656,-2.45991671402506,
4.16412896152871));
#31196=CARTESIAN_POINT('Ctrl Pts',(-48.1019976408707,-4.15042213080724,
2.4829732951217));
#31197=CARTESIAN_POINT('Ctrl Pts',(-47.9830886418757,-4.83236769520448,
0.198450766000718));
#31198=CARTESIAN_POINT('Ctrl Pts',(-47.8641796428808,-4.34003943979692,
-2.13429564709045));
#31199=CARTESIAN_POINT('Ctrl Pts',(-47.7452706438857,-2.79307399357064,
-3.9484044770795));
#31200=CARTESIAN_POINT('Ctrl Pts',(-47.6263616448909,-0.567386671382312,
-4.80304409862326));
#31201=CARTESIAN_POINT('Ctrl Pts',(-47.5074526458958,1.79617660643157,-4.49053558572806));
#31202=CARTESIAN_POINT('Ctrl Pts',(-47.3885436469009,3.72326582065724,-3.08681905477267));
#31203=CARTESIAN_POINT('Ctrl Pts',(-47.2696346479059,4.74559491455711,-0.933000083125277));
#31204=CARTESIAN_POINT('Ctrl Pts',(-47.150725648911,4.61473612643938,1.44753954402541));
#31205=CARTESIAN_POINT('Ctrl Pts',(-47.031816649916,3.36248837117773,3.47632452482166));
#31206=CARTESIAN_POINT('Ctrl Pts',(-46.9129076509211,1.29315004816182,4.66035655300334));
#31207=CARTESIAN_POINT('Ctrl Pts',(-46.7939986519261,-1.09042600310945,
4.71191377042543));
#31208=CARTESIAN_POINT('Ctrl Pts',(-46.6750896529311,-3.20902662439505,
3.61846768288813));
#31209=CARTESIAN_POINT('Ctrl Pts',(-46.5561806539363,-4.54782815137267,
1.64572760618649));
#31210=CARTESIAN_POINT('Ctrl Pts',(-46.4372716549411,-4.78149946641965,
-0.726927163346267));
#31211=CARTESIAN_POINT('Ctrl Pts',(-46.3183626559463,-3.8532580304152,-2.9229373580737));
#31212=CARTESIAN_POINT('Ctrl Pts',(-46.1994536569512,-1.98866813927163,
-4.40866865164845));
#31213=CARTESIAN_POINT('Ctrl Pts',(-46.0805446579564,0.359171595327386,
-4.82308573563571));
#31214=CARTESIAN_POINT('Ctrl Pts',(-45.9616356589613,2.61973200272841,-4.06548453226198));
#31215=CARTESIAN_POINT('Ctrl Pts',(-45.8427266599665,4.24369294176513,-2.31996346182361));
#31216=CARTESIAN_POINT('Ctrl Pts',(-45.7238176609714,4.83642905787465,-0.0106872038750072));
#31217=CARTESIAN_POINT('Ctrl Pts',(-45.6049086619765,4.25390443593254,2.3011860633449));
#31218=CARTESIAN_POINT('Ctrl Pts',(-45.4859996629815,2.63767358008176,4.05386708380217));
#31219=CARTESIAN_POINT('Ctrl Pts',(-45.3670906639866,0.380483421124782,
4.8214512975237));
#31220=CARTESIAN_POINT('Ctrl Pts',(-45.2481816649916,-1.96916487605686,
4.41741439522765));
#31221=CARTESIAN_POINT('Ctrl Pts',(-45.1292726659966,-3.84030265692052,
2.93993805229097));
#31222=CARTESIAN_POINT('Ctrl Pts',(-45.0103636670017,-4.77824016112727,
0.748051609777494));
#31223=CARTESIAN_POINT('Ctrl Pts',(-44.8914546680067,-4.5550569311501,-1.6256126851861));
#31224=CARTESIAN_POINT('Ctrl Pts',(-44.7725456690118,-3.22498688314855,
-3.60425024810576));
#31225=CARTESIAN_POINT('Ctrl Pts',(-44.6536366700168,-1.1112393698635,-4.70704868397537));
#31226=CARTESIAN_POINT('Ctrl Pts',(-44.5347276710218,1.27254125776094,-4.66602603833752));
#31227=CARTESIAN_POINT('Ctrl Pts',(-44.4158186720269,3.34709212981373,-3.49115088922637));
#31228=CARTESIAN_POINT('Ctrl Pts',(-44.2969096730319,4.60829374676278,-1.46791995065565));
#31229=CARTESIAN_POINT('Ctrl Pts',(-44.1780006740369,4.74967190808896,0.912018100208794));
#31230=CARTESIAN_POINT('Ctrl Pts',(-44.059091675042,3.736871466898,3.0703341713363));
#31231=CARTESIAN_POINT('Ctrl Pts',(-43.940182676047,1.81600471732796,4.48255362314666));
#31232=CARTESIAN_POINT('Ctrl Pts',(-43.8212736770521,-0.546154377151393,
4.80550475600336));
#31233=CARTESIAN_POINT('Ctrl Pts',(-43.7023646780571,-2.77559696955997,
3.96070967430342));
#31234=CARTESIAN_POINT('Ctrl Pts',(-43.5834556790621,-4.33056469562674,
2.15345547107664));
#31235=CARTESIAN_POINT('Ctrl Pts',(-43.4645466800672,-4.83319748633371,
-0.17709272746758));
#31236=CARTESIAN_POINT('Ctrl Pts',(-43.3456376810722,-4.16135506385137,
-2.46460600286104));
#31237=CARTESIAN_POINT('Ctrl Pts',(-43.2267286820773,-2.47829557375599,
-4.15321785406617));
#31238=CARTESIAN_POINT('Ctrl Pts',(-43.1078196830823,-0.193006899530237,
-4.83258618986839));
#31239=CARTESIAN_POINT('Ctrl Pts',(-42.9889106840873,2.13918475261367,-4.33763618354885));
#31240=CARTESIAN_POINT('Ctrl Pts',(-42.8700016850924,3.95154684462089,-2.78861588215986));
#31241=CARTESIAN_POINT('Ctrl Pts',(-42.7510926860974,4.80368393854071,-0.561991143777627));
#31242=CARTESIAN_POINT('Ctrl Pts',(-42.6321836871025,4.48850183427287,1.80126646943557));
#31243=CARTESIAN_POINT('Ctrl Pts',(-42.5132746881075,3.08263699872303,3.72667744534695));
#31244=CARTESIAN_POINT('Ctrl Pts',(-42.3943656891126,0.927623968672873,
4.74677001683145));
#31245=CARTESIAN_POINT('Ctrl Pts',(-42.2754566901175,-1.45267963417639,
4.6128490766745));
#31246=CARTESIAN_POINT('Ctrl Pts',(-42.1565476911226,-3.48022624863131,
3.35907505239722));
#31247=CARTESIAN_POINT('Ctrl Pts',(-42.0376386921276,-4.66157965137196,
1.28689095585245));
#31248=CARTESIAN_POINT('Ctrl Pts',(-41.9187296931327,-4.71114278964874,
-1.09372420553542));
#31249=CARTESIAN_POINT('Ctrl Pts',(-41.7998206941377,-3.61393072426332,
-3.21709883313528));
#31250=CARTESIAN_POINT('Ctrl Pts',(-41.6809116951427,-1.64244694706527,
-4.54184166612561));
#31251=CARTESIAN_POINT('Ctrl Pts',(-41.5223663631495,1.52894460133419,-4.87830739976151));
#31252=CARTESIAN_POINT('Ctrl Pts',(-41.3241846981579,4.99877807903749,-2.25841532927366));
#31253=CARTESIAN_POINT('Ctrl Pts',(-41.086366700168,4.60241820340005,2.9842869774832));
#31254=CARTESIAN_POINT('Ctrl Pts',(-40.8881850351763,0.778136400847418,
5.05272781991995));
#31255=CARTESIAN_POINT('Ctrl Pts',(-40.7296397031831,-2.30662180443871,
4.24328334493074));
#31256=CARTESIAN_POINT('Ctrl Pts',(-40.6107307041881,-4.05652828451666,
2.63719518785605));
#31257=CARTESIAN_POINT('Ctrl Pts',(-40.4918217051932,-4.82203002291603,
0.372995281913602));
#31258=CARTESIAN_POINT('Ctrl Pts',(-40.3729127061982,-4.41511643585742,
-1.97310923067162));
#31259=CARTESIAN_POINT('Ctrl Pts',(-40.2540037072032,-2.9356480856696,-3.84412932488023));
#31260=CARTESIAN_POINT('Ctrl Pts',(-40.1350947082083,-0.742648649291964,
-4.77882074443397));
#31261=CARTESIAN_POINT('Ctrl Pts',(-40.0161857092133,1.63073377662217,-4.55335251981767));
#31262=CARTESIAN_POINT('Ctrl Pts',(-39.8972767102183,3.60788611023574,-3.22085911879452));
#31263=CARTESIAN_POINT('Ctrl Pts',(-39.7783677112233,4.70829520478864,-1.1059682973522));
#31264=CARTESIAN_POINT('Ctrl Pts',(-39.6594587122285,4.66459063444655,1.27781361712572));
#31265=CARTESIAN_POINT('Ctrl Pts',(-39.5405497132334,3.48737718947312,3.35101497188689));
#31266=CARTESIAN_POINT('Ctrl Pts',(-39.4216407142385,1.462727569112,4.60994871177617));
#31267=CARTESIAN_POINT('Ctrl Pts',(-39.3027317152436,-0.917368714773737,
4.74863934058245));
#31268=CARTESIAN_POINT('Ctrl Pts',(-39.1838227162485,-3.07454214113269,
3.73341105647792));
#31269=CARTESIAN_POINT('Ctrl Pts',(-39.0649137172536,-4.48459676515183,
1.81095294548753));
#31270=CARTESIAN_POINT('Ctrl Pts',(-38.9460047182586,-4.80488635108207,
-0.551567701383731));
#31271=CARTESIAN_POINT('Ctrl Pts',(-38.8270957192637,-3.95758021413045,
-2.7800575349517));
#31272=CARTESIAN_POINT('Ctrl Pts',(-38.7081867202687,-2.14857510737313,
-4.33298796092579));
#31273=CARTESIAN_POINT('Ctrl Pts',(-38.5892777212738,0.18253749572199,-4.83299499547723));
#31274=CARTESIAN_POINT('Ctrl Pts',(-38.4703687222788,2.46929317776407,-4.15857563595885));
#31275=CARTESIAN_POINT('Ctrl Pts',(-38.3514597232838,4.15600628440037,-2.47361517779471));
#31276=CARTESIAN_POINT('Ctrl Pts',(-38.2325507242888,4.8328025821415,-0.187561860846965));
#31277=CARTESIAN_POINT('Ctrl Pts',(-38.1136417252939,4.33521938048628,2.14406929949615));
#31278=CARTESIAN_POINT('Ctrl Pts',(-37.9947327262989,2.78417027152664,3.95468787086344));
#31279=CARTESIAN_POINT('Ctrl Pts',(-37.875823727304,0.556562906339921,4.80431035367553));
#31280=CARTESIAN_POINT('Ctrl Pts',(-37.756914728309,-1.80629022043161,4.48647700206097));
#31281=CARTESIAN_POINT('Ctrl Pts',(-37.6380057293141,-3.73021165776875,
3.07842187422335));
#31282=CARTESIAN_POINT('Ctrl Pts',(-37.5190967303191,-4.74768512414649,
0.922304835840504));
#31283=CARTESIAN_POINT('Ctrl Pts',(-37.4001877313241,-4.6114627839335,-1.45793389448783));
#31284=CARTESIAN_POINT('Ctrl Pts',(-37.2812787323292,-3.35464690453247,
-3.48389213294125));
#31285=CARTESIAN_POINT('Ctrl Pts',(-37.1623697333342,-1.28264594752121,
-4.66325847681296));
#31286=CARTESIAN_POINT('Ctrl Pts',(-37.0434607343393,1.10104022288146,-4.70944483731798));
#31287=CARTESIAN_POINT('Ctrl Pts',(-36.9245517353443,3.21717168928859,-3.61122784795367));
#31288=CARTESIAN_POINT('Ctrl Pts',(-36.8056427363493,4.55152479634309,-1.63547616199481));
#31289=CARTESIAN_POINT('Ctrl Pts',(-36.6867337373544,4.77984940025959,0.737699097884072));
#31290=CARTESIAN_POINT('Ctrl Pts',(-36.5678247383594,3.84666222209386,2.93161218398677));
#31291=CARTESIAN_POINT('Ctrl Pts',(-36.4489157393645,1.9787293817717,4.41313837103418));
#31292=CARTESIAN_POINT('Ctrl Pts',(-36.3300067403695,-0.370038166513298,
4.82226419884955));
#31293=CARTESIAN_POINT('Ctrl Pts',(-36.2110977413745,-2.628885791756,4.05957137418291));
#31294=CARTESIAN_POINT('Ctrl Pts',(-36.0921887423796,-4.24890956185634,
2.31039559022863));
#31295=CARTESIAN_POINT('Ctrl Pts',(-35.9732797433846,-4.83644086120422,
-0.000210371667320702));
#31296=CARTESIAN_POINT('Ctrl Pts',(-35.8543707443896,-4.2487085542702,-2.31076521287933));
#31297=CARTESIAN_POINT('Ctrl Pts',(-35.7354617453947,-2.62853262177948,
-4.05980005719779));
#31298=CARTESIAN_POINT('Ctrl Pts',(-35.6165527463997,-0.369618655069714,
-4.82229637185506));
#31299=CARTESIAN_POINT('Ctrl Pts',(-35.4976437474047,1.97911329266632,-4.41296621593386));
#31300=CARTESIAN_POINT('Ctrl Pts',(-35.3787347484098,3.84691724141916,-2.93127753477115));
#31301=CARTESIAN_POINT('Ctrl Pts',(-35.2598257494148,4.77991355787262,-0.737283274900226));
#31302=CARTESIAN_POINT('Ctrl Pts',(-35.1409167504199,4.55138250183126,1.63587211303519));
#31303=CARTESIAN_POINT('Ctrl Pts',(-35.0220077514249,3.21685752046802,3.61150771024934));
#31304=CARTESIAN_POINT('Ctrl Pts',(-34.9030987524299,1.10063052332557,4.70954060384939));
#31305=CARTESIAN_POINT('Ctrl Pts',(-34.7841897534351,-1.28305162010095,
4.66314687612758));
#31306=CARTESIAN_POINT('Ctrl Pts',(-34.6652807544399,-3.35494997099078,
3.48360028423627));
#31307=CARTESIAN_POINT('Ctrl Pts',(-34.5463717554451,-4.6115895985846,1.45753271744012));
#31308=CARTESIAN_POINT('Ctrl Pts',(-34.4274627564501,-4.74760487081823,
-0.922717854365599));
#31309=CARTESIAN_POINT('Ctrl Pts',(-34.3085537574552,-3.7299438381399,-3.07874637027869));
#31310=CARTESIAN_POINT('Ctrl Pts',(-34.1896447584601,-1.80589991518268,
-4.48663412198111));
#31311=CARTESIAN_POINT('Ctrl Pts',(-34.0707357594653,0.556980852431709,
-4.80426191815211));
#31312=CARTESIAN_POINT('Ctrl Pts',(-33.9518267604702,2.78451429666418,-3.95444564760406));
#31313=CARTESIAN_POINT('Ctrl Pts',(-33.8329177614753,4.33540588628578,-2.14369215358474));
#31314=CARTESIAN_POINT('Ctrl Pts',(-33.7140087624803,4.83278624671323,0.187982291084487));
#31315=CARTESIAN_POINT('Ctrl Pts',(-33.5950997634854,4.15579107858574,2.47397670953652));
#31316=CARTESIAN_POINT('Ctrl Pts',(-33.4761907644904,2.46893139435267,4.1587904513407));
#31317=CARTESIAN_POINT('Ctrl Pts',(-33.3572817654955,0.18211705390445,4.83301082420234));
#31318=CARTESIAN_POINT('Ctrl Pts',(-33.2383727665005,-2.14895204984623,
4.3328010957865));
#31319=CARTESIAN_POINT('Ctrl Pts',(-33.1194637675056,-3.9578220389356,2.77971310683131));
#31320=CARTESIAN_POINT('Ctrl Pts',(-33.0005547685105,-4.80493433554354,
0.55114996081392));
#31321=CARTESIAN_POINT('Ctrl Pts',(-32.8816457695156,-4.48443916682499,
-1.81134359171032));
#31322=CARTESIAN_POINT('Ctrl Pts',(-32.7627367705206,-3.07421742053067,
-3.73367747662374));
#31323=CARTESIAN_POINT('Ctrl Pts',(-32.6438277715257,-0.916955452741436,
-4.74872119059472));
#31324=CARTESIAN_POINT('Ctrl Pts',(-32.5249187725307,1.46312829722367,-4.60981733192737));
#31325=CARTESIAN_POINT('Ctrl Pts',(-32.4060097735358,3.48766930652834,-3.35071978193168));
#31326=CARTESIAN_POINT('Ctrl Pts',(-32.2871007745408,4.66470056129123,-1.27739145174084));
#31327=CARTESIAN_POINT('Ctrl Pts',(-32.1681917755458,4.70820140384233,1.1063452396459));
#31328=CARTESIAN_POINT('Ctrl Pts',(-32.0492827765509,3.60760105267017,3.22123809968074));
#31329=CARTESIAN_POINT('Ctrl Pts',(-31.9303737775559,1.63034732322182,4.55336445348616));
#31330=CARTESIAN_POINT('Ctrl Pts',(-31.811464778561,-0.743083664733639,
4.77901526828014));
#31331=CARTESIAN_POINT('Ctrl Pts',(-31.692555779566,-2.93594401694779,3.84335698847294));
#31332=CARTESIAN_POINT('Ctrl Pts',(-31.573646780571,-4.41536483265262,1.97375624013402));
#31333=CARTESIAN_POINT('Ctrl Pts',(-31.4547377815761,-4.82184424398428,
-0.37547076607239));
#31334=CARTESIAN_POINT('Ctrl Pts',(-31.3358287825811,-4.05660707467442,
-2.63345765411083));
#31335=CARTESIAN_POINT('Ctrl Pts',(-31.2169197835861,-2.30560723202455,
-4.25150984392904));
#31336=CARTESIAN_POINT('Ctrl Pts',(-31.0980107845912,0.00565912130376327,
-4.83643743558468));
#31337=CARTESIAN_POINT('Ctrl Pts',(-30.9791017855962,2.31555047343088,-4.24610276067837));
#31338=CARTESIAN_POINT('Ctrl Pts',(-30.8601927866012,4.06275865248972,-2.6239566607003));
#31339=CARTESIAN_POINT('Ctrl Pts',(-30.7412837876063,4.82271005516587,-0.36418651162684));
#31340=CARTESIAN_POINT('Ctrl Pts',(-30.6223747886113,4.41073307089764,1.98408562466634));
#31341=CARTESIAN_POINT('Ctrl Pts',(-30.5034657896164,2.92694299346985,3.85021344448564));
#31342=CARTESIAN_POINT('Ctrl Pts',(-30.3845567906214,0.731895105117071,
4.78074867115039));
#31343=CARTESIAN_POINT('Ctrl Pts',(-30.2656477916264,-1.64099353880028,
4.54952162986908));
#31344=CARTESIAN_POINT('Ctrl Pts',(-30.1467387926315,-3.61513989472913,
3.21281662300008));
#31345=CARTESIAN_POINT('Ctrl Pts',(-30.0278297936365,-4.7107569950382,1.09526423732179));
#31346=CARTESIAN_POINT('Ctrl Pts',(-29.9089207946416,-4.66173954917656,
-1.28818385109136));
#31347=CARTESIAN_POINT('Ctrl Pts',(-29.7900117956466,-3.47973551769813,
-3.35912821382421));
#31348=CARTESIAN_POINT('Ctrl Pts',(-29.71073912965,-2.12824042603018,-4.19466969599423));
#31349=CARTESIAN_POINT('Ctrl Pts',(-29.6711027966516,-1.39339708167538,
-4.42601302158308));
#31350=CARTESIAN_POINT('Ctrl Pts',(-52.575,-2.16839587231062,4.42195480991679));
#31351=CARTESIAN_POINT('Ctrl Pts',(-52.5353636670017,-2.90256543874872,
4.06193976546852));
#31352=CARTESIAN_POINT('Ctrl Pts',(-52.4560910010051,-4.18738584118213,
2.9695258861188));
#31353=CARTESIAN_POINT('Ctrl Pts',(-52.3371820020101,-5.09721778105195,
0.607825225057359));
#31354=CARTESIAN_POINT('Ctrl Pts',(-52.2182730030151,-4.76831662455853,
-1.90099678325861));
#31355=CARTESIAN_POINT('Ctrl Pts',(-52.0993640040201,-3.28075739502472,
-3.94815525392406));
#31356=CARTESIAN_POINT('Ctrl Pts',(-51.9804550050252,-0.995942592073579,
-5.03576448149704));
#31357=CARTESIAN_POINT('Ctrl Pts',(-51.8615460060302,1.53087507743214,-4.8997445366854));
#31358=CARTESIAN_POINT('Ctrl Pts',(-51.7426370070352,3.68569390186919,-3.57304278234542));
#31359=CARTESIAN_POINT('Ctrl Pts',(-51.6237280080403,4.94487939857967,-1.3781030647573));
#31360=CARTESIAN_POINT('Ctrl Pts',(-51.5048190090453,5.00245216338252,1.15172698390898));
#31361=CARTESIAN_POINT('Ctrl Pts',(-51.3859100100504,3.84441946785506,3.40168090974558));
#31362=CARTESIAN_POINT('Ctrl Pts',(-51.2670010110554,1.75218651277466,4.8250226416206));
#31363=CARTESIAN_POINT('Ctrl Pts',(-51.1480920120605,-0.765831041264851,
5.07587429698539));
#31364=CARTESIAN_POINT('Ctrl Pts',(-51.0291830130655,-3.09775020709136,
4.093280161774));
#31365=CARTESIAN_POINT('Ctrl Pts',(-50.9102740140705,-4.67691069463037,
2.11601149194133));
#31366=CARTESIAN_POINT('Ctrl Pts',(-50.7913650150755,-5.11957366012311,
-0.375451538443796));
#31367=CARTESIAN_POINT('Ctrl Pts',(-50.6724560160806,-4.31817126590131,
-2.77567925750427));
#31368=CARTESIAN_POINT('Ctrl Pts',(-50.5535470170856,-2.46744567894858,
-4.50141201657024));
#31369=CARTESIAN_POINT('Ctrl Pts',(-50.4346380180907,-0.0171264704852943,
-5.1332937835567));
#31370=CARTESIAN_POINT('Ctrl Pts',(-50.3157290190957,2.43735450195713,-4.51777615493182));
#31371=CARTESIAN_POINT('Ctrl Pts',(-50.1968200201007,4.2995540575637,-2.80443100664268));
#31372=CARTESIAN_POINT('Ctrl Pts',(-50.0779110211058,5.11695444160483,-0.409604206074291));
#31373=CARTESIAN_POINT('Ctrl Pts',(-49.9590020221108,4.69092592745442,2.08475713337828));
#31374=CARTESIAN_POINT('Ctrl Pts',(-49.8400930231159,3.12499419107588,4.07251883595044));
#31375=CARTESIAN_POINT('Ctrl Pts',(-49.7211840241209,0.799683388920974,
5.07065132305026));
#31376=CARTESIAN_POINT('Ctrl Pts',(-49.6022750251259,-1.71995187835053,
4.8366066512714));
#31377=CARTESIAN_POINT('Ctrl Pts',(-49.483366026131,-3.82163582457242,3.42725808586297));
#31378=CARTESIAN_POINT('Ctrl Pts',(-49.3644570271361,-4.99465556709384,
1.18507979854295));
#31379=CARTESIAN_POINT('Ctrl Pts',(-49.245548028141,-4.95396525249667,-1.3450749569741));
#31380=CARTESIAN_POINT('Ctrl Pts',(-49.1266390291462,-3.70945269854255,
-3.54837414037477));
#31381=CARTESIAN_POINT('Ctrl Pts',(-49.0077300301511,-1.56353663714809,
-4.88941218830188));
#31382=CARTESIAN_POINT('Ctrl Pts',(-48.8888210311562,0.962321567542419,
-5.04231450461531));
#31383=CARTESIAN_POINT('Ctrl Pts',(-48.7699120321612,3.25433394462322,-3.96992555845671));
#31384=CARTESIAN_POINT('Ctrl Pts',(-48.6510030331663,4.75553746916888,-1.93283774335679));
#31385=CARTESIAN_POINT('Ctrl Pts',(-48.5320940341713,5.10113705349954,0.573933031134927));
#31386=CARTESIAN_POINT('Ctrl Pts',(-48.4131850351763,4.20715139287775,2.9412370731073));
#31387=CARTESIAN_POINT('Ctrl Pts',(-48.2942760361814,2.29082056975638,4.59381535109922));
#31388=CARTESIAN_POINT('Ctrl Pts',(-48.1753670371864,-0.182183667021966,
5.13008844702354));
#31389=CARTESIAN_POINT('Ctrl Pts',(-48.0564580381915,-2.61091695339391,
4.41974105862483));
#31390=CARTESIAN_POINT('Ctrl Pts',(-47.9375490391964,-4.40519284384016,
2.63538884633622));
#31391=CARTESIAN_POINT('Ctrl Pts',(-47.8186400402016,-5.12899915208836,
0.21063252524413));
#31392=CARTESIAN_POINT('Ctrl Pts',(-47.6997310412066,-4.60644967659206,
-2.26530786866572));
#31393=CARTESIAN_POINT('Ctrl Pts',(-47.5808220422116,-2.96452485578869,
-4.19077448000068));
#31394=CARTESIAN_POINT('Ctrl Pts',(-47.4619130432167,-0.602215298996013,
-5.09787554736961));
#31395=CARTESIAN_POINT('Ctrl Pts',(-47.3430040442217,1.90643363097778,-4.7661839214922));
#31396=CARTESIAN_POINT('Ctrl Pts',(-47.2240950452267,3.95181584714705,-3.27630124882485));
#31397=CARTESIAN_POINT('Ctrl Pts',(-47.1051860462317,5.03689988596539,-0.990271630198361));
#31398=CARTESIAN_POINT('Ctrl Pts',(-46.9862770472368,4.8980084241329,1.53639573025216));
#31399=CARTESIAN_POINT('Ctrl Pts',(-46.8673680482418,3.56889233031509,3.6897162353536));
#31400=CARTESIAN_POINT('Ctrl Pts',(-46.7484590492469,1.37252914490077,4.94642922816165));
#31401=CARTESIAN_POINT('Ctrl Pts',(-46.629550050252,-1.15736102840716,5.00115124873645));
#31402=CARTESIAN_POINT('Ctrl Pts',(-46.5106410512569,-3.40601044326257,
3.84058475016503));
#31403=CARTESIAN_POINT('Ctrl Pts',(-46.391732052262,-4.82699335056435,1.74674942576816));
#31404=CARTESIAN_POINT('Ctrl Pts',(-46.272823053267,-5.07500841322872,-0.771549070682864));
#31405=CARTESIAN_POINT('Ctrl Pts',(-46.1539140542721,-4.08978753632303,
-3.1023597906353));
#31406=CARTESIAN_POINT('Ctrl Pts',(-46.0350050552771,-2.11074111976858,
-4.67929164384222));
#31407=CARTESIAN_POINT('Ctrl Pts',(-45.9160960562821,0.381219088463907,
-5.11914742602763));
#31408=CARTESIAN_POINT('Ctrl Pts',(-45.7971870572872,2.78054239002277,-4.31504141116849));
#31409=CARTESIAN_POINT('Ctrl Pts',(-45.6782780582922,4.50418901724648,-2.46237277026286));
#31410=CARTESIAN_POINT('Ctrl Pts',(-45.5593690592973,5.13330981861987,-0.0113432302901153));
#31411=CARTESIAN_POINT('Ctrl Pts',(-45.4404600603022,4.51502733672665,2.44244273452252));
#31412=CARTESIAN_POINT('Ctrl Pts',(-45.3215510613074,2.79958529835195,4.30271083389079));
#31413=CARTESIAN_POINT('Ctrl Pts',(-45.2026420623123,0.403839125542828,
5.11741265909362));
#31414=CARTESIAN_POINT('Ctrl Pts',(-45.0837330633175,-2.09004066260118,
4.68857423867596));
#31415=CARTESIAN_POINT('Ctrl Pts',(-44.9648240643224,-4.076036906433,3.12040406038571));
#31416=CARTESIAN_POINT('Ctrl Pts',(-44.8459150653275,-5.07154903779715,
0.793970226246384));
#31417=CARTESIAN_POINT('Ctrl Pts',(-44.7270060663325,-4.83466586385136,
-1.72539976463664));
#31418=CARTESIAN_POINT('Ctrl Pts',(-44.6080970673376,-3.42295041115765,
-3.82549458825203));
#31419=CARTESIAN_POINT('Ctrl Pts',(-44.4891880683426,-1.17945200888858,
-4.99598752241199));
#31420=CARTESIAN_POINT('Ctrl Pts',(-44.3702790693476,1.35065529854657,-4.9524467308241));
#31421=CARTESIAN_POINT('Ctrl Pts',(-44.2513700703527,3.55255100161615,-3.70545270560108));
#31422=CARTESIAN_POINT('Ctrl Pts',(-44.1324610713577,4.89117058355806,-1.55802717366026));
#31423=CARTESIAN_POINT('Ctrl Pts',(-44.0135520723628,5.04122714284792,0.968001683171198));
#31424=CARTESIAN_POINT('Ctrl Pts',(-43.8946430733678,3.96625666631358,3.25880445253356));
#31425=CARTESIAN_POINT('Ctrl Pts',(-43.7757340743728,1.92747887637088,4.75771199181005));
#31426=CARTESIAN_POINT('Ctrl Pts',(-43.6568250753779,-0.579679675472256,
5.10048725045433));
#31427=CARTESIAN_POINT('Ctrl Pts',(-43.5379160763829,-2.94597501707901,
4.20383502301162));
#31428=CARTESIAN_POINT('Ctrl Pts',(-43.419007077388,-4.59639333198412,2.28564380483155));
#31429=CARTESIAN_POINT('Ctrl Pts',(-43.300098078393,-5.12987987935639,-0.187963438693522));
#31430=CARTESIAN_POINT('Ctrl Pts',(-43.181189079398,-4.41679688720981,-2.61589409089269));
#31431=CARTESIAN_POINT('Ctrl Pts',(-43.0622800804031,-2.63042398636866,
-4.40816018058456));
#31432=CARTESIAN_POINT('Ctrl Pts',(-42.9433710814082,-0.204854490899003,
-5.12923105889195));
#31433=CARTESIAN_POINT('Ctrl Pts',(-42.8244620824131,2.27049708845707,-4.60389889816705));
#31434=CARTESIAN_POINT('Ctrl Pts',(-42.7055530834182,4.1941097395405,-2.95979308637708));
#31435=CARTESIAN_POINT('Ctrl Pts',(-42.5866440844232,5.09855466340569,-0.596488570763601));
#31436=CARTESIAN_POINT('Ctrl Pts',(-42.4677350854283,4.76402532964921,1.9118359316052));
#31437=CARTESIAN_POINT('Ctrl Pts',(-42.3488260864333,3.27186248023655,3.95543689199389));
#31438=CARTESIAN_POINT('Ctrl Pts',(-42.2299170874383,0.984565506780792,
5.03814712105775));
#31439=CARTESIAN_POINT('Ctrl Pts',(-42.1110080884434,-1.54185134118429,
4.89600553915921));
#31440=CARTESIAN_POINT('Ctrl Pts',(-41.9920990894484,-3.69385746370658,
3.56526948738689));
#31441=CARTESIAN_POINT('Ctrl Pts',(-41.8731900904534,-4.94772740555443,
1.36588584265797));
#31442=CARTESIAN_POINT('Ctrl Pts',(-41.7542810914585,-5.00033294185268,
-1.16086168864519));
#31443=CARTESIAN_POINT('Ctrl Pts',(-41.6353720924635,-3.83576929355919,
-3.41457815879987));
#31444=CARTESIAN_POINT('Ctrl Pts',(-41.5164630934686,-1.74326738571816,
-4.82063938917464));
#31445=CARTESIAN_POINT('Ctrl Pts',(-41.3579177614753,1.62279777915393,-5.17775883276294));
#31446=CARTESIAN_POINT('Ctrl Pts',(-41.1597360964837,5.30562451907466,-2.39704654933505));
#31447=CARTESIAN_POINT('Ctrl Pts',(-40.9219180984938,4.88493437414144,3.16747531283459));
#31448=CARTESIAN_POINT('Ctrl Pts',(-40.7237364335022,0.825901750836606,
5.36288592646222));
#31449=CARTESIAN_POINT('Ctrl Pts',(-40.5651911015089,-2.4482121447205,4.5037542776015));
#31450=CARTESIAN_POINT('Ctrl Pts',(-40.4462821025139,-4.30553539051999,
2.79907754035943));
#31451=CARTESIAN_POINT('Ctrl Pts',(-40.327373103519,-5.11802690913289,0.395891332227557));
#31452=CARTESIAN_POINT('Ctrl Pts',(-40.208464104524,-4.68613522070281,-2.09422713862094));
#31453=CARTESIAN_POINT('Ctrl Pts',(-40.0895551055291,-3.11585075721193,
-4.08009847168603));
#31454=CARTESIAN_POINT('Ctrl Pts',(-39.970646106534,-0.788235608871022,
-5.07216525979755));
#31455=CARTESIAN_POINT('Ctrl Pts',(-39.8517371075391,1.73083521063125,-4.83285682844052));
#31456=CARTESIAN_POINT('Ctrl Pts',(-39.7328281085442,3.82935363519506,-3.41856926692211));
#31457=CARTESIAN_POINT('Ctrl Pts',(-39.6139191095492,4.99731056001954,-1.17385737533702));
#31458=CARTESIAN_POINT('Ctrl Pts',(-39.4950101105542,4.95092321568535,1.3562512979442));
#31459=CARTESIAN_POINT('Ctrl Pts',(-39.3761011115593,3.70144735997023,3.55671464456224));
#31460=CARTESIAN_POINT('Ctrl Pts',(-39.2571921125643,1.55251606146547,4.8929271374227));
#31461=CARTESIAN_POINT('Ctrl Pts',(-39.1382831135694,-0.973680741408834,
5.04013119191881));
#31462=CARTESIAN_POINT('Ctrl Pts',(-39.0193741145743,-3.26327072556555,
3.96258384105897));
#31463=CARTESIAN_POINT('Ctrl Pts',(-38.9004651155794,-4.75988055063526,
1.92211700510603));
#31464=CARTESIAN_POINT('Ctrl Pts',(-38.7815561165845,-5.09983088518642,
-0.585425292765658));
#31465=CARTESIAN_POINT('Ctrl Pts',(-38.6626471175895,-4.20051346314986,
-2.95070939110744));
#31466=CARTESIAN_POINT('Ctrl Pts',(-38.5437381185946,-2.2804638634703,-4.59896534770147));
#31467=CARTESIAN_POINT('Ctrl Pts',(-38.4248291195996,0.193742430177945,
-5.12966495874259));
#31468=CARTESIAN_POINT('Ctrl Pts',(-38.3059201206046,2.62086898469623,-4.41384684611128));
#31469=CARTESIAN_POINT('Ctrl Pts',(-38.1870111216097,4.41111977673326,-2.6254562876274));
#31470=CARTESIAN_POINT('Ctrl Pts',(-38.0681021226147,5.12946073425098,-0.199075212385634));
#31471=CARTESIAN_POINT('Ctrl Pts',(-37.9491931236197,4.60133374136596,2.27568146977877));
#31472=CARTESIAN_POINT('Ctrl Pts',(-37.8302841246248,2.95507458509439,4.19744357544679));
#31473=CARTESIAN_POINT('Ctrl Pts',(-37.7113751256298,0.590727124828317,
5.09921953058841));
#31474=CARTESIAN_POINT('Ctrl Pts',(-37.5924661266348,-1.91716806198604,
4.76187620455091));
#31475=CARTESIAN_POINT('Ctrl Pts',(-37.4735571276399,-3.95918804953365,
3.26738861331491));
#31476=CARTESIAN_POINT('Ctrl Pts',(-37.3546481286449,-5.03911840158502,
0.978919862759506));
#31477=CARTESIAN_POINT('Ctrl Pts',(-37.23573912965,-4.89453414982347,-1.54742813053104));
#31478=CARTESIAN_POINT('Ctrl Pts',(-37.116830130655,-3.56056952081229,-3.69774837571975));
#31479=CARTESIAN_POINT('Ctrl Pts',(-36.99792113166,-1.36138025750699,-4.94950928450209));
#31480=CARTESIAN_POINT('Ctrl Pts',(-36.8790121326651,1.16862679451695,-4.99853076192473));
#31481=CARTESIAN_POINT('Ctrl Pts',(-36.7601031336701,3.41465548717637,-3.83290050310805));
#31482=CARTESIAN_POINT('Ctrl Pts',(-36.6411941346751,4.83091691145929,-1.73586870395989));
#31483=CARTESIAN_POINT('Ctrl Pts',(-36.5222851356802,5.07325705893003,0.782982232767275));
#31484=CARTESIAN_POINT('Ctrl Pts',(-36.4033761366852,4.08278684899514,3.11156711457234));
#31485=CARTESIAN_POINT('Ctrl Pts',(-36.2844671376903,2.10019227870243,4.68403573377608));
#31486=CARTESIAN_POINT('Ctrl Pts',(-36.1655581386953,-0.392752696399822,
5.11827545978968));
#31487=CARTESIAN_POINT('Ctrl Pts',(-36.0466491397004,-2.79025807788474,
4.30876527808287));
#31488=CARTESIAN_POINT('Ctrl Pts',(-35.9277401407054,-4.50972585585484,
2.45221758166935));
#31489=CARTESIAN_POINT('Ctrl Pts',(-35.8088311417104,-5.13332234648844,
-0.000223285182599037));
#31490=CARTESIAN_POINT('Ctrl Pts',(-35.6899221427155,-4.50951250956089,
-2.45260989334375));
#31491=CARTESIAN_POINT('Ctrl Pts',(-35.5710131437205,-2.78988322882023,
-4.30900799864209));
#31492=CARTESIAN_POINT('Ctrl Pts',(-35.4521041447255,-0.392307433544437,
-5.11830960771226));
#31493=CARTESIAN_POINT('Ctrl Pts',(-35.3331951457306,2.10059975569445,-4.68385301105728));
#31494=CARTESIAN_POINT('Ctrl Pts',(-35.2142861467356,4.08305752250047,-3.11121192315247));
#31495=CARTESIAN_POINT('Ctrl Pts',(-35.0953771477407,5.07332515481253,-0.782540884785113));
#31496=CARTESIAN_POINT('Ctrl Pts',(-34.9764681487457,4.83076588229999,1.73628896017346));
#31497=CARTESIAN_POINT('Ctrl Pts',(-34.8575591497507,3.41432203332604,3.83319754455183));
#31498=CARTESIAN_POINT('Ctrl Pts',(-34.7386501507558,1.16819194584502,4.99863240701661));
#31499=CARTESIAN_POINT('Ctrl Pts',(-34.6197411517608,-1.36181083200972,
4.94939083328796));
#31500=CARTESIAN_POINT('Ctrl Pts',(-34.5008321527658,-3.56089119078974,
3.69743861208944));
#31501=CARTESIAN_POINT('Ctrl Pts',(-34.3819231537709,-4.89466874890179,
1.5470023275154));
#31502=CARTESIAN_POINT('Ctrl Pts',(-34.2630141547759,-5.03903322196325,
-0.979358234133216));
#31503=CARTESIAN_POINT('Ctrl Pts',(-34.144105155781,-3.95890378998724,-3.26773302832997));
#31504=CARTESIAN_POINT('Ctrl Pts',(-34.025196156786,-1.91675379812682,-4.76204296916568));
#31505=CARTESIAN_POINT('Ctrl Pts',(-33.906287157791,0.591170726243899,-5.0991681218848));
#31506=CARTESIAN_POINT('Ctrl Pts',(-33.7873781587961,2.95543972797048,-4.19718648348481));
#31507=CARTESIAN_POINT('Ctrl Pts',(-33.6684691598011,4.60153169569141,-2.27528117303364));
#31508=CARTESIAN_POINT('Ctrl Pts',(-33.5495601608061,5.12944339608405,0.199521450434463));
#31509=CARTESIAN_POINT('Ctrl Pts',(-33.4306511618112,4.41089136066265,2.62584001173821));
#31510=CARTESIAN_POINT('Ctrl Pts',(-33.3117421628162,2.62048499346726,4.41407484778267));
#31511=CARTESIAN_POINT('Ctrl Pts',(-33.1928331638213,0.193296179838262,
5.12968175910273));
#31512=CARTESIAN_POINT('Ctrl Pts',(-33.0739241648263,-2.28086394428919,
4.59876701197841));
#31513=CARTESIAN_POINT('Ctrl Pts',(-32.9550151658314,-4.2007701321988,2.95034382051169));
#31514=CARTESIAN_POINT('Ctrl Pts',(-32.8361061668364,-5.09988181513996,
0.584981909487872));
#31515=CARTESIAN_POINT('Ctrl Pts',(-32.7171971678414,-4.75971327824715,
-1.92253163086956));
#31516=CARTESIAN_POINT('Ctrl Pts',(-32.5982881688464,-3.26292607222017,
-3.96286661521608));
#31517=CARTESIAN_POINT('Ctrl Pts',(-32.4793791698515,-0.973242111580406,
-5.04021806623591));
#31518=CARTESIAN_POINT('Ctrl Pts',(-32.3604701708565,1.55294138798746,-4.89278769291527));
#31519=CARTESIAN_POINT('Ctrl Pts',(-32.2415611718616,3.70175740842325,-3.55640133458143));
#31520=CARTESIAN_POINT('Ctrl Pts',(-32.1226521728666,4.95103989031126,-1.35580321823721));
#31521=CARTESIAN_POINT('Ctrl Pts',(-32.0037431738717,4.99721100116881,1.1742574559655));
#31522=CARTESIAN_POINT('Ctrl Pts',(-31.8848341748767,3.82905107957342,3.41897151128069));
#31523=CARTESIAN_POINT('Ctrl Pts',(-31.7659251758817,1.73042503506359,4.83286949464875));
#31524=CARTESIAN_POINT('Ctrl Pts',(-31.6470161768868,-0.788697327426404,
5.0723717243518));
#31525=CARTESIAN_POINT('Ctrl Pts',(-31.5281071778918,-3.11616485402129,
4.07927872595725));
#31526=CARTESIAN_POINT('Ctrl Pts',(-31.4091981788969,-4.68639886515875,
2.09491386429945));
#31527=CARTESIAN_POINT('Ctrl Pts',(-31.2902891799019,-5.11782972629342,
-0.398518772222211));
#31528=CARTESIAN_POINT('Ctrl Pts',(-31.1713801809069,-4.30561901715562,
-2.79511058076127));
#31529=CARTESIAN_POINT('Ctrl Pts',(-31.052471181912,-2.44713529349973,-4.5124857543947));
#31530=CARTESIAN_POINT('Ctrl Pts',(-30.933562182917,0.00600650244336238,
-5.13331871058968));
#31531=CARTESIAN_POINT('Ctrl Pts',(-30.8146531839221,2.45768889371366,-4.50674676118122));
#31532=CARTESIAN_POINT('Ctrl Pts',(-30.6957441849271,4.31214820520351,-2.78502637562208));
#31533=CARTESIAN_POINT('Ctrl Pts',(-30.5768351859322,5.11874868467912,-0.386541841836633));
#31534=CARTESIAN_POINT('Ctrl Pts',(-30.4579261869371,4.68148278599999,2.10587731076074));
#31535=CARTESIAN_POINT('Ctrl Pts',(-30.3390171879422,3.1066113091137,4.08655606064977));
#31536=CARTESIAN_POINT('Ctrl Pts',(-30.2201081889472,0.776821966028881,
5.0742115309254));
#31537=CARTESIAN_POINT('Ctrl Pts',(-30.1011991899523,-1.74172476101964,
4.82879078203482));
#31538=CARTESIAN_POINT('Ctrl Pts',(-29.9822901909573,-3.83705268809473,
3.41003308823867));
#31539=CARTESIAN_POINT('Ctrl Pts',(-29.8633811919624,-4.99992346551413,
1.16249625418841));
#31540=CARTESIAN_POINT('Ctrl Pts',(-29.7444721929674,-4.94789711857216,
-1.3672581013523));
#31541=CARTESIAN_POINT('Ctrl Pts',(-29.6255631939724,-3.69333660960383,
-3.56532591209026));
#31542=CARTESIAN_POINT('Ctrl Pts',(-29.5462905279758,-2.2588809521638,-4.45215651437195));
#31543=CARTESIAN_POINT('Ctrl Pts',(-29.5066541949775,-1.47892977132675,
-4.69770068559965));
#31544=CARTESIAN_POINT('',(-30.,-3.42872620889076,3.53545776165769));
#31545=CARTESIAN_POINT('Ctrl Pts',(-30.,-3.42895048616045,3.53554286219762));
#31546=CARTESIAN_POINT('Ctrl Pts',(-30.,-3.50915824907527,3.44370185733568));
#31547=CARTESIAN_POINT('Ctrl Pts',(-30.,-3.5858151589605,3.34898224904683));
#31548=CARTESIAN_POINT('Ctrl Pts',(-30.,-3.65871285115596,3.25152489539123));
#31549=CARTESIAN_POINT('Ctrl Pts',(-30.,-3.74535380187751,3.1356940985412));
#31550=CARTESIAN_POINT('Ctrl Pts',(-30.,-3.8266858316306,3.01599591628009));
#31551=CARTESIAN_POINT('Ctrl Pts',(-30.,-3.90252528247381,2.89283180563127));
#31552=CARTESIAN_POINT('Ctrl Pts',(-30.,-3.94702891750592,2.82055740796055));
#31553=CARTESIAN_POINT('Ctrl Pts',(-30.,-3.98964027665325,2.74708912193236));
#31554=CARTESIAN_POINT('Ctrl Pts',(-30.,-4.03031418131548,2.67250586558729));
#31555=CARTESIAN_POINT('Ctrl Pts',(-30.,-4.05883144322561,2.62021410080679));
#31556=CARTESIAN_POINT('Ctrl Pts',(-30.,-4.08639618876187,2.56737422065883));
#31557=CARTESIAN_POINT('Ctrl Pts',(-30.,-4.11299101272886,2.51401321575239));
#31558=CARTESIAN_POINT('Ctrl Pts',(-30.,-4.1267818975772,2.48634258800281));
#31559=CARTESIAN_POINT('Ctrl Pts',(-30.,-4.1403138718257,2.45852754287451));
#31560=CARTESIAN_POINT('Ctrl Pts',(-30.,-4.15357199197421,2.43059854489151));
#31561=CARTESIAN_POINT('Ctrl Pts',(-30.,-4.21456648083399,2.30211012140037));
#31562=CARTESIAN_POINT('Ctrl Pts',(-30.,-4.26981903788002,2.17111455395773));
#31563=CARTESIAN_POINT('Ctrl Pts',(-30.,-4.31915507771131,2.03799840069774));
#31564=CARTESIAN_POINT('Ctrl Pts',(-30.,-4.36809646707205,1.90594707454391));
#31565=CARTESIAN_POINT('Ctrl Pts',(-30.,-4.41121576257342,1.77180819965443));
#31566=CARTESIAN_POINT('Ctrl Pts',(-30.,-4.44829211824752,1.63595208979158));
#31567=CARTESIAN_POINT('Ctrl Pts',(-30.,-4.4740200136751,1.54167929182643));
#31568=CARTESIAN_POINT('Ctrl Pts',(-30.,-4.49683706950385,1.44657946040838));
#31569=CARTESIAN_POINT('Ctrl Pts',(-30.,-4.51665445828582,1.35077716111864));
#31570=CARTESIAN_POINT('Ctrl Pts',(-30.,-4.52076402557002,1.33091046731537));
#31571=CARTESIAN_POINT('Ctrl Pts',(-30.,-4.52474455448724,1.31101357182006));
#31572=CARTESIAN_POINT('Ctrl Pts',(-30.,-4.5285951840834,1.29108759749586));
#31573=CARTESIAN_POINT('Ctrl Pts',(-30.,-4.53235404910015,1.2716364802327));
#31574=CARTESIAN_POINT('Ctrl Pts',(-30.,-4.53598714329179,1.25216794356776));
#31575=CARTESIAN_POINT('Ctrl Pts',(-30.,-4.53949403413647,1.23268315058861));
#31576=CARTESIAN_POINT('Ctrl Pts',(-30.,-4.54971861620548,1.17587389311906));
#31577=CARTESIAN_POINT('Ctrl Pts',(-30.,-4.55887057855727,1.11892613790267));
#31578=CARTESIAN_POINT('Ctrl Pts',(-30.,-4.56693872096676,1.06186566568387));
#31579=CARTESIAN_POINT('Ctrl Pts',(-30.,-4.58634448579418,0.924621917542047));
#31580=CARTESIAN_POINT('Ctrl Pts',(-30.,-4.59948384692545,0.78672603593175));
#31581=CARTESIAN_POINT('Ctrl Pts',(-30.,-4.60642482463028,0.648594114271953));
#31582=CARTESIAN_POINT('Ctrl Pts',(-30.,-4.61338602653636,0.510059712169018));
#31583=CARTESIAN_POINT('Ctrl Pts',(-30.,-4.61411251727511,0.371287074813086));
#31584=CARTESIAN_POINT('Ctrl Pts',(-30.,-4.60862117424193,0.232702680772997));
#31585=CARTESIAN_POINT('Ctrl Pts',(-30.,-4.60321431390715,0.0962503668985886));
#31586=CARTESIAN_POINT('Ctrl Pts',(-30.,-4.59177918602515,-0.0400201649351817));
#31587=CARTESIAN_POINT('Ctrl Pts',(-30.,-4.57428528182906,-0.175683987839321));
#31588=CARTESIAN_POINT('Ctrl Pts',(-30.,-4.56307291200204,-0.262635015894491));
#31589=CARTESIAN_POINT('Ctrl Pts',(-30.,-4.54937072347399,-0.349336422774511));
#31590=CARTESIAN_POINT('Ctrl Pts',(-30.,-4.53316113535111,-0.435670359101438));
#31591=CARTESIAN_POINT('Ctrl Pts',(-30.,-4.52960775784034,-0.454596013808723));
#31592=CARTESIAN_POINT('Ctrl Pts',(-30.,-4.52593385944817,-0.473503988545268));
#31593=CARTESIAN_POINT('Ctrl Pts',(-30.,-4.52213920851564,-0.492393004726145));
#31594=CARTESIAN_POINT('Ctrl Pts',(-30.,-4.51862269595122,-0.509897503535277));
#31595=CARTESIAN_POINT('Ctrl Pts',(-30.,-4.51500446283229,-0.527375860827068));
#31596=CARTESIAN_POINT('Ctrl Pts',(-30.,-4.51128474310241,-0.544826751555983));
#31597=CARTESIAN_POINT('Ctrl Pts',(-30.,-4.48314120023153,-0.676860863540087));
#31598=CARTESIAN_POINT('Ctrl Pts',(-30.,-4.44919041908381,-0.807332295944959));
#31599=CARTESIAN_POINT('Ctrl Pts',(-30.,-4.40946707177224,-0.935850920961004));
#31600=CARTESIAN_POINT('Ctrl Pts',(-30.,-4.38257271922611,-1.02286335681679));
#31601=CARTESIAN_POINT('Ctrl Pts',(-30.,-4.35303126425028,-1.10898042810463));
#31602=CARTESIAN_POINT('Ctrl Pts',(-30.,-4.32084099235389,-1.19407565851423));
#31603=CARTESIAN_POINT('Ctrl Pts',(-30.,-4.27308790247552,-1.32031131750617));
#31604=CARTESIAN_POINT('Ctrl Pts',(-30.,-4.21950722125047,-1.44429998404022));
#31605=CARTESIAN_POINT('Ctrl Pts',(-30.,-4.16031888721692,-1.56567294676739));
#31606=CARTESIAN_POINT('Ctrl Pts',(-30.,-4.10160826700295,-1.68606629851947));
#31607=CARTESIAN_POINT('Ctrl Pts',(-30.,-4.03737956959752,-1.80388657460641));
#31608=CARTESIAN_POINT('Ctrl Pts',(-30.,-3.96781310771827,-1.91873618474768));
#31609=CARTESIAN_POINT('Ctrl Pts',(-30.,-3.94906147189672,-1.94969389059385));
#31610=CARTESIAN_POINT('Ctrl Pts',(-30.,-3.92992184197122,-1.98043551594257));
#31611=CARTESIAN_POINT('Ctrl Pts',(-30.,-3.91039740038924,-2.01095271663753));
#31612=CARTESIAN_POINT('Ctrl Pts',(-30.,-3.89784637190895,-2.03057029460784));
#31613=CARTESIAN_POINT('Ctrl Pts',(-30.,-3.88513632143196,-2.05009512650469));
#31614=CARTESIAN_POINT('Ctrl Pts',(-30.,-3.87226806614249,-2.06952493918974));
#31615=CARTESIAN_POINT('Ctrl Pts',(-30.,-3.8625180853102,-2.08424646102723));
#31616=CARTESIAN_POINT('Ctrl Pts',(-30.,-3.85267751973718,-2.09891297868158));
#31617=CARTESIAN_POINT('Ctrl Pts',(-30.,-3.84275441273704,-2.11351248267563));
#31618=CARTESIAN_POINT('Ctrl Pts',(-30.,-3.76866004569854,-2.22252481192893));
#31619=CARTESIAN_POINT('Ctrl Pts',(-30.,-3.68986014466549,-2.32796611537092));
#31620=CARTESIAN_POINT('Ctrl Pts',(-30.,-3.60658842790908,-2.42951355313142));
#31621=CARTESIAN_POINT('Ctrl Pts',(-30.,-3.52423619248041,-2.52993971014333));
#31622=CARTESIAN_POINT('Ctrl Pts',(-30.,-3.43750975231292,-2.62655802487046));
#31623=CARTESIAN_POINT('Ctrl Pts',(-30.,-3.34660114632163,-2.71901920330891));
#31624=CARTESIAN_POINT('Ctrl Pts',(-30.,-3.26049065975227,-2.8066003181802));
#31625=CARTESIAN_POINT('Ctrl Pts',(-30.,-3.1706272005035,-2.8904516534147));
#31626=CARTESIAN_POINT('Ctrl Pts',(-30.,-3.07715232424116,-2.97023901552393));
#31627=CARTESIAN_POINT('Ctrl Pts',(-30.,-3.01100240161384,-3.02670261345746));
#31628=CARTESIAN_POINT('Ctrl Pts',(-30.,-2.94304331188841,-3.0811300988234));
#31629=CARTESIAN_POINT('Ctrl Pts',(-30.,-2.87337762503368,-3.13344777611549));
#31630=CARTESIAN_POINT('Ctrl Pts',(-30.,-2.83651942594881,-3.1611276204169));
#31631=CARTESIAN_POINT('Ctrl Pts',(-30.,-2.79918348293621,-3.18821672602252));
#31632=CARTESIAN_POINT('Ctrl Pts',(-30.,-2.76138482187608,-3.21470302668161));
#31633=CARTESIAN_POINT('Ctrl Pts',(-30.,-2.74112373262897,-3.2289003894037));
#31634=CARTESIAN_POINT('Ctrl Pts',(-30.,-2.72072969185338,-3.24292453759925));
#31635=CARTESIAN_POINT('Ctrl Pts',(-30.,-2.70020500874655,-3.25677351535391));
#31636=CARTESIAN_POINT('Ctrl Pts',(-30.,-2.68589781217084,-3.26642725987592));
#31637=CARTESIAN_POINT('Ctrl Pts',(-30.,-2.67153139302699,-3.27599297571375));
#31638=CARTESIAN_POINT('Ctrl Pts',(-30.,-2.65711296641173,-3.2854660917133));
#31639=CARTESIAN_POINT('Ctrl Pts',(-30.,-2.54789875315275,-3.35722141832476));
#31640=CARTESIAN_POINT('Ctrl Pts',(-30.,-2.43559241880322,-3.42374262101484));
#31641=CARTESIAN_POINT('Ctrl Pts',(-30.,-2.32058110672905,-3.48486248573992));
#31642=CARTESIAN_POINT('Ctrl Pts',(-30.,-2.20823322648152,-3.54456693671123));
#31643=CARTESIAN_POINT('Ctrl Pts',(-30.,-2.09330331962513,-3.599117393161));
#31644=CARTESIAN_POINT('Ctrl Pts',(-30.,-1.97613528593933,-3.64830883882638));
#31645=CARTESIAN_POINT('Ctrl Pts',(-30.,-1.85480069740671,-3.69924955730885));
#31646=CARTESIAN_POINT('Ctrl Pts',(-30.,-1.73106514290719,-3.74444397765563));
#31647=CARTESIAN_POINT('Ctrl Pts',(-30.,-1.60530493978341,-3.7836051080115));
#31648=CARTESIAN_POINT('Ctrl Pts',(-30.,-1.48790451895484,-3.82016304183877));
#31649=CARTESIAN_POINT('Ctrl Pts',(-30.,-1.36873904140857,-3.8514627731731));
#31650=CARTESIAN_POINT('Ctrl Pts',(-30.,-1.24812048797374,-3.87721988828248));
#31651=CARTESIAN_POINT('Ctrl Pts',(-30.,-1.23953155072496,-3.87905398626397));
#31652=CARTESIAN_POINT('Ctrl Pts',(-30.,-1.23093525049353,-3.88085995890718));
#31653=CARTESIAN_POINT('Ctrl Pts',(-30.,-1.22233170237264,-3.88263769354994));
#31654=CARTESIAN_POINT('Ctrl Pts',(-31.3088415259036,-4.9251906134473,-0.000109311167407344));
#31655=CARTESIAN_POINT('Ctrl Pts',(-31.3026574105697,-4.92531380403982,
-0.127669621032252));
#31656=CARTESIAN_POINT('Ctrl Pts',(-31.2964732952358,-4.92045776407975,
-0.255220574660955));
#31657=CARTESIAN_POINT('Ctrl Pts',(-31.2902891799019,-4.91055613124801,
-0.382378634225134));
#31658=CARTESIAN_POINT('Ctrl Pts',(-31.2506528469036,-4.84709282324748,
-1.19738270840192));
#31659=CARTESIAN_POINT('Ctrl Pts',(-31.2110165139052,-4.57635592020155,
-1.99624664458159));
#31660=CARTESIAN_POINT('Ctrl Pts',(-31.1713801809069,-4.1312401814026,-2.681907808277));
#31661=CARTESIAN_POINT('Ctrl Pts',(-31.1317438479086,-3.68612444260365,
-3.36756897197242));
#31662=CARTESIAN_POINT('Ctrl Pts',(-31.0921075149103,-3.06662986805169,
-3.94002736318355));
#31663=CARTESIAN_POINT('Ctrl Pts',(-31.052471181912,-2.3480256147852,-4.32972871815496));
#31664=CARTESIAN_POINT('Ctrl Pts',(-31.0128348489136,-1.6294213615187,-4.71943007312636));
#31665=CARTESIAN_POINT('Ctrl Pts',(-30.9731985159153,-0.811707429537671,
-4.92637439185802));
#31666=CARTESIAN_POINT('Ctrl Pts',(-30.933562182917,0.00576326833122948,
-4.92541789298911));
#31667=CARTESIAN_POINT('Ctrl Pts',(-30.8939258499187,0.823233966200106,
-4.9244613941202));
#31668=CARTESIAN_POINT('Ctrl Pts',(-30.8542895169204,1.64046142995691,-4.71560407765069));
#31669=CARTESIAN_POINT('Ctrl Pts',(-30.814653183922,2.35815171375025,-4.32422202182277));
#31670=CARTESIAN_POINT('Ctrl Pts',(-30.7750168509237,3.07584199754363,-3.93283996599483));
#31671=CARTESIAN_POINT('Ctrl Pts',(-30.7353805179254,3.69399510137354,-3.35893317080848));
#31672=CARTESIAN_POINT('Ctrl Pts',(-30.6957441849271,4.13750506653447,-2.6722323509177));
#31673=CARTESIAN_POINT('Ctrl Pts',(-30.6561078519288,4.58101503169538,-1.98553153102693));
#31674=CARTESIAN_POINT('Ctrl Pts',(-30.6164715189305,4.84988185818724,-1.1860366864318));
#31675=CARTESIAN_POINT('Ctrl Pts',(-30.5768351859321,4.91143762165332,-0.370886072034668));
#31676=CARTESIAN_POINT('Ctrl Pts',(-30.5371988529338,4.97299338511941,0.444264542362484));
#31677=CARTESIAN_POINT('Ctrl Pts',(-30.4975625199355,4.82723808555968,1.27507092656169));
#31678=CARTESIAN_POINT('Ctrl Pts',(-30.4579261869371,4.49188185629875,2.02058724364277));
#31679=CARTESIAN_POINT('Ctrl Pts',(-30.4182898539388,4.15652562703785,2.76610356072381));
#31680=CARTESIAN_POINT('Ctrl Pts',(-30.3786535209405,3.63156846807577,3.42632981068678));
#31681=CARTESIAN_POINT('Ctrl Pts',(-30.3390171879422,2.98079166474727,3.92105218071421));
#31682=CARTESIAN_POINT('Ctrl Pts',(-30.2993808549439,2.33001486141874,4.41577455074166));
#31683=CARTESIAN_POINT('Ctrl Pts',(-30.2597445219456,1.55341841372378,4.74499304083354));
#31684=CARTESIAN_POINT('Ctrl Pts',(-30.2201081889472,0.745362402034862,
4.86869882773104));
#31685=CARTESIAN_POINT('Ctrl Pts',(-30.1804718559489,-0.0626936096540083,
4.99240461462853));
#31686=CARTESIAN_POINT('Ctrl Pts',(-30.1408355229506,-0.902209185336816,
4.91059769833167));
#31687=CARTESIAN_POINT('Ctrl Pts',(-30.1011991899523,-1.6711882943574,4.63323462455056));
#31688=CARTESIAN_POINT('Ctrl Pts',(-30.0674661266349,-2.32563887068767,
4.39718084706891));
#31689=CARTESIAN_POINT('Ctrl Pts',(-30.0337330633174,-2.92899916179811,
4.01948374188552));
#31690=CARTESIAN_POINT('Ctrl Pts',(-30.,-3.42895048616045,3.53554286219762));
#31691=CARTESIAN_POINT('',(-52.575,-2.3624802440062,-3.31498401464311));
#31692=CARTESIAN_POINT('Ctrl Pts',(-52.575,-2.36248024400613,-3.31498401464316));
#31693=CARTESIAN_POINT('Ctrl Pts',(-52.575,-2.45083842515724,-3.26474899095752));
#31694=CARTESIAN_POINT('Ctrl Pts',(-52.575,-2.53718350580222,-3.21123766039523));
#31695=CARTESIAN_POINT('Ctrl Pts',(-52.575,-2.62132193580694,-3.15455696157957));
#31696=CARTESIAN_POINT('Ctrl Pts',(-52.575,-2.72544813390243,-3.08441130194771));
#31697=CARTESIAN_POINT('Ctrl Pts',(-52.575,-2.82619583876697,-3.00941312765807));
#31698=CARTESIAN_POINT('Ctrl Pts',(-52.575,-2.92335409742353,-2.92992007978695));
#31699=CARTESIAN_POINT('Ctrl Pts',(-52.575,-2.97900323996874,-2.884389004884));
#31700=CARTESIAN_POINT('Ctrl Pts',(-52.575,-3.03347452971045,-2.83738238248389));
#31701=CARTESIAN_POINT('Ctrl Pts',(-52.575,-3.08672527840934,-2.78896043733211));
#31702=CARTESIAN_POINT('Ctrl Pts',(-52.575,-3.11397380637268,-2.76418281901225));
#31703=CARTESIAN_POINT('Ctrl Pts',(-52.575,-3.14090270788054,-2.73903453627563));
#31704=CARTESIAN_POINT('Ctrl Pts',(-52.575,-3.16750598016368,-2.71352319283678));
#31705=CARTESIAN_POINT('Ctrl Pts',(-52.575,-3.18459441820031,-2.69713614815498));
#31706=CARTESIAN_POINT('Ctrl Pts',(-52.575,-3.20154849591608,-2.68059929653958));
#31707=CARTESIAN_POINT('Ctrl Pts',(-52.575,-3.21836657574555,-2.66391458876838));
#31708=CARTESIAN_POINT('Ctrl Pts',(-52.575,-3.23304555953287,-2.6493520134118));
#31709=CARTESIAN_POINT('Ctrl Pts',(-52.575,-3.24761411042159,-2.63468357077931));
#31710=CARTESIAN_POINT('Ctrl Pts',(-52.575,-3.26207083882393,-2.61991143683803));
#31711=CARTESIAN_POINT('Ctrl Pts',(-52.575,-3.35252129885386,-2.527487599755));
#31712=CARTESIAN_POINT('Ctrl Pts',(-52.575,-3.43860302817434,-2.43100187945135));
#31713=CARTESIAN_POINT('Ctrl Pts',(-52.575,-3.52009386900591,-2.33082932389395));
#31714=CARTESIAN_POINT('Ctrl Pts',(-52.575,-3.60209138438908,-2.23003393902036));
#31715=CARTESIAN_POINT('Ctrl Pts',(-52.575,-3.67944139370459,-2.12550522054836));
#31716=CARTESIAN_POINT('Ctrl Pts',(-52.575,-3.75189018667931,-2.01758011205502));
#31717=CARTESIAN_POINT('Ctrl Pts',(-52.575,-3.77730845597078,-1.97971516830155));
#31718=CARTESIAN_POINT('Ctrl Pts',(-52.575,-3.80212313369375,-1.94143178856851));
#31719=CARTESIAN_POINT('Ctrl Pts',(-52.575,-3.82632223974423,-1.90274340160315));
#31720=CARTESIAN_POINT('Ctrl Pts',(-52.575,-3.84913245184897,-1.86627551263115));
#31721=CARTESIAN_POINT('Ctrl Pts',(-52.575,-3.87139572307394,-1.82944776587887));
#31722=CARTESIAN_POINT('Ctrl Pts',(-52.575,-3.89310152313127,-1.79227099068793));
#31723=CARTESIAN_POINT('Ctrl Pts',(-52.575,-3.90322370392622,-1.77493414805314));
#31724=CARTESIAN_POINT('Ctrl Pts',(-52.575,-3.91321999890863,-1.75752932486574));
#31725=CARTESIAN_POINT('Ctrl Pts',(-52.575,-3.92308811855202,-1.74006057784368));
#31726=CARTESIAN_POINT('Ctrl Pts',(-52.575,-3.95009373716041,-1.69225467999363));
#31727=CARTESIAN_POINT('Ctrl Pts',(-52.575,-3.97614326297851,-1.643963649635));
#31728=CARTESIAN_POINT('Ctrl Pts',(-52.575,-4.00122119219861,-1.59521504644078));
#31729=CARTESIAN_POINT('Ctrl Pts',(-52.575,-4.06049526868924,-1.47999307539268));
#31730=CARTESIAN_POINT('Ctrl Pts',(-52.575,-4.11434405528511,-1.36221753728262));
#31731=CARTESIAN_POINT('Ctrl Pts',(-52.575,-4.16278066252525,-1.24231802685534));
#31732=CARTESIAN_POINT('Ctrl Pts',(-52.575,-4.21199575328309,-1.12049146583625));
#31733=CARTESIAN_POINT('Ctrl Pts',(-52.575,-4.25562365155741,-0.996471504820113));
#31734=CARTESIAN_POINT('Ctrl Pts',(-52.575,-4.29363801884489,-0.870672911911608));
#31735=CARTESIAN_POINT('Ctrl Pts',(-52.575,-4.32788618697962,-0.757337568764584));
#31736=CARTESIAN_POINT('Ctrl Pts',(-52.575,-4.35757764642574,-0.642557729992402));
#31737=CARTESIAN_POINT('Ctrl Pts',(-52.575,-4.38266242226516,-0.526618827435207));
#31738=CARTESIAN_POINT('Ctrl Pts',(-52.575,-4.40147600414472,-0.43966465051731));
#31739=CARTESIAN_POINT('Ctrl Pts',(-52.575,-4.41769774414857,-0.352058115046802));
#31740=CARTESIAN_POINT('Ctrl Pts',(-52.575,-4.43129495642288,-0.263915699110775));
#31741=CARTESIAN_POINT('Ctrl Pts',(-52.575,-4.43428275677774,-0.244547615690493));
#31742=CARTESIAN_POINT('Ctrl Pts',(-52.575,-4.43714379477229,-0.225153648965712));
#31743=CARTESIAN_POINT('Ctrl Pts',(-52.575,-4.43987765592149,-0.205735021774693));
#31744=CARTESIAN_POINT('Ctrl Pts',(-52.575,-4.44260798913829,-0.186341453502313));
#31745=CARTESIAN_POINT('Ctrl Pts',(-52.575,-4.44521045926173,-0.166930227795076));
#31746=CARTESIAN_POINT('Ctrl Pts',(-52.575,-4.44768395086165,-0.147510951408631));
#31747=CARTESIAN_POINT('Ctrl Pts',(-52.575,-4.46489548234348,-0.0123839564793861));
#31748=CARTESIAN_POINT('Ctrl Pts',(-52.575,-4.47588307079217,0.123253805094162));
#31749=CARTESIAN_POINT('Ctrl Pts',(-52.575,-4.48063897431675,0.258956414548593));
#31750=CARTESIAN_POINT('Ctrl Pts',(-52.575,-4.48385862007716,0.350824201384031));
#31751=CARTESIAN_POINT('Ctrl Pts',(-52.575,-4.48422139979451,0.442722422791573));
#31752=CARTESIAN_POINT('Ctrl Pts',(-52.575,-4.48171295534441,0.534519045515166));
#31753=CARTESIAN_POINT('Ctrl Pts',(-52.575,-4.47802927241361,0.669323566388171));
#31754=CARTESIAN_POINT('Ctrl Pts',(-52.575,-4.46815625725434,0.803908860906131));
#31755=CARTESIAN_POINT('Ctrl Pts',(-52.575,-4.45227140210682,0.937896967744017));
#31756=CARTESIAN_POINT('Ctrl Pts',(-52.575,-4.43625287788906,1.07301256775057));
#31757=CARTESIAN_POINT('Ctrl Pts',(-52.575,-4.41412086946338,1.20752165052657));
#31758=CARTESIAN_POINT('Ctrl Pts',(-52.575,-4.38600460743474,1.3410398419735));
#31759=CARTESIAN_POINT('Ctrl Pts',(-52.575,-4.37816899892792,1.37824949223395));
#31760=CARTESIAN_POINT('Ctrl Pts',(-52.575,-4.36986830738069,1.41538216450086));
#31761=CARTESIAN_POINT('Ctrl Pts',(-52.575,-4.36110461497015,1.45242945648354));
#31762=CARTESIAN_POINT('Ctrl Pts',(-52.575,-4.35581207705533,1.47480292513971));
#31763=CARTESIAN_POINT('Ctrl Pts',(-52.575,-4.35035066978824,1.49714525323282));
#31764=CARTESIAN_POINT('Ctrl Pts',(-52.575,-4.34472079756005,1.51945457780506));
#31765=CARTESIAN_POINT('Ctrl Pts',(-52.575,-4.33978278713431,1.53902228251733));
#31766=CARTESIAN_POINT('Ctrl Pts',(-52.575,-4.33471471620666,1.55856607009609));
#31767=CARTESIAN_POINT('Ctrl Pts',(-52.575,-4.32952186708747,1.57806649096184));
#31768=CARTESIAN_POINT('Ctrl Pts',(-52.575,-4.29379030157313,1.7122472749072));
#31769=CARTESIAN_POINT('Ctrl Pts',(-52.575,-4.25210787632114,1.8445664661999));
#31770=CARTESIAN_POINT('Ctrl Pts',(-52.575,-4.2046945955001,1.97463033236496));
#31771=CARTESIAN_POINT('Ctrl Pts',(-52.575,-4.15669273431461,2.10630878913467));
#31772=CARTESIAN_POINT('Ctrl Pts',(-52.575,-4.10281680514146,2.2356763657865));
#31773=CARTESIAN_POINT('Ctrl Pts',(-52.575,-4.04324167749382,2.36232823147581));
#31774=CARTESIAN_POINT('Ctrl Pts',(-52.575,-3.98430004740198,2.48763333299492));
#31775=CARTESIAN_POINT('Ctrl Pts',(-52.575,-3.91977954437028,2.61028094909734));
#31776=CARTESIAN_POINT('Ctrl Pts',(-52.575,-3.84979995958599,2.72987096421517));
#31777=CARTESIAN_POINT('Ctrl Pts',(-52.575,-3.79916663882266,2.81639962274062));
#31778=CARTESIAN_POINT('Ctrl Pts',(-52.575,-3.74567435543154,2.90132744181084));
#31779=CARTESIAN_POINT('Ctrl Pts',(-52.575,-3.68943437806386,2.98455695852906));
#31780=CARTESIAN_POINT('Ctrl Pts',(-52.575,-3.66455066574735,3.0213823529761));
#31781=CARTESIAN_POINT('Ctrl Pts',(-52.575,-3.63912888080377,3.05787519175057));
#31782=CARTESIAN_POINT('Ctrl Pts',(-52.575,-3.61317791043782,3.09402659330026));
#31783=CARTESIAN_POINT('Ctrl Pts',(-52.575,-3.5984365124608,3.11456232626731));
#31784=CARTESIAN_POINT('Ctrl Pts',(-52.575,-3.58352434957018,3.13498787947549));
#31785=CARTESIAN_POINT('Ctrl Pts',(-52.575,-3.56844298859188,3.15530158081671));
#31786=CARTESIAN_POINT('Ctrl Pts',(-52.575,-3.55715242145521,3.17050930703699));
#31787=CARTESIAN_POINT('Ctrl Pts',(-52.575,-3.54576681267099,3.18565452567972));
#31788=CARTESIAN_POINT('Ctrl Pts',(-52.575,-3.53429612334896,3.20072456181671));
#31789=CARTESIAN_POINT('Ctrl Pts',(-52.575,-3.44911973336135,3.31262814834888));
#31790=CARTESIAN_POINT('Ctrl Pts',(-52.575,-3.35913530229149,3.42055165052906));
#31791=CARTESIAN_POINT('Ctrl Pts',(-52.575,-3.26472470398113,3.5242711902548));
#31792=CARTESIAN_POINT('Ctrl Pts',(-52.575,-3.168304243029,3.63019876627992));
#31793=CARTESIAN_POINT('Ctrl Pts',(-52.575,-3.0672668488026,3.73174212442733));
#31794=CARTESIAN_POINT('Ctrl Pts',(-52.575,-2.9619683093501,3.82864474738118));
#31795=CARTESIAN_POINT('Ctrl Pts',(-52.575,-2.85628308759516,3.92590322075376));
#31796=CARTESIAN_POINT('Ctrl Pts',(-52.575,-2.74630488841782,4.0184874465719));
#31797=CARTESIAN_POINT('Ctrl Pts',(-52.575,-2.63234878081027,4.10611049349789));
#31798=CARTESIAN_POINT('Ctrl Pts',(-52.575,-2.51936354614263,4.1929870175129));
#31799=CARTESIAN_POINT('Ctrl Pts',(-52.575,-2.40246734548989,4.2749871084609));
#31800=CARTESIAN_POINT('Ctrl Pts',(-52.575,-2.28193125768585,4.35179515368219));
#31801=CARTESIAN_POINT('Ctrl Pts',(-52.575,-2.24443605083211,4.3756878616344));
#31802=CARTESIAN_POINT('Ctrl Pts',(-52.575,-2.20658839941422,4.39907786480192));
#31803=CARTESIAN_POINT('Ctrl Pts',(-52.575,-2.16839587231069,4.42195480991676));
#31804=CARTESIAN_POINT('Ctrl Pts',(-52.575,-2.3624802440062,-3.31498401464311));
#31805=CARTESIAN_POINT('Ctrl Pts',(-52.5412669366826,-1.89383403051946,
-3.64828975900151));
#31806=CARTESIAN_POINT('Ctrl Pts',(-52.4678975403668,-0.719464420527365,
-4.15646543436434));
#31807=CARTESIAN_POINT('Ctrl Pts',(-52.3548918110528,1.26526436602798,-4.04962642367063));
#31808=CARTESIAN_POINT('Ctrl Pts',(-52.2359828120578,3.04621665534188,-2.95311079097194));
#31809=CARTESIAN_POINT('Ctrl Pts',(-52.1170738130628,4.08693027247079,-1.13899868529834));
#31810=CARTESIAN_POINT('Ctrl Pts',(-51.9981648140679,4.13451401645655,0.951899429035897));
#31811=CARTESIAN_POINT('Ctrl Pts',(-51.8792558150729,3.17740293277235,2.81148063819688));
#31812=CARTESIAN_POINT('Ctrl Pts',(-51.760346816078,1.44817770563431,3.98786896704909));
#31813=CARTESIAN_POINT('Ctrl Pts',(-51.641437817083,-0.632957411871854,
4.19519722352873));
#31814=CARTESIAN_POINT('Ctrl Pts',(-51.522528818088,-2.56028268385088,3.38308566467023));
#31815=CARTESIAN_POINT('Ctrl Pts',(-51.4094453227024,-3.80151277026337,
1.82894004028097));
#31816=CARTESIAN_POINT('Ctrl Pts',(-51.3359981603151,-4.07013175620066,
0.576320675082573));
#31817=CARTESIAN_POINT('Ctrl Pts',(-51.3021873309261,-4.07067545460402,
-8.70709198036793E-5));
#31818=CARTESIAN_POINT('Origin',(-52.575,-4.52129938221115E-16,0.));
#31819=CARTESIAN_POINT('',(-52.575,-4.925,-6.03138548580072E-16));
#31820=CARTESIAN_POINT('Origin',(-52.575,0.,0.));
#31821=CARTESIAN_POINT('Origin',(-52.575,0.,0.));
#31822=CARTESIAN_POINT('',(-52.575,2.36230756092333,-3.31488661006745));
#31823=CARTESIAN_POINT('Ctrl Pts',(-52.575,2.16858289183278,4.42210503781149));
#31824=CARTESIAN_POINT('Ctrl Pts',(-52.575,2.27324543867332,4.35954461344517));
#31825=CARTESIAN_POINT('Ctrl Pts',(-52.575,2.37542046052859,4.29314920151771));
#31826=CARTESIAN_POINT('Ctrl Pts',(-52.575,2.47486626316976,4.22298837806258));
#31827=CARTESIAN_POINT('Ctrl Pts',(-52.575,2.59306038724079,4.13960027266106));
#31828=CARTESIAN_POINT('Ctrl Pts',(-52.575,2.70740051443753,4.05089352006367));
#31829=CARTESIAN_POINT('Ctrl Pts',(-52.575,2.81758791907416,3.95719317432484));
#31830=CARTESIAN_POINT('Ctrl Pts',(-52.575,2.88224740587185,3.90220852078646));
#31831=CARTESIAN_POINT('Ctrl Pts',(-52.575,2.94547616306427,3.84550366688624));
#31832=CARTESIAN_POINT('Ctrl Pts',(-52.575,3.00720683632612,3.78713970701225));
#31833=CARTESIAN_POINT('Ctrl Pts',(-52.575,3.0504874052719,3.74621960593771));
#31834=CARTESIAN_POINT('Ctrl Pts',(-52.575,3.09303145431524,3.70448387254875));
#31835=CARTESIAN_POINT('Ctrl Pts',(-52.575,3.13481408960903,3.66195279787687));
#31836=CARTESIAN_POINT('Ctrl Pts',(-52.575,3.15648069704987,3.63989808322154));
#31837=CARTESIAN_POINT('Ctrl Pts',(-52.575,3.17794569325268,3.61762601164362));
#31838=CARTESIAN_POINT('Ctrl Pts',(-52.575,3.19918545204692,3.59516093882889));
#31839=CARTESIAN_POINT('Ctrl Pts',(-52.575,3.29689976205027,3.4918095255416));
#31840=CARTESIAN_POINT('Ctrl Pts',(-52.575,3.38992792061982,3.38429932195033));
#31841=CARTESIAN_POINT('Ctrl Pts',(-52.575,3.47798443456353,3.27294401601918));
#31842=CARTESIAN_POINT('Ctrl Pts',(-52.575,3.56533656591254,3.16247946462524));
#31843=CARTESIAN_POINT('Ctrl Pts',(-52.575,3.64779664533402,3.04823040929176));
#31844=CARTESIAN_POINT('Ctrl Pts',(-52.575,3.72504020298562,2.9304807933875));
#31845=CARTESIAN_POINT('Ctrl Pts',(-52.575,3.7786407807849,2.84877239413719));
#31846=CARTESIAN_POINT('Ctrl Pts',(-52.575,3.82972855358387,2.76537793963324));
#31847=CARTESIAN_POINT('Ctrl Pts',(-52.575,3.87818054873119,2.68038844930736));
#31848=CARTESIAN_POINT('Ctrl Pts',(-52.575,3.88822812521621,2.66276402740532));
#31849=CARTESIAN_POINT('Ctrl Pts',(-52.575,3.89816231179414,2.64507100689568));
#31850=CARTESIAN_POINT('Ctrl Pts',(-52.575,3.90798194266676,2.62731018963255));
#31851=CARTESIAN_POINT('Ctrl Pts',(-52.575,3.91756756129971,2.60997263152042));
#31852=CARTESIAN_POINT('Ctrl Pts',(-52.575,3.92703894769771,2.5925796412082));
#31853=CARTESIAN_POINT('Ctrl Pts',(-52.575,3.93639533109687,2.57513219119634));
#31854=CARTESIAN_POINT('Ctrl Pts',(-52.575,3.96367451327325,2.52426294534762));
#31855=CARTESIAN_POINT('Ctrl Pts',(-52.575,3.98997637187834,2.47293052215805));
#31856=CARTESIAN_POINT('Ctrl Pts',(-52.575,4.01528228820605,2.42115597945716));
#31857=CARTESIAN_POINT('Ctrl Pts',(-52.575,4.07614892166724,2.29662612357737));
#31858=CARTESIAN_POINT('Ctrl Pts',(-52.575,4.13125737282119,2.16953962378044));
#31859=CARTESIAN_POINT('Ctrl Pts',(-52.575,4.1805437519518,2.0403132293574));
#31860=CARTESIAN_POINT('Ctrl Pts',(-52.575,4.22997373559905,1.91071031115163));
#31861=CARTESIAN_POINT('Ctrl Pts',(-52.575,4.27354777659503,1.77895418493233));
#31862=CARTESIAN_POINT('Ctrl Pts',(-52.575,4.31115013628448,1.64545567277246));
#31863=CARTESIAN_POINT('Ctrl Pts',(-52.575,4.34817398830438,1.51401101876923));
#31864=CARTESIAN_POINT('Ctrl Pts',(-52.575,4.37940844584972,1.38087641354689));
#31865=CARTESIAN_POINT('Ctrl Pts',(-52.575,4.40469318296196,1.24644656007076));
#31866=CARTESIAN_POINT('Ctrl Pts',(-52.575,4.42089893755181,1.16028639137634));
#31867=CARTESIAN_POINT('Ctrl Pts',(-52.575,4.43465959569322,1.0735942307477));
#31868=CARTESIAN_POINT('Ctrl Pts',(-52.575,4.44592201924774,0.986476727243181));
#31869=CARTESIAN_POINT('Ctrl Pts',(-52.575,4.44839087427289,0.967379551110164));
#31870=CARTESIAN_POINT('Ctrl Pts',(-52.575,4.45073964677597,0.948261947204026));
#31871=CARTESIAN_POINT('Ctrl Pts',(-52.575,4.45296772135315,0.929125059904503));
#31872=CARTESIAN_POINT('Ctrl Pts',(-52.575,4.45503253428023,0.911390423602443));
#31873=CARTESIAN_POINT('Ctrl Pts',(-52.575,4.45699252464179,0.893649215236444));
#31874=CARTESIAN_POINT('Ctrl Pts',(-52.575,4.45884750535299,0.8759027682724));
#31875=CARTESIAN_POINT('Ctrl Pts',(-52.575,4.47288219592637,0.741634044929663));
#31876=CARTESIAN_POINT('Ctrl Pts',(-52.575,4.48091097969341,0.607056985697511));
#31877=CARTESIAN_POINT('Ctrl Pts',(-52.575,4.4828462748776,0.472553339734528));
#31878=CARTESIAN_POINT('Ctrl Pts',(-52.575,4.48415655129386,0.381488701819775));
#31879=CARTESIAN_POINT('Ctrl Pts',(-52.575,4.4826725944393,0.290457608534688));
#31880=CARTESIAN_POINT('Ctrl Pts',(-52.575,4.4783536900286,0.19957981697436));
#31881=CARTESIAN_POINT('Ctrl Pts',(-52.575,4.47194675885048,0.0647660538580273));
#31882=CARTESIAN_POINT('Ctrl Pts',(-52.575,4.45930309571538,-0.0697115117325435));
#31883=CARTESIAN_POINT('Ctrl Pts',(-52.575,4.44051793802534,-0.203434251933974));
#31884=CARTESIAN_POINT('Ctrl Pts',(-52.575,4.42188439250804,-0.336077736080069));
#31885=CARTESIAN_POINT('Ctrl Pts',(-52.575,4.39720771395406,-0.467979255925283));
#31886=CARTESIAN_POINT('Ctrl Pts',(-52.575,4.36653652929021,-0.598704962823127));
#31887=CARTESIAN_POINT('Ctrl Pts',(-52.575,4.35826910408269,-0.633942108578089));
#31888=CARTESIAN_POINT('Ctrl Pts',(-52.575,4.34956590074294,-0.66909364602887));
#31889=CARTESIAN_POINT('Ctrl Pts',(-52.575,4.34042736750284,-0.704150655988287));
#31890=CARTESIAN_POINT('Ctrl Pts',(-52.575,4.33455267477135,-0.726687003582102));
#31891=CARTESIAN_POINT('Ctrl Pts',(-52.575,4.32849807591017,-0.749184283359156));
#31892=CARTESIAN_POINT('Ctrl Pts',(-52.575,4.32226364568102,-0.77164008078128));
#31893=CARTESIAN_POINT('Ctrl Pts',(-52.575,4.31754011549755,-0.788653766558259));
#31894=CARTESIAN_POINT('Ctrl Pts',(-52.575,4.31271343970828,-0.805643132465032));
#31895=CARTESIAN_POINT('Ctrl Pts',(-52.575,4.3077875565571,-0.822594272316468));
#31896=CARTESIAN_POINT('Ctrl Pts',(-52.575,4.27100624199071,-0.949167556334511));
#31897=CARTESIAN_POINT('Ctrl Pts',(-52.575,4.22864619087658,-1.07379868233084));
#31898=CARTESIAN_POINT('Ctrl Pts',(-52.575,4.18082992080759,-1.19610839048349));
#31899=CARTESIAN_POINT('Ctrl Pts',(-52.575,4.1335416210436,-1.31706759819301));
#31900=CARTESIAN_POINT('Ctrl Pts',(-52.575,4.08091651537112,-1.43575703633188));
#31901=CARTESIAN_POINT('Ctrl Pts',(-52.575,4.02302930721789,-1.55178516490185));
#31902=CARTESIAN_POINT('Ctrl Pts',(-52.575,3.96819756105823,-1.66168897778376));
#31903=CARTESIAN_POINT('Ctrl Pts',(-52.575,3.90864399407258,-1.76920531054976));
#31904=CARTESIAN_POINT('Ctrl Pts',(-52.575,3.84439996309285,-1.87397258856179));
#31905=CARTESIAN_POINT('Ctrl Pts',(-52.575,3.79893585979599,-1.9481141123272));
#31906=CARTESIAN_POINT('Ctrl Pts',(-52.575,3.75112194501686,-2.02087824453719));
#31907=CARTESIAN_POINT('Ctrl Pts',(-52.575,3.70103299493048,-2.09216319996224));
#31908=CARTESIAN_POINT('Ctrl Pts',(-52.575,3.67453230440468,-2.1298781159189));
#31909=CARTESIAN_POINT('Ctrl Pts',(-52.575,3.6473947043283,-2.16717883751779));
#31910=CARTESIAN_POINT('Ctrl Pts',(-52.575,3.61963075641688,-2.20404924569613));
#31911=CARTESIAN_POINT('Ctrl Pts',(-52.575,3.60474852672729,-2.22381278526946));
#31912=CARTESIAN_POINT('Ctrl Pts',(-52.575,3.58968632609275,-2.2434526722059));
#31913=CARTESIAN_POINT('Ctrl Pts',(-52.575,3.57444574627334,-2.26296633271248));
#31914=CARTESIAN_POINT('Ctrl Pts',(-52.575,3.56382195463694,-2.27656877210399));
#31915=CARTESIAN_POINT('Ctrl Pts',(-52.575,3.55311463654801,-2.29010579189593));
#31916=CARTESIAN_POINT('Ctrl Pts',(-52.575,3.54232924135416,-2.30357081513136));
#31917=CARTESIAN_POINT('Ctrl Pts',(-52.575,3.46063398202519,-2.4055632359298));
#31918=CARTESIAN_POINT('Ctrl Pts',(-52.575,3.3743805109152,-2.50353323130147));
#31919=CARTESIAN_POINT('Ctrl Pts',(-52.575,3.28388534939653,-2.59720213470236));
#31920=CARTESIAN_POINT('Ctrl Pts',(-52.575,3.19548588962452,-2.68870183832316));
#31921=CARTESIAN_POINT('Ctrl Pts',(-52.575,3.10303810752968,-2.77609769489524));
#31922=CARTESIAN_POINT('Ctrl Pts',(-52.575,3.00680571587098,-2.85908844917917));
#31923=CARTESIAN_POINT('Ctrl Pts',(-52.575,2.90715122652406,-2.94503041836574));
#31924=CARTESIAN_POINT('Ctrl Pts',(-52.575,2.80343757806056,-3.02624927085457));
#31925=CARTESIAN_POINT('Ctrl Pts',(-52.575,2.6959339822994,-3.10235576984184));
#31926=CARTESIAN_POINT('Ctrl Pts',(-52.575,2.59557664254627,-3.17340312153467));
#31927=CARTESIAN_POINT('Ctrl Pts',(-52.575,2.49191576181343,-3.2399950596289));
#31928=CARTESIAN_POINT('Ctrl Pts',(-52.575,2.38516016083428,-3.30176468148191));
#31929=CARTESIAN_POINT('Ctrl Pts',(-52.575,2.37755829676769,-3.30616317921379));
#31930=CARTESIAN_POINT('Ctrl Pts',(-52.575,2.36994073858172,-3.31053720298181));
#31931=CARTESIAN_POINT('Ctrl Pts',(-52.575,2.36230756092339,-3.31488661006741));
#31932=CARTESIAN_POINT('Origin',(-52.575,0.,0.));
#31933=CARTESIAN_POINT('Origin',(-55.3478126690739,0.,0.));
#31934=CARTESIAN_POINT('Ctrl Pts',(-52.575,2.36230756092333,-3.31488661006745));
#31935=CARTESIAN_POINT('Ctrl Pts',(-52.5353636670017,2.91267249451488,-2.92267674082431));
#31936=CARTESIAN_POINT('Ctrl Pts',(-52.456091001005,3.81372197207604,-1.85922435845946));
#31937=CARTESIAN_POINT('Ctrl Pts',(-52.3371820020101,4.2384739899776,0.188973964574656));
#31938=CARTESIAN_POINT('Ctrl Pts',(-52.2182730030151,3.63326518569111,2.1907646706185));
#31939=CARTESIAN_POINT('Ctrl Pts',(-52.0993640040202,2.14517071451495,3.66043213853357));
#31940=CARTESIAN_POINT('Ctrl Pts',(-51.9804550050252,0.135793741969793,
4.240490317549));
#31941=CARTESIAN_POINT('Ctrl Pts',(-51.8615460060302,-1.90658020276247,
3.79016093772832));
#31942=CARTESIAN_POINT('Ctrl Pts',(-51.7426370070353,-3.48565239142985,
2.41878623204276));
#31943=CARTESIAN_POINT('Ctrl Pts',(-51.6547258947165,-4.02686902757588,
0.970374196809295));
#31944=CARTESIAN_POINT('Ctrl Pts',(-51.606451115396,-4.07067915096537,0.147388340486156));
#31945=CARTESIAN_POINT('Ctrl Pts',(-51.5978126690739,-4.07052776695671,
0.00010449757507032));
#31946=CARTESIAN_POINT('Ctrl Pts',(-53.0683458050225,2.85821514250023,-4.01076441581681));
#31947=CARTESIAN_POINT('Ctrl Pts',(-53.0287094720242,3.52411547364834,-3.53621986207098));
#31948=CARTESIAN_POINT('Ctrl Pts',(-52.9494368060276,4.6143178264278,-2.24952216322641));
#31949=CARTESIAN_POINT('Ctrl Pts',(-52.8305278070326,5.12823594168768,0.228644337435172));
#31950=CARTESIAN_POINT('Ctrl Pts',(-52.7116188080377,4.3959786364154,2.65066109883206));
#31951=CARTESIAN_POINT('Ctrl Pts',(-52.5927098090426,2.59549582827328,4.42884861375204));
#31952=CARTESIAN_POINT('Ctrl Pts',(-52.4738008100477,0.16430025284401,5.13067554696692));
#31953=CARTESIAN_POINT('Ctrl Pts',(-52.3548918110528,-2.30681918648935,
4.58581074028058));
#31954=CARTESIAN_POINT('Ctrl Pts',(-52.2359828120578,-4.21737821589285,
2.92655010264362));
#31955=CARTESIAN_POINT('Ctrl Pts',(-52.1170738130628,-5.1031065981609,0.556150593197082));
#31956=CARTESIAN_POINT('Ctrl Pts',(-51.9981648140679,-4.74877130744063,
-1.94940347214282));
#31957=CARTESIAN_POINT('Ctrl Pts',(-51.8792558150729,-3.24047617807803,
-3.9812445731161));
#31958=CARTESIAN_POINT('Ctrl Pts',(-51.760346816078,-0.944739701634101,
-5.04563852186393));
#31959=CARTESIAN_POINT('Ctrl Pts',(-51.641437817083,1.58057020018507,-4.88393233495926));
#31960=CARTESIAN_POINT('Ctrl Pts',(-51.522528818088,3.72179876201096,-3.53542259729576));
#31961=CARTESIAN_POINT('Ctrl Pts',(-51.4036198190931,4.95862370685834,-1.32779868772642));
#31962=CARTESIAN_POINT('Ctrl Pts',(-51.2847108200981,4.99049439700665,1.20248248786643));
#31963=CARTESIAN_POINT('Ctrl Pts',(-51.1658018211031,3.80966620304533,3.44055838262431));
#31964=CARTESIAN_POINT('Ctrl Pts',(-51.0468928221082,1.70308244370534,4.8425725242518));
#31965=CARTESIAN_POINT('Ctrl Pts',(-50.9279838231132,-0.817353334162299,
5.06783307265007));
#31966=CARTESIAN_POINT('Ctrl Pts',(-50.8090748241183,-3.13917081939765,
4.06160129283451));
#31967=CARTESIAN_POINT('Ctrl Pts',(-50.6901658251233,-4.69816429329073,
2.06839328444175));
#31968=CARTESIAN_POINT('Ctrl Pts',(-50.5712568261283,-5.11549560931122,
-0.427437919675575));
#31969=CARTESIAN_POINT('Ctrl Pts',(-50.4523478271334,-4.28975252612823,
-2.81940095899504));
#31970=CARTESIAN_POINT('Ctrl Pts',(-50.3334388281384,-2.42159206029875,
-4.52624462417659));
#31971=CARTESIAN_POINT('Ctrl Pts',(-50.2145298291435,0.0350195206030677,
-5.1332029120825));
#31972=CARTESIAN_POINT('Ctrl Pts',(-50.0956208301484,2.48312129661556,-4.49278389533952));
#31973=CARTESIAN_POINT('Ctrl Pts',(-49.9767118311536,4.32782024529306,-2.76061051728878));
#31974=CARTESIAN_POINT('Ctrl Pts',(-49.8578028321585,5.12085128883261,-0.357603944948157));
#31975=CARTESIAN_POINT('Ctrl Pts',(-49.7388938331636,4.6695064936802,2.13230101281847));
#31976=CARTESIAN_POINT('Ctrl Pts',(-49.6199848341686,3.08346343614612,4.10405308709817));
#31977=CARTESIAN_POINT('Ctrl Pts',(-49.5010758351737,0.748133359127894,
5.07851306789146));
#31978=CARTESIAN_POINT('Ctrl Pts',(-49.3821668361787,-1.76899443543955,
4.81888547188666));
#31979=CARTESIAN_POINT('Ctrl Pts',(-49.2632578371838,-3.85625348161299,
3.38826025997524));
#31980=CARTESIAN_POINT('Ctrl Pts',(-49.1443488381888,-5.00643617275599,
1.13428186615986));
#31981=CARTESIAN_POINT('Ctrl Pts',(-49.0254398391939,-4.94004609895293,
-1.39532900922998));
#31982=CARTESIAN_POINT('Ctrl Pts',(-48.9065308401988,-3.6732161645023,-3.58587248973217));
#31983=CARTESIAN_POINT('Ctrl Pts',(-48.787621841204,-1.51378826389541,-4.90504267013768));
#31984=CARTESIAN_POINT('Ctrl Pts',(-48.6687128422089,1.01349283811091,-5.03227888444955));
#31985=CARTESIAN_POINT('Ctrl Pts',(-48.549803843214,3.29449340406979,-3.93666250957833));
#31986=CARTESIAN_POINT('Ctrl Pts',(-48.430894844219,4.77492629845893,-1.88443024494519));
#31987=CARTESIAN_POINT('Ctrl Pts',(-48.3119858452241,5.09504373313213,0.625721872120406));
#31988=CARTESIAN_POINT('Ctrl Pts',(-48.1930768462291,4.17705661038212,2.98382247753481));
#31989=CARTESIAN_POINT('Ctrl Pts',(-48.0741678472341,2.24403741002721,4.61684899105194));
#31990=CARTESIAN_POINT('Ctrl Pts',(-47.9552588482392,-0.234286814171907,
5.12797310762099));
#31991=CARTESIAN_POINT('Ctrl Pts',(-47.8363498492442,-2.65567893188406,
4.39299077104949));
#31992=CARTESIAN_POINT('Ctrl Pts',(-47.7174408502493,-4.43173641444143,
2.59050397735512));
#31993=CARTESIAN_POINT('Ctrl Pts',(-47.5985318512543,-5.13087418062076,
0.158520176691056));
#31994=CARTESIAN_POINT('Ctrl Pts',(-47.4796228522593,-4.58320052783577,
-2.31198430475313));
#31995=CARTESIAN_POINT('Ctrl Pts',(-47.3607138532644,-2.92180111364115,
-4.22067254784166));
#31996=CARTESIAN_POINT('Ctrl Pts',(-47.2418048542695,-0.55039890768255,
-5.10372996407537));
#31997=CARTESIAN_POINT('Ctrl Pts',(-47.1228958552744,1.95475119754748,-4.74657205354196));
#31998=CARTESIAN_POINT('Ctrl Pts',(-47.0039868562796,3.98489333560856,-3.23598881450499));
#31999=CARTESIAN_POINT('Ctrl Pts',(-46.8850778572845,5.04669940864642,-0.93905462170567));
#32000=CARTESIAN_POINT('Ctrl Pts',(-46.7661688582896,4.88214867984596,1.58607149008397));
#32001=CARTESIAN_POINT('Ctrl Pts',(-46.6472598592946,3.53122726471987,3.72577944981691));
#32002=CARTESIAN_POINT('Ctrl Pts',(-46.5283508602996,1.3222114349539,4.96011647293244));
#32003=CARTESIAN_POINT('Ctrl Pts',(-46.4094418613047,-1.20810409099495,
4.98913649934544));
#32004=CARTESIAN_POINT('Ctrl Pts',(-46.2905328623097,-3.44484820534307,
3.80578761177265));
#32005=CARTESIAN_POINT('Ctrl Pts',(-46.1716238633147,-4.84448816787985,
1.69762566399454));
#32006=CARTESIAN_POINT('Ctrl Pts',(-46.0527148643198,-5.06690901450728,
-0.823062295626789));
#32007=CARTESIAN_POINT('Ctrl Pts',(-45.9338058653248,-4.05806208965098,
-3.14374467479683));
#32008=CARTESIAN_POINT('Ctrl Pts',(-45.8148968663299,-2.0630989642918,-4.70049158783766));
#32009=CARTESIAN_POINT('Ctrl Pts',(-45.6959878673349,0.43320082545685,-5.11501080629941));
#32010=CARTESIAN_POINT('Ctrl Pts',(-45.57707886834,2.82423205533933,-4.2865734335784));
#32011=CARTESIAN_POINT('Ctrl Pts',(-45.458169869345,4.52896994562411,-2.41649120322742));
#32012=CARTESIAN_POINT('Ctrl Pts',(-45.33926087035,5.13316020105655,0.0408026249133683));
#32013=CARTESIAN_POINT('Ctrl Pts',(-45.2203518713551,4.48998353049627,2.48818134382005));
#32014=CARTESIAN_POINT('Ctrl Pts',(-45.1014428723601,2.75573299237594,4.33092763477912));
#32015=CARTESIAN_POINT('Ctrl Pts',(-44.9825338733652,0.351834506810982,
5.12125092005135));
#32016=CARTESIAN_POINT('Ctrl Pts',(-44.8636248743701,-2.13756038013976,
4.66710125446325));
#32017=CARTESIAN_POINT('Ctrl Pts',(-44.7447158753753,-4.10752434901852,
3.07883780599703));
#32018=CARTESIAN_POINT('Ctrl Pts',(-44.6258068763802,-5.07935269991291,
0.742411369974384));
#32019=CARTESIAN_POINT('Ctrl Pts',(-44.5068978773853,-4.81688944547566,
-1.77442232161193));
#32020=CARTESIAN_POINT('Ctrl Pts',(-44.3879888783903,-3.38391360602914,
-3.86006829609525));
#32021=CARTESIAN_POINT('Ctrl Pts',(-44.2690798793954,-1.12864084321015,
-5.00771087473245));
#32022=CARTESIAN_POINT('Ctrl Pts',(-44.1501708804004,1.40089365066207,-4.93847100187184));
#32023=CARTESIAN_POINT('Ctrl Pts',(-44.0312618814055,3.59000847626879,-3.66917388350381));
#32024=CARTESIAN_POINT('Ctrl Pts',(-43.9123528824105,4.90674506105724,-1.50826135214278));
#32025=CARTESIAN_POINT('Ctrl Pts',(-43.7934438834155,5.03113377377479,1.0191618737146));
#32026=CARTESIAN_POINT('Ctrl Pts',(-43.6745348844206,3.93294860418829,3.29892589575286));
#32027=CARTESIAN_POINT('Ctrl Pts',(-43.5556258854256,1.87904914644228,4.77704730235934));
#32028=CARTESIAN_POINT('Ctrl Pts',(-43.4367168864307,-0.631460783603362,
5.09433353275251));
#32029=CARTESIAN_POINT('Ctrl Pts',(-43.3178078874357,-2.98852815585981,
4.1736963834896));
#32030=CARTESIAN_POINT('Ctrl Pts',(-43.1988988884407,-4.61937092551605,
2.23882654156266));
#32031=CARTESIAN_POINT('Ctrl Pts',(-43.0799898894457,-5.12771247664765,
-0.240047840842145));
#32032=CARTESIAN_POINT('Ctrl Pts',(-42.9610808904508,-4.3899829470878,-2.66065848599509));
#32033=CARTESIAN_POINT('Ctrl Pts',(-42.8421718914558,-2.58553566085927,
-4.43458815242399));
#32034=CARTESIAN_POINT('Ctrl Pts',(-42.7232628924609,-0.152687346186725,
-5.13117710407935));
#32035=CARTESIAN_POINT('Ctrl Pts',(-42.6043538934659,2.31704211155937,-4.58033832038339));
#32036=CARTESIAN_POINT('Ctrl Pts',(-42.485444894471,4.22416955122785,-2.91755220346545));
#32037=CARTESIAN_POINT('Ctrl Pts',(-42.366535895476,5.10393188151341,-0.543635036753471));
#32038=CARTESIAN_POINT('Ctrl Pts',(-42.247626896481,4.74519466135189,1.95807585226838));
#32039=CARTESIAN_POINT('Ctrl Pts',(-42.1287178974861,3.22984652054977,3.99255890873504));
#32040=CARTESIAN_POINT('Ctrl Pts',(-42.0098088984911,0.936649650830306,
5.03987138354553));
#32041=CARTESIAN_POINT('Ctrl Pts',(-41.8512635664979,-2.44270025858044,
4.84518225905994));
#32042=CARTESIAN_POINT('Ctrl Pts',(-41.6530819015062,-5.62465355290164,
1.50292499192576));
#32043=CARTESIAN_POINT('Ctrl Pts',(-41.4152639035164,-4.30521954672645,
-3.91925959538388));
#32044=CARTESIAN_POINT('Ctrl Pts',(-41.2170822385247,0.0566412091691752,
-5.42580569594987));
#32045=CARTESIAN_POINT('Ctrl Pts',(-41.0585369065314,3.1476070435387,-4.04600865428477));
#32046=CARTESIAN_POINT('Ctrl Pts',(-40.9396279075364,4.70319485935917,-2.06213319184877));
#32047=CARTESIAN_POINT('Ctrl Pts',(-40.8207189085415,5.11432592288447,0.441139175171419));
#32048=CARTESIAN_POINT('Ctrl Pts',(-40.7018099095466,4.28348608439691,2.82796864711987));
#32049=CARTESIAN_POINT('Ctrl Pts',(-40.5829009105515,2.41133856199462,4.53223626887482));
#32050=CARTESIAN_POINT('Ctrl Pts',(-40.4639919115566,-0.0465612617872453,
5.13283696651402));
#32051=CARTESIAN_POINT('Ctrl Pts',(-40.3450829125616,-2.49325046885601,
4.48731478711524));
#32052=CARTESIAN_POINT('Ctrl Pts',(-40.2261739135667,-4.3340233953047,2.75078315105821));
#32053=CARTESIAN_POINT('Ctrl Pts',(-40.1072649145717,-5.1216471237482,0.346099110980013));
#32054=CARTESIAN_POINT('Ctrl Pts',(-39.9883559155767,-4.66468855239917,
-2.14283431888165));
#32055=CARTESIAN_POINT('Ctrl Pts',(-39.8694469165818,-3.07420903783289,
-4.11098173462434));
#32056=CARTESIAN_POINT('Ctrl Pts',(-39.7505379175868,-0.736688055742687,
-5.08019022758471));
#32057=CARTESIAN_POINT('Ctrl Pts',(-39.6316289185919,1.77984776980155,-4.81488512640624));
#32058=CARTESIAN_POINT('Ctrl Pts',(-39.5127199195969,3.86387829223252,-3.37956375387986));
#32059=CARTESIAN_POINT('Ctrl Pts',(-39.393810920602,5.00897920406026,-1.12299782820232));
#32060=CARTESIAN_POINT('Ctrl Pts',(-39.274901921607,4.93688959696835,1.40645621396351));
#32061=CARTESIAN_POINT('Ctrl Pts',(-39.155992922612,3.66512706095948,3.59414009571131));
#32062=CARTESIAN_POINT('Ctrl Pts',(-39.0370839236171,1.50273227714512,4.90844105091367));
#32063=CARTESIAN_POINT('Ctrl Pts',(-38.9181749246221,-1.024829109976,5.02998252006308));
#32064=CARTESIAN_POINT('Ctrl Pts',(-38.7992659256272,-3.30335521405396,
3.92922927399997));
#32065=CARTESIAN_POINT('Ctrl Pts',(-38.6803569266322,-4.77916021775016,
1.8736665009182));
#32066=CARTESIAN_POINT('Ctrl Pts',(-38.5614479276373,-5.09362090864089,
-0.637200552750805));
#32067=CARTESIAN_POINT('Ctrl Pts',(-38.4425389286422,-4.17032279259777,
-2.99322673680418));
#32068=CARTESIAN_POINT('Ctrl Pts',(-38.3236299296473,-2.23362892764998,
-4.62189358672198));
#32069=CARTESIAN_POINT('Ctrl Pts',(-38.2047209306523,0.24584068126806,-5.12743218946767));
#32070=CARTESIAN_POINT('Ctrl Pts',(-38.0858119316574,2.66557057395082,-4.38699578545469));
#32071=CARTESIAN_POINT('Ctrl Pts',(-37.9669029326624,4.43756214501543,-2.58051171516208));
#32072=CARTESIAN_POINT('Ctrl Pts',(-37.8479939336674,5.13121833701352,-0.146958775709808));
#32073=CARTESIAN_POINT('Ctrl Pts',(-37.7290849346725,4.57797947941461,2.32230540411237));
#32074=CARTESIAN_POINT('Ctrl Pts',(-37.6101759356775,2.91228358433659,4.22724530019794));
#32075=CARTESIAN_POINT('Ctrl Pts',(-37.4912669366826,0.538897673790773,
5.10495717915922));
#32076=CARTESIAN_POINT('Ctrl Pts',(-37.3723579376876,-1.96544131602887,
4.74215551590023));
#32077=CARTESIAN_POINT('Ctrl Pts',(-37.2534489386926,-3.99217462115323,
3.22700175054406));
#32078=CARTESIAN_POINT('Ctrl Pts',(-37.1345399396977,-5.04880249610402,
0.927680903710816));
#32079=CARTESIAN_POINT('Ctrl Pts',(-37.0156309407027,-4.87856251527856,
-1.59706802870025));
#32080=CARTESIAN_POINT('Ctrl Pts',(-36.8967219417078,-3.52282329240276,
-3.73372663089914));
#32081=CARTESIAN_POINT('Ctrl Pts',(-36.7778129427128,-1.31103183489013,
-4.96308311754722));
#32082=CARTESIAN_POINT('Ctrl Pts',(-36.6589039437178,1.21934265639497,-4.98640170765204));
#32083=CARTESIAN_POINT('Ctrl Pts',(-36.5399949447229,3.45341474498895,-3.79801594294593));
#32084=CARTESIAN_POINT('Ctrl Pts',(-36.4210859457279,4.84830099762253,-1.68670564718072));
#32085=CARTESIAN_POINT('Ctrl Pts',(-36.302176946733,5.06504161003687,0.834477077201056));
#32086=CARTESIAN_POINT('Ctrl Pts',(-36.183267947738,4.05096823352596,3.15288040920401));
#32087=CARTESIAN_POINT('Ctrl Pts',(-36.064358948743,2.05250247598596,4.70512827559997));
#32088=CARTESIAN_POINT('Ctrl Pts',(-35.9454499497481,-0.444724980715808,
5.1140217241723));
#32089=CARTESIAN_POINT('Ctrl Pts',(-35.8265409507531,-2.83388348761767,
4.28019893023523));
#32090=CARTESIAN_POINT('Ctrl Pts',(-35.7076319517582,-4.53440333997578,
2.40628029418757));
#32091=CARTESIAN_POINT('Ctrl Pts',(-35.5887229527631,-5.13305523310285,
-0.0523686709243773));
#32092=CARTESIAN_POINT('Ctrl Pts',(-35.4698139537683,-4.48436570768963,
-2.4982919572132));
#32093=CARTESIAN_POINT('Ctrl Pts',(-35.3509049547733,-2.74596745539376,
-4.33712591905021));
#32094=CARTESIAN_POINT('Ctrl Pts',(-35.2319959557783,-0.340294298478209,
-5.12203068071659));
#32095=CARTESIAN_POINT('Ctrl Pts',(-35.1130869567833,2.14807096941398,-4.66227300939571));
#32096=CARTESIAN_POINT('Ctrl Pts',(-34.9941779577884,4.11445122673493,-3.06957482505287));
#32097=CARTESIAN_POINT('Ctrl Pts',(-34.8752689587934,5.08101262440804,-0.730964578064523));
#32098=CARTESIAN_POINT('Ctrl Pts',(-34.7563599597985,4.81287904867072,1.78527134258224));
#32099=CARTESIAN_POINT('Ctrl Pts',(-34.6374509608035,3.37520742839479,3.86768319787021));
#32100=CARTESIAN_POINT('Ctrl Pts',(-34.5185419618086,1.11735448716771,5.01024125704392));
#32101=CARTESIAN_POINT('Ctrl Pts',(-34.3996329628135,-1.41201755286977,
4.93530190912031));
#32102=CARTESIAN_POINT('Ctrl Pts',(-34.2807239638187,-3.59826685266438,
3.66107554699376));
#32103=CARTESIAN_POINT('Ctrl Pts',(-34.1618149648236,-4.91013100044579,
1.49720141004484));
#32104=CARTESIAN_POINT('Ctrl Pts',(-34.0429059658287,-5.02882470895011,
-1.03049529374547));
#32105=CARTESIAN_POINT('Ctrl Pts',(-33.9239969668337,-3.92550519897206,
-3.30777983496817));
#32106=CARTESIAN_POINT('Ctrl Pts',(-33.8050879678388,-1.86828104526512,
-4.78126807862545));
#32107=CARTESIAN_POINT('Ctrl Pts',(-33.6861789688438,0.642938677046443,
-5.0928997988704));
#32108=CARTESIAN_POINT('Ctrl Pts',(-33.5672699698489,2.9979231739338,-4.16694794147646));
#32109=CARTESIAN_POINT('Ctrl Pts',(-33.4483609708539,4.62440708498306,-2.22842043073757));
#32110=CARTESIAN_POINT('Ctrl Pts',(-33.3294519718589,5.12715196901376,0.251617150501759));
#32111=CARTESIAN_POINT('Ctrl Pts',(-33.210542972864,4.38398993802041,2.67051132315832));
#32112=CARTESIAN_POINT('Ctrl Pts',(-33.091633973869,2.57551066811489,4.44046656356744));
#32113=CARTESIAN_POINT('Ctrl Pts',(-32.972724974874,0.141177791647324,5.13138064609063));
#32114=CARTESIAN_POINT('Ctrl Pts',(-32.8538159758791,-2.32746153560409,
4.57536023758993));
#32115=CARTESIAN_POINT('Ctrl Pts',(-32.7349069768842,-4.23052363034337,
2.90751927207641));
#32116=CARTESIAN_POINT('Ctrl Pts',(-32.6159979778891,-5.1055610677782,0.533146027081844));
#32117=CARTESIAN_POINT('Ctrl Pts',(-32.4970889788942,-4.73993821730678,
-1.97078263646032));
#32118=CARTESIAN_POINT('Ctrl Pts',(-32.3781799798992,-3.22250207162541,
-3.99580766607272));
#32119=CARTESIAN_POINT('Ctrl Pts',(-32.2592709809043,-0.921992275415497,
-5.04984442724594));
#32120=CARTESIAN_POINT('Ctrl Pts',(-32.1403619819093,1.60256326187619,-4.87676014550612));
#32121=CARTESIAN_POINT('Ctrl Pts',(-32.0214529829143,3.73769311337828,-3.51861459283342));
#32122=CARTESIAN_POINT('Ctrl Pts',(-31.9025439839194,4.96455699567959,-1.30543954265259));
#32123=CARTESIAN_POINT('Ctrl Pts',(-31.7836349849244,4.98502480941995,1.22495963592593));
#32124=CARTESIAN_POINT('Ctrl Pts',(-31.6647259859295,3.79412289105023,3.45769141320538));
#32125=CARTESIAN_POINT('Ctrl Pts',(-31.5458169869345,1.68124239217829,4.85019824183698));
#32126=CARTESIAN_POINT('Ctrl Pts',(-31.4269079879396,-0.840182819327128,
5.06409814678598));
#32127=CARTESIAN_POINT('Ctrl Pts',(-31.3079989889446,-3.15744240337648,
4.04741382447126));
#32128=CARTESIAN_POINT('Ctrl Pts',(-31.1890899899496,-4.70743740996291,
2.04719985417626));
#32129=CARTESIAN_POINT('Ctrl Pts',(-31.0701809909546,-5.11351795109797,
-0.450485284301895));
#32130=CARTESIAN_POINT('Ctrl Pts',(-30.9512719919597,-4.27700252027738,
-2.83870566914707));
#32131=CARTESIAN_POINT('Ctrl Pts',(-30.8323629929647,-2.40117226505815,
-4.53710769903983));
#32132=CARTESIAN_POINT('Ctrl Pts',(-30.7134539939698,0.0581556084619265,
-5.13300037307933));
#32133=CARTESIAN_POINT('Ctrl Pts',(-30.5945449949748,2.5033345078755,-4.48153349680761));
#32134=CARTESIAN_POINT('Ctrl Pts',(-30.4756359959799,4.34023277605901,-2.7411089157019));
#32135=CARTESIAN_POINT('Ctrl Pts',(-30.3567269969849,5.12237892249915,-0.334464657353477));
#32136=CARTESIAN_POINT('Ctrl Pts',(-30.2378179979899,4.65991389359687,2.15320333710529));
#32137=CARTESIAN_POINT('Ctrl Pts',(-30.118908998995,3.06480657161386,4.11815974006944));
#32138=CARTESIAN_POINT('Ctrl Pts',(-30.0396363329983,1.50529535683796,4.76007633060596));
#32139=CARTESIAN_POINT('Ctrl Pts',(-30.,0.695807839646249,4.87560011181053));
#32140=CARTESIAN_POINT('Ctrl Pts',(-52.9038972033484,2.69291261530793,-3.77880514723369));
#32141=CARTESIAN_POINT('Ctrl Pts',(-52.86426087035,3.32030114727052,-3.33170548832209));
#32142=CARTESIAN_POINT('Ctrl Pts',(-52.7849882043534,4.34745254164389,-2.11942289497076));
#32143=CARTESIAN_POINT('Ctrl Pts',(-52.6660792053584,4.83164862445098,0.215420879815001));
#32144=CARTESIAN_POINT('Ctrl Pts',(-52.5471702063635,4.14174081950731,2.49736228942754));
#32145=CARTESIAN_POINT('Ctrl Pts',(-52.4282612073685,2.4453874570205,4.17270978867922));
#32146=CARTESIAN_POINT('Ctrl Pts',(-52.3093522083736,0.154798082552608,
4.83394713716095));
#32147=CARTESIAN_POINT('Ctrl Pts',(-52.1904432093786,-2.17340619191372,
4.32059413942983));
#32148=CARTESIAN_POINT('Ctrl Pts',(-52.0715342103836,-3.97346960773852,
2.75729547911));
#32149=CARTESIAN_POINT('Ctrl Pts',(-51.9526252113887,-4.80797261588486,
0.523986080040587));
#32150=CARTESIAN_POINT('Ctrl Pts',(-51.8337162123937,-4.47413001592062,
-1.83666132209573));
#32151=CARTESIAN_POINT('Ctrl Pts',(-51.7148072133987,-3.05306589759289,
-3.75099256041035));
#32152=CARTESIAN_POINT('Ctrl Pts',(-51.5958982144038,-0.890101456284074,
-4.75382815861975));
#32153=CARTESIAN_POINT('Ctrl Pts',(-51.4769892154088,1.48915921974122,-4.60147411633167));
#32154=CARTESIAN_POINT('Ctrl Pts',(-51.3580802164139,3.50655158487809,-3.33095433270087));
#32155=CARTESIAN_POINT('Ctrl Pts',(-51.2391712174189,4.67184577403192,-1.25100654027042));
#32156=CARTESIAN_POINT('Ctrl Pts',(-51.1202622184239,4.70187324896995,1.1329378999895));
#32157=CARTESIAN_POINT('Ctrl Pts',(-51.001353219429,3.58933728456801,3.24157651203533));
#32158=CARTESIAN_POINT('Ctrl Pts',(-50.882444220434,1.60458606819627,4.56250631633484));
#32159=CARTESIAN_POINT('Ctrl Pts',(-50.763535221439,-0.770082374836318,
4.77473910577498));
#32160=CARTESIAN_POINT('Ctrl Pts',(-50.6446262224441,-2.95761945119629,
3.826701915188));
#32161=CARTESIAN_POINT('Ctrl Pts',(-50.5257172234491,-4.4264498169038,1.94876945624846));
#32162=CARTESIAN_POINT('Ctrl Pts',(-50.4068082244542,-4.81964511874225,
-0.402717398365085));
#32163=CARTESIAN_POINT('Ctrl Pts',(-50.2878992254592,-4.04165820913488,
-2.65634321825318));
#32164=CARTESIAN_POINT('Ctrl Pts',(-50.1689902264643,-2.28154127075387,
-4.26447298076822));
#32165=CARTESIAN_POINT('Ctrl Pts',(-50.0500812274693,0.0329941953675342,
-4.83632833418913));
#32166=CARTESIAN_POINT('Ctrl Pts',(-49.9311722284743,2.33951201418187,-4.23294742572411));
#32167=CARTESIAN_POINT('Ctrl Pts',(-49.8122632294794,4.07752431300185,-2.600952873497));
#32168=CARTESIAN_POINT('Ctrl Pts',(-49.6933542304844,4.82469105693362,-0.336922214257224));
#32169=CARTESIAN_POINT('Ctrl Pts',(-49.5744452314894,4.39944941761592,2.00898113359999));
#32170=CARTESIAN_POINT('Ctrl Pts',(-49.4555362324945,2.90513385873921,3.86669854476821));
#32171=CARTESIAN_POINT('Ctrl Pts',(-49.3366272334995,0.7048656802531,4.78480143225605));
#32172=CARTESIAN_POINT('Ctrl Pts',(-49.2177182345045,-1.66668609397878,
4.54018918520461));
#32173=CARTESIAN_POINT('Ctrl Pts',(-49.0988092355096,-3.63323022611126,
3.19230300839155));
#32174=CARTESIAN_POINT('Ctrl Pts',(-48.9799002365146,-4.71689304520134,
1.06868160527093));
#32175=CARTESIAN_POINT('Ctrl Pts',(-48.8609912375197,-4.65434258683413,
-1.31463130104814));
#32176=CARTESIAN_POINT('Ctrl Pts',(-48.7420822385247,-3.46077872202735,
-3.3784864970096));
#32177=CARTESIAN_POINT('Ctrl Pts',(-48.6231732395298,-1.4262395619327,-4.6213635525991));
#32178=CARTESIAN_POINT('Ctrl Pts',(-48.5042642405347,0.954878311534569,
-4.74124116487174));
#32179=CARTESIAN_POINT('Ctrl Pts',(-48.3853552415398,3.10395908164831,-3.7089888639313));
#32180=CARTESIAN_POINT('Ctrl Pts',(-48.2664462425448,4.4987723544973,-1.77544576817321));
#32181=CARTESIAN_POINT('Ctrl Pts',(-48.1475372435499,4.80037606003829,0.589533761140604));
#32182=CARTESIAN_POINT('Ctrl Pts',(-48.0286282445549,3.93547996919283,2.81125555319956));
#32183=CARTESIAN_POINT('Ctrl Pts',(-47.90971924556,2.11425534797181,4.34983731843916));
#32184=CARTESIAN_POINT('Ctrl Pts',(-47.790810246565,-0.220737028540126,
4.83140099117685));
#32185=CARTESIAN_POINT('Ctrl Pts',(-47.6719012475701,-2.50208992022283,
4.13892575488286));
#32186=CARTESIAN_POINT('Ctrl Pts',(-47.5529922485751,-4.17543057578559,
2.44068430570367));
#32187=CARTESIAN_POINT('Ctrl Pts',(-47.4340832495801,-4.83413428300043,
0.149352292360577));
#32188=CARTESIAN_POINT('Ctrl Pts',(-47.3151742505852,-4.31813488647971,
-2.17827258980143));
#32189=CARTESIAN_POINT('Ctrl Pts',(-47.1962652515901,-2.75282114398926,
-3.97657341470254));
#32190=CARTESIAN_POINT('Ctrl Pts',(-47.0773562525953,-0.51856703853771,
-4.80855992994323));
#32191=CARTESIAN_POINT('Ctrl Pts',(-46.9584472536002,1.84169976619019,-4.47205795406638));
#32192=CARTESIAN_POINT('Ctrl Pts',(-46.8395382546054,3.75443029971838,-3.04883805700957));
#32193=CARTESIAN_POINT('Ctrl Pts',(-46.7206292556103,4.75482768988579,-0.884745168287887));
#32194=CARTESIAN_POINT('Ctrl Pts',(-46.6017202566154,4.5997936174481,1.49434234705342));
#32195=CARTESIAN_POINT('Ctrl Pts',(-46.4828112576204,3.32700163374164,3.5103020528715));
#32196=CARTESIAN_POINT('Ctrl Pts',(-46.3639022586255,1.24574242167685,4.67325220720515));
#32197=CARTESIAN_POINT('Ctrl Pts',(-46.2449932596305,-1.13823438231442,
4.70059388420562));
#32198=CARTESIAN_POINT('Ctrl Pts',(-46.1260842606356,-3.24561823637756,
3.58568300843865));
#32199=CARTESIAN_POINT('Ctrl Pts',(-46.0071752616406,-4.56431117028574,
1.59944487686198));
#32200=CARTESIAN_POINT('Ctrl Pts',(-45.8882662626456,-4.77386848977654,
-0.775461163199525));
#32201=CARTESIAN_POINT('Ctrl Pts',(-45.7693572636507,-3.82336739891617,
-2.96192878142196));
#32202=CARTESIAN_POINT('Ctrl Pts',(-45.6504482646557,-1.94378132875964,
-4.42864251428049));
#32203=CARTESIAN_POINT('Ctrl Pts',(-45.5315392656608,0.408147011219782,
-4.81918835391478));
#32204=CARTESIAN_POINT('Ctrl Pts',(-45.4126302666657,2.66089491210501,-4.03866297679377));
#32205=CARTESIAN_POINT('Ctrl Pts',(-45.2937212676709,4.26704068548633,-2.27673541756528));
#32206=CARTESIAN_POINT('Ctrl Pts',(-45.1748122686758,4.83628809332033,0.0384428385859125));
#32207=CARTESIAN_POINT('Ctrl Pts',(-45.0559032696809,4.23030901768346,2.34427941770878));
#32208=CARTESIAN_POINT('Ctrl Pts',(-44.936994270686,2.59635743623479,4.08045198916703));
#32209=CARTESIAN_POINT('Ctrl Pts',(-44.818085271691,0.331486446840065,4.82506757580879));
#32210=CARTESIAN_POINT('Ctrl Pts',(-44.699176272696,-2.01393632972831,4.39718328343523));
#32211=CARTESIAN_POINT('Ctrl Pts',(-44.5802672737011,-3.86996904910406,
2.9007757481138));
#32212=CARTESIAN_POINT('Ctrl Pts',(-44.4613582747061,-4.78559250484858,
0.699474617646573));
#32213=CARTESIAN_POINT('Ctrl Pts',(-44.3424492757111,-4.53830859734306,
-1.67180006280874));
#32214=CARTESIAN_POINT('Ctrl Pts',(-44.2235402767162,-3.18820773960938,
-3.63682441392853));
#32215=CARTESIAN_POINT('Ctrl Pts',(-44.1046312777212,-1.06336682625425,
-4.71809402583507));
#32216=CARTESIAN_POINT('Ctrl Pts',(-43.9857222787263,1.31987411600958,-4.65285858420012));
#32217=CARTESIAN_POINT('Ctrl Pts',(-43.8668132797312,3.38238328215905,-3.45697022303314));
#32218=CARTESIAN_POINT('Ctrl Pts',(-43.7479042807364,4.62296748713688,-1.42103229458567));
#32219=CARTESIAN_POINT('Ctrl Pts',(-43.6289952817413,4.74016228073313,0.960219483116374));
#32220=CARTESIAN_POINT('Ctrl Pts',(-43.5100862827464,3.7054897492117,3.10813522381238));
#32221=CARTESIAN_POINT('Ctrl Pts',(-43.3911772837514,1.77037588108625,4.50077069187773));
#32222=CARTESIAN_POINT('Ctrl Pts',(-43.2722682847565,-0.594940767387539,
4.79970693351479));
#32223=CARTESIAN_POINT('Ctrl Pts',(-43.1533592857615,-2.81568908248032,
3.9323140782651));
#32224=CARTESIAN_POINT('Ctrl Pts',(-43.0344502867666,-4.35221339889315,
2.10934584580864));
#32225=CARTESIAN_POINT('Ctrl Pts',(-42.9155412877716,-4.83115543358196,
-0.226164870960634));
#32226=CARTESIAN_POINT('Ctrl Pts',(-42.7966322887766,-4.13609188595165,
-2.50678148590829));
#32227=CARTESIAN_POINT('Ctrl Pts',(-42.6777232897817,-2.43600332771514,
-4.17811738584219));
#32228=CARTESIAN_POINT('Ctrl Pts',(-42.5588142907867,-0.143856798821795,
-4.83441968712938));
#32229=CARTESIAN_POINT('Ctrl Pts',(-42.4399052917917,2.18303788250169,-4.31543821244649));
#32230=CARTESIAN_POINT('Ctrl Pts',(-42.3209962927968,3.97986817176768,-2.74881796604673));
#32231=CARTESIAN_POINT('Ctrl Pts',(-42.2020872938018,4.80875016965195,-0.512194350533092));
#32232=CARTESIAN_POINT('Ctrl Pts',(-42.0831782948068,4.47076022222327,1.84483214223366));
#32233=CARTESIAN_POINT('Ctrl Pts',(-41.9642692958119,3.04305099758463,3.7616525407138));
#32234=CARTESIAN_POINT('Ctrl Pts',(-41.8453602968169,0.882479286929472,
4.74839455801324));
#32235=CARTESIAN_POINT('Ctrl Pts',(-41.6868149648237,-2.30142869371028,
4.564965119272));
#32236=CARTESIAN_POINT('Ctrl Pts',(-41.488633299832,-5.29935633050202,1.41600455838255));
#32237=CARTESIAN_POINT('Ctrl Pts',(-41.2508153018422,-4.0562307072897,-3.69259243299773));
#32238=CARTESIAN_POINT('Ctrl Pts',(-41.0526336368505,0.0533654113191093,
-5.11200867617396));
#32239=CARTESIAN_POINT('Ctrl Pts',(-40.8940883048573,2.96556777323727,-3.81201106409278));
#32240=CARTESIAN_POINT('Ctrl Pts',(-40.7751793058623,4.43118944431198,-1.9428714109733));
#32241=CARTESIAN_POINT('Ctrl Pts',(-40.6562703068673,4.8185430801701,0.415626252993168));
#32242=CARTESIAN_POINT('Ctrl Pts',(-40.5373613078723,4.03575418191859,2.66441540116632));
#32243=CARTESIAN_POINT('Ctrl Pts',(-40.4184523088774,2.27188077510969,4.27011810361233));
#32244=CARTESIAN_POINT('Ctrl Pts',(-40.2995433098825,-0.0438684294219718,
4.83598355278229));
#32245=CARTESIAN_POINT('Ctrl Pts',(-40.1806343108874,-2.34905537405823,
4.22779461888579));
#32246=CARTESIAN_POINT('Ctrl Pts',(-40.0617253118925,-4.08336870892313,
2.59169386492762));
#32247=CARTESIAN_POINT('Ctrl Pts',(-39.9428163128975,-4.82544086538998,
0.326082752920268));
#32248=CARTESIAN_POINT('Ctrl Pts',(-39.8239073139026,-4.39491011801506,
-2.01890525455108));
#32249=CARTESIAN_POINT('Ctrl Pts',(-39.7049983149076,-2.89641468095787,
-3.87322647965064));
#32250=CARTESIAN_POINT('Ctrl Pts',(-39.5860893159127,-0.694082306596669,
-4.78638159479478));
#32251=CARTESIAN_POINT('Ctrl Pts',(-39.4671803169177,1.67691173465467,-4.5364201964222));
#32252=CARTESIAN_POINT('Ctrl Pts',(-39.3482713179228,3.64041406206585,-3.18410945758946));
#32253=CARTESIAN_POINT('Ctrl Pts',(-39.2293623189277,4.71928900237705,-1.05805017038851));
#32254=CARTESIAN_POINT('Ctrl Pts',(-39.1104533199328,4.65136863855145,1.32511497302736));
#32255=CARTESIAN_POINT('Ctrl Pts',(-38.9915443209378,3.45315744514966,3.38627595278169));
#32256=CARTESIAN_POINT('Ctrl Pts',(-38.8726353219429,1.41582298910311,4.62456539081176));
#32257=CARTESIAN_POINT('Ctrl Pts',(-38.7537263229479,-0.965558959419366,
4.73907760883507));
#32258=CARTESIAN_POINT('Ctrl Pts',(-38.634817323953,-3.11230837612443,3.70198552343258));
#32259=CARTESIAN_POINT('Ctrl Pts',(-38.5159083249579,-4.50276140854086,
1.76530453644884));
#32260=CARTESIAN_POINT('Ctrl Pts',(-38.3969993259631,-4.79903552343387,
-0.600348581696643));
#32261=CARTESIAN_POINT('Ctrl Pts',(-38.278090326968,-3.92913559623399,-2.82011592485163));
#32262=CARTESIAN_POINT('Ctrl Pts',(-38.1591813279731,-2.10444883163121,
-4.35459016405844));
#32263=CARTESIAN_POINT('Ctrl Pts',(-38.0402723289782,0.231622687214369,
-4.83089135658103));
#32264=CARTESIAN_POINT('Ctrl Pts',(-37.9213633299832,2.51140948728817,-4.1332774843602));
#32265=CARTESIAN_POINT('Ctrl Pts',(-37.8024543309883,4.18091938001268,-2.43126993779448));
#32266=CARTESIAN_POINT('Ctrl Pts',(-37.6835453319933,4.83445853539064,-0.138459535517298));
#32267=CARTESIAN_POINT('Ctrl Pts',(-37.5646363329983,4.31321579310937,2.18799677684917));
#32268=CARTESIAN_POINT('Ctrl Pts',(-37.4457273340034,2.74385405318153,3.98276603732017));
#32269=CARTESIAN_POINT('Ctrl Pts',(-37.3268183350084,0.507730969069655,
4.80971617004981));
#32270=CARTESIAN_POINT('Ctrl Pts',(-37.2079093360135,-1.85177163044197,
4.46789684325476));
#32271=CARTESIAN_POINT('Ctrl Pts',(-37.0890003370184,-3.76129047808892,
3.04037075251765));
#32272=CARTESIAN_POINT('Ctrl Pts',(-36.9700913380235,-4.75680914700616,
0.874029239939502));
#32273=CARTESIAN_POINT('Ctrl Pts',(-36.8511823390286,-4.59641485576549,
-1.50470290988306));
#32274=CARTESIAN_POINT('Ctrl Pts',(-36.7322733400336,-3.31908369826683,
-3.51778961525764));
#32275=CARTESIAN_POINT('Ctrl Pts',(-36.6133643410386,-1.2352093846083,-4.67604727836319));
#32276=CARTESIAN_POINT('Ctrl Pts',(-36.4944553420437,1.14882297450738,-4.69801725694553));
#32277=CARTESIAN_POINT('Ctrl Pts',(-36.3755463430487,3.25368933723309,-3.57836080770076));
#32278=CARTESIAN_POINT('Ctrl Pts',(-36.2566373440537,4.56790348814921,-1.58915641025914));
#32279=CARTESIAN_POINT('Ctrl Pts',(-36.1377283450588,4.77210908511122,0.786215780248905));
#32280=CARTESIAN_POINT('Ctrl Pts',(-36.0188193460638,3.81668381013861,2.97053615812688));
#32281=CARTESIAN_POINT('Ctrl Pts',(-35.8999103470689,1.93379767965904,4.43301104301114));
#32282=CARTESIAN_POINT('Ctrl Pts',(-35.7810013480739,-0.419004676416563,
4.8182564745408));
#32283=CARTESIAN_POINT('Ctrl Pts',(-35.6620923490789,-2.66998816171791,
4.03265713762026));
#32284=CARTESIAN_POINT('Ctrl Pts',(-35.543183350084,-4.27215984393455,2.26711504807025));
#32285=CARTESIAN_POINT('Ctrl Pts',(-35.424274351089,-4.83618919610208,-0.049339971817471));
#32286=CARTESIAN_POINT('Ctrl Pts',(-35.3053653520941,-4.22501609704862,
-2.35380529207354));
#32287=CARTESIAN_POINT('Ctrl Pts',(-35.1864563530991,-2.58715668106996,
-4.08629180075389));
#32288=CARTESIAN_POINT('Ctrl Pts',(-35.0675473541041,-0.32061365698583,
-4.82580223965586));
#32289=CARTESIAN_POINT('Ctrl Pts',(-34.9486383551092,2.0238390476973,-4.39263427595891));
#32290=CARTESIAN_POINT('Ctrl Pts',(-34.8297293561142,3.87649531653223,-2.89204848407095));
#32291=CARTESIAN_POINT('Ctrl Pts',(-34.7108203571192,4.78715642897274,-0.688689841553088));
#32292=CARTESIAN_POINT('Ctrl Pts',(-34.5919113581243,4.53453013854623,1.6820216395544));
#32293=CARTESIAN_POINT('Ctrl Pts',(-34.4730023591293,3.18000507661384,3.64399891410845));
#32294=CARTESIAN_POINT('Ctrl Pts',(-34.3540933601343,1.05273320735146,4.7204780655621));
#32295=CARTESIAN_POINT('Ctrl Pts',(-34.2351843611394,-1.33035467646186,
4.64987277332718));
#32296=CARTESIAN_POINT('Ctrl Pts',(-34.1162753621445,-3.39016404213297,
3.4493402471693));
#32297=CARTESIAN_POINT('Ctrl Pts',(-33.9973663631495,-4.62615760349954,
1.4106119951627));
#32298=CARTESIAN_POINT('Ctrl Pts',(-33.8784573641545,-4.73798675877766,
-0.970897444100449));
#32299=CARTESIAN_POINT('Ctrl Pts',(-33.7595483651595,-3.69847682722778,
-3.11647710271909));
#32300=CARTESIAN_POINT('Ctrl Pts',(-33.6406393661646,-1.76023054420391,
-4.50474736301224));
#32301=CARTESIAN_POINT('Ctrl Pts',(-33.5217303671696,0.605754846282592,
-4.79835611845518));
#32302=CARTESIAN_POINT('Ctrl Pts',(-33.4028213681747,2.82454074739396,-3.92595592685773));
#32303=CARTESIAN_POINT('Ctrl Pts',(-33.2839123691797,4.35695829621027,-2.09954156386342));
#32304=CARTESIAN_POINT('Ctrl Pts',(-33.1650033701848,4.83062734244711,0.237065079090355));
#32305=CARTESIAN_POINT('Ctrl Pts',(-33.0460943711897,4.13044547764555,2.51606449231984));
#32306=CARTESIAN_POINT('Ctrl Pts',(-32.9271853721949,2.42655812219919,4.18365582390123));
#32307=CARTESIAN_POINT('Ctrl Pts',(-32.8082763731998,0.133012889923945,
4.83461145745548));
#32308=CARTESIAN_POINT('Ctrl Pts',(-32.6893673742049,-2.19285470770741,
4.31074803298615));
#32309=CARTESIAN_POINT('Ctrl Pts',(-32.5704583752099,-3.98585476793198,
2.73936528101113));
#32310=CARTESIAN_POINT('Ctrl Pts',(-32.451549376215,-4.81028513326609,0.502311964128084));
#32311=CARTESIAN_POINT('Ctrl Pts',(-32.33264037722,-4.46580778030585,-1.85680403998959));
#32312=CARTESIAN_POINT('Ctrl Pts',(-32.2137313782251,-3.03613130883664,
-3.76471340883693));
#32313=CARTESIAN_POINT('Ctrl Pts',(-32.0948223792301,-0.868669608793307,
-4.75779081891554));
#32314=CARTESIAN_POINT('Ctrl Pts',(-31.9759133802352,1.50988033075788,-4.59471672456974));
#32315=CARTESIAN_POINT('Ctrl Pts',(-31.8570043812401,3.52152669947767,-3.31511840538324));
#32316=CARTESIAN_POINT('Ctrl Pts',(-31.7380953822452,4.6774359159633,-1.22994051800305));
#32317=CARTESIAN_POINT('Ctrl Pts',(-31.6191863832502,4.69671999049274,1.1541151006367));
#32318=CARTESIAN_POINT('Ctrl Pts',(-31.5002773842553,3.57469290726663,3.25771866785284));
#32319=CARTESIAN_POINT('Ctrl Pts',(-31.3813683852603,1.5840091181264,4.56969100680148));
#32320=CARTESIAN_POINT('Ctrl Pts',(-31.2624593862654,-0.791591535461496,
4.77122018628319));
#32321=CARTESIAN_POINT('Ctrl Pts',(-31.1435503872704,-2.97483431311015,
3.81333496741468));
#32322=CARTESIAN_POINT('Ctrl Pts',(-31.0246413882754,-4.43518663048317,
1.92880173063014));
#32323=CARTESIAN_POINT('Ctrl Pts',(-30.9057323892805,-4.81778183676882,
-0.424431837571901));
#32324=CARTESIAN_POINT('Ctrl Pts',(-30.7868233902855,-4.02964558940921,
-2.67453145633584));
#32325=CARTESIAN_POINT('Ctrl Pts',(-30.6679143912906,-2.26230243761365,
-4.27470779861144));
#32326=CARTESIAN_POINT('Ctrl Pts',(-30.5490053922956,0.0547922265715433,
-4.836137508863));
#32327=CARTESIAN_POINT('Ctrl Pts',(-30.4300963933006,2.35855621095642,-4.22234768475872));
#32328=CARTESIAN_POINT('Ctrl Pts',(-30.3111873943057,4.0892189752372,-2.58257913103404));
#32329=CARTESIAN_POINT('Ctrl Pts',(-30.1922783953107,4.8261303411607,-0.31512116837149));
#32330=CARTESIAN_POINT('Ctrl Pts',(-30.0733693963157,4.39041159768631,2.02867458911503));
#32331=CARTESIAN_POINT('Ctrl Pts',(-29.9544603973208,2.88755599865654,3.8799893510414));
#32332=CARTESIAN_POINT('Ctrl Pts',(-29.8751877313241,1.41823783518528,4.48478122234858));
#32333=CARTESIAN_POINT('Ctrl Pts',(-29.8355513983258,0.655566364250106,
4.59362378047096));
#32334=CARTESIAN_POINT('Ctrl Pts',(-52.7394486016742,2.52761008811563,-3.54684587865057));
#32335=CARTESIAN_POINT('Ctrl Pts',(-52.6998122686759,3.1164868208927,-3.1271911145732));
#32336=CARTESIAN_POINT('Ctrl Pts',(-52.6205396026793,4.08058725685996,-1.98932362671511));
#32337=CARTESIAN_POINT('Ctrl Pts',(-52.5016306036842,4.53506130721429,0.202197422194829));
#32338=CARTESIAN_POINT('Ctrl Pts',(-52.3827216046893,3.88750300259921,2.34406348002302));
#32339=CARTESIAN_POINT('Ctrl Pts',(-52.2638126056943,2.29527908576773,3.9165709636064));
#32340=CARTESIAN_POINT('Ctrl Pts',(-52.1449036066994,0.145295912261199,
4.53721872735497));
#32341=CARTESIAN_POINT('Ctrl Pts',(-52.0259946077044,-2.03999319733809,
4.05537753857908));
#32342=CARTESIAN_POINT('Ctrl Pts',(-51.9070856087095,-3.72956099958419,
2.58804085557638));
#32343=CARTESIAN_POINT('Ctrl Pts',(-51.7881766097145,-4.51283863360882,
0.491821566884094));
#32344=CARTESIAN_POINT('Ctrl Pts',(-51.6692676107196,-4.19948872440061,
-1.72391917204864));
#32345=CARTESIAN_POINT('Ctrl Pts',(-51.5503586117245,-2.86565561710775,
-3.52074054770459));
#32346=CARTESIAN_POINT('Ctrl Pts',(-51.4314496127296,-0.835463210934045,
-4.46201779537558));
#32347=CARTESIAN_POINT('Ctrl Pts',(-51.3125406137346,1.39774823929737,-4.31901589770407));
#32348=CARTESIAN_POINT('Ctrl Pts',(-51.1936316147397,3.29130440774522,-3.12648606810599));
#32349=CARTESIAN_POINT('Ctrl Pts',(-51.0747226157447,4.38506784120549,-1.17421439281441));
#32350=CARTESIAN_POINT('Ctrl Pts',(-50.9558136167497,4.41325210093325,1.06339331211258));
#32351=CARTESIAN_POINT('Ctrl Pts',(-50.8369046177548,3.36900836609068,3.04259464144634));
#32352=CARTESIAN_POINT('Ctrl Pts',(-50.7179956187598,1.50608969268721,4.28244010841788));
#32353=CARTESIAN_POINT('Ctrl Pts',(-50.5990866197649,-0.722811415510337,
4.48164513889988));
#32354=CARTESIAN_POINT('Ctrl Pts',(-50.4801776207699,-2.77606808299493,
3.59180253754148));
#32355=CARTESIAN_POINT('Ctrl Pts',(-50.361268621775,-4.15473534051688,1.82914562805518));
#32356=CARTESIAN_POINT('Ctrl Pts',(-50.24235962278,-4.52379462817329,-0.377996877054597));
#32357=CARTESIAN_POINT('Ctrl Pts',(-50.123450623785,-3.79356389214153,-2.49328547751131));
#32358=CARTESIAN_POINT('Ctrl Pts',(-50.0045416247901,-2.14149048120899,
-4.00270133735984));
#32359=CARTESIAN_POINT('Ctrl Pts',(-49.8856326257951,0.0309688701320005,
-4.53945375629576));
#32360=CARTESIAN_POINT('Ctrl Pts',(-49.7667236268001,2.19590273174818,-3.97311095610869));
#32361=CARTESIAN_POINT('Ctrl Pts',(-49.6478146278052,3.82722838071063,-2.44129522970522));
#32362=CARTESIAN_POINT('Ctrl Pts',(-49.5289056288102,4.52853082503464,-0.316240483566295));
#32363=CARTESIAN_POINT('Ctrl Pts',(-49.4099966298152,4.12939234155163,1.88566125438151));
#32364=CARTESIAN_POINT('Ctrl Pts',(-49.2910876308203,2.7268042813323,3.62934400243824));
#32365=CARTESIAN_POINT('Ctrl Pts',(-49.1721786318253,0.661598001378305,
4.49108979662063));
#32366=CARTESIAN_POINT('Ctrl Pts',(-49.0532696328304,-1.56437775251801,
4.26149289852256));
#32367=CARTESIAN_POINT('Ctrl Pts',(-48.9343606338354,-3.41020697060952,
2.99634575680785));
#32368=CARTESIAN_POINT('Ctrl Pts',(-48.8154516348404,-4.42734991764669,
1.00308134438201));
#32369=CARTESIAN_POINT('Ctrl Pts',(-48.6965426358456,-4.36863907471532,
-1.23393359286629));
#32370=CARTESIAN_POINT('Ctrl Pts',(-48.5776336368505,-3.24834127955239,
-3.17110050428704));
#32371=CARTESIAN_POINT('Ctrl Pts',(-48.4587246378556,-1.33869085997,-4.33768443506052));
#32372=CARTESIAN_POINT('Ctrl Pts',(-48.3398156388605,0.896263784958227,
-4.45020344529392));
#32373=CARTESIAN_POINT('Ctrl Pts',(-48.2209066398657,2.91342475922682,-3.48131521828427));
#32374=CARTESIAN_POINT('Ctrl Pts',(-48.1019976408706,4.22261841053568,-1.66646129140123));
#32375=CARTESIAN_POINT('Ctrl Pts',(-47.9830886418758,4.50570838694445,0.5533456501608));
#32376=CARTESIAN_POINT('Ctrl Pts',(-47.8641796428807,3.69390332800355,2.63868862886432));
#32377=CARTESIAN_POINT('Ctrl Pts',(-47.7452706438858,1.98447328591641,4.08282564582639));
#32378=CARTESIAN_POINT('Ctrl Pts',(-47.6263616448909,-0.207187242908341,
4.53482887473271));
#32379=CARTESIAN_POINT('Ctrl Pts',(-47.5074526458958,-2.3485009085616,3.88486073871624));
#32380=CARTESIAN_POINT('Ctrl Pts',(-47.3885436469009,-3.91912473712975,
2.29086463405221));
#32381=CARTESIAN_POINT('Ctrl Pts',(-47.269634647906,-4.53739438538009,0.140184408030102));
#32382=CARTESIAN_POINT('Ctrl Pts',(-47.150725648911,-4.05306924512365,-2.04456087484974));
#32383=CARTESIAN_POINT('Ctrl Pts',(-47.031816649916,-2.58384117433738,-3.73247428156342));
#32384=CARTESIAN_POINT('Ctrl Pts',(-46.9129076509211,-0.486735169392868,
-4.51338989581109));
#32385=CARTESIAN_POINT('Ctrl Pts',(-46.7939986519261,1.72864833483289,-4.19754385459079));
#32386=CARTESIAN_POINT('Ctrl Pts',(-46.6750896529311,3.52396726382821,-2.86168729951416));
#32387=CARTESIAN_POINT('Ctrl Pts',(-46.5561806539362,4.46295597112516,-0.830435714870097));
#32388=CARTESIAN_POINT('Ctrl Pts',(-46.4372716549412,4.31743855505023,1.40261320402286));
#32389=CARTESIAN_POINT('Ctrl Pts',(-46.3183626559463,3.12277600276341,3.2948246559261));
#32390=CARTESIAN_POINT('Ctrl Pts',(-46.1994536569513,1.1692734083998,4.38638794147786));
#32391=CARTESIAN_POINT('Ctrl Pts',(-46.0805446579563,-1.06836467363388,
4.41205126906581));
#32392=CARTESIAN_POINT('Ctrl Pts',(-45.9616356589614,-3.04638826741205,
3.36557840510464));
#32393=CARTESIAN_POINT('Ctrl Pts',(-45.8427266599664,-4.2841341726916,1.50126408972942));
#32394=CARTESIAN_POINT('Ctrl Pts',(-45.7238176609715,-4.48082796504582,
-0.727860030772266));
#32395=CARTESIAN_POINT('Ctrl Pts',(-45.6049086619765,-3.58867270818134,
-2.78011288804709));
#32396=CARTESIAN_POINT('Ctrl Pts',(-45.4859996629815,-1.82446369322749,
-4.15679344072332));
#32397=CARTESIAN_POINT('Ctrl Pts',(-45.3670906639866,0.383093196982726,
-4.52336590153015));
#32398=CARTESIAN_POINT('Ctrl Pts',(-45.2481816649916,2.49755776887068,-3.79075252000914));
#32399=CARTESIAN_POINT('Ctrl Pts',(-45.1292726659966,4.00511142534855,-2.13697963190314));
#32400=CARTESIAN_POINT('Ctrl Pts',(-45.0103636670017,4.53941598558409,0.0360830522584563));
#32401=CARTESIAN_POINT('Ctrl Pts',(-44.8914546680067,3.97063450487066,2.20037749159751));
#32402=CARTESIAN_POINT('Ctrl Pts',(-44.7725456690117,2.43698188009364,3.82997634355494));
#32403=CARTESIAN_POINT('Ctrl Pts',(-44.6536366700168,0.311138386869151,
4.52888423156623));
#32404=CARTESIAN_POINT('Ctrl Pts',(-44.5347276710218,-1.89031227931686,
4.12726531240721));
#32405=CARTESIAN_POINT('Ctrl Pts',(-44.4158186720269,-3.6324137491896,2.72271369023057));
#32406=CARTESIAN_POINT('Ctrl Pts',(-44.2969096730319,-4.49183230978425,
0.656537865318763));
#32407=CARTESIAN_POINT('Ctrl Pts',(-44.178000674037,-4.25972774921047,-1.56917780400555));
#32408=CARTESIAN_POINT('Ctrl Pts',(-44.059091675042,-2.9925018731896,-3.41358053176182));
#32409=CARTESIAN_POINT('Ctrl Pts',(-43.940182676047,-0.998092809298354,
-4.42847717693769));
#32410=CARTESIAN_POINT('Ctrl Pts',(-43.821273677052,1.2388545813571,-4.36724616652841));
#32411=CARTESIAN_POINT('Ctrl Pts',(-43.7023646780571,3.17475808804931,-3.24476656256246));
#32412=CARTESIAN_POINT('Ctrl Pts',(-43.5834556790621,4.33918991321652,-1.33380323702856));
#32413=CARTESIAN_POINT('Ctrl Pts',(-43.4645466800672,4.44919078769146,0.901277092518143));
#32414=CARTESIAN_POINT('Ctrl Pts',(-43.3456376810722,3.47803089423511,2.9173445518719));
#32415=CARTESIAN_POINT('Ctrl Pts',(-43.2267286820773,1.66170261573023,4.2244940813961));
#32416=CARTESIAN_POINT('Ctrl Pts',(-43.1078196830822,-0.558420751171717,
4.5050803342771));
#32417=CARTESIAN_POINT('Ctrl Pts',(-42.9889106840873,-2.64285000910083,
3.6909317730406));
#32418=CARTESIAN_POINT('Ctrl Pts',(-42.8700016850924,-4.08505587227025,
1.97986515005463));
#32419=CARTESIAN_POINT('Ctrl Pts',(-42.7510926860974,-4.53459839051628,
-0.212281901079125));
#32420=CARTESIAN_POINT('Ctrl Pts',(-42.6321836871025,-3.8822008248155,-2.35290448582148));
#32421=CARTESIAN_POINT('Ctrl Pts',(-42.5132746881075,-2.28647099457101,
-3.92164661926039));
#32422=CARTESIAN_POINT('Ctrl Pts',(-42.3943656891125,-0.135026251456862,
-4.53766227017941));
#32423=CARTESIAN_POINT('Ctrl Pts',(-42.2754566901175,2.04903365344401,-4.05053810450959));
#32424=CARTESIAN_POINT('Ctrl Pts',(-42.1565476911226,3.73556679230751,-2.58008372862802));
#32425=CARTESIAN_POINT('Ctrl Pts',(-42.0376386921276,4.51356845779047,-0.480753664312707));
#32426=CARTESIAN_POINT('Ctrl Pts',(-41.9187296931327,4.19632578309466,1.73158843219894));
#32427=CARTESIAN_POINT('Ctrl Pts',(-41.7998206941377,2.85625547461948,3.53074617269255));
#32428=CARTESIAN_POINT('Ctrl Pts',(-41.6809116951428,0.828308923028642,
4.45691773248095));
#32429=CARTESIAN_POINT('Ctrl Pts',(-41.5223663631495,-2.16015712884012,
4.28474797948406));
#32430=CARTESIAN_POINT('Ctrl Pts',(-41.3241846981579,-4.9740591081024,1.32908412483934));
#32431=CARTESIAN_POINT('Ctrl Pts',(-41.0863667001679,-3.80724186785295,
-3.46592527061159));
#32432=CARTESIAN_POINT('Ctrl Pts',(-40.8881850351764,0.0500896134690414,
-4.79821165639804));
#32433=CARTESIAN_POINT('Ctrl Pts',(-40.7296397031831,2.78352850293585,-3.5780134739008));
#32434=CARTESIAN_POINT('Ctrl Pts',(-40.6107307041881,4.15918402926478,-1.82360963009783));
#32435=CARTESIAN_POINT('Ctrl Pts',(-40.4918217051932,4.52276023745573,0.390113330814915));
#32436=CARTESIAN_POINT('Ctrl Pts',(-40.3729127061981,3.78802227944025,2.50086215521277));
#32437=CARTESIAN_POINT('Ctrl Pts',(-40.2540037072033,2.13242298822478,4.00799993834983));
#32438=CARTESIAN_POINT('Ctrl Pts',(-40.1350947082082,-0.0411755970567031,
4.53913013905057));
#32439=CARTESIAN_POINT('Ctrl Pts',(-40.0161857092133,-2.20486027926045,
3.96827445065634));
#32440=CARTESIAN_POINT('Ctrl Pts',(-39.8972767102183,-3.83271402254156,
2.43260457879703));
#32441=CARTESIAN_POINT('Ctrl Pts',(-39.7783677112234,-4.52923460703175,
0.306066394860525));
#32442=CARTESIAN_POINT('Ctrl Pts',(-39.6594587122284,-4.12513168363095,
-1.89497619022052));
#32443=CARTESIAN_POINT('Ctrl Pts',(-39.5405497132335,-2.71862032408285,
-3.63547122467695));
#32444=CARTESIAN_POINT('Ctrl Pts',(-39.4216407142385,-0.651476557450647,
-4.49257296200486));
#32445=CARTESIAN_POINT('Ctrl Pts',(-39.3027317152435,1.57397569950779,-4.25795526643815));
#32446=CARTESIAN_POINT('Ctrl Pts',(-39.1838227162486,3.41694983189919,-2.98865516129907));
#32447=CARTESIAN_POINT('Ctrl Pts',(-39.0649137172536,4.42959880069384,-0.993102512574686));
#32448=CARTESIAN_POINT('Ctrl Pts',(-38.9460047182586,4.36584768013456,1.24377373209122));
#32449=CARTESIAN_POINT('Ctrl Pts',(-38.8270957192637,3.24118782933984,3.17841180985207));
#32450=CARTESIAN_POINT('Ctrl Pts',(-38.7081867202687,1.32891370106109,4.34068973070986));
#32451=CARTESIAN_POINT('Ctrl Pts',(-38.5892777212737,-0.906288808862736,
4.44817269760705));
#32452=CARTESIAN_POINT('Ctrl Pts',(-38.4703687222788,-2.92126153819489,
3.47474177286519));
#32453=CARTESIAN_POINT('Ctrl Pts',(-38.3514597232838,-4.22636259933156,
1.65694257197947));
#32454=CARTESIAN_POINT('Ctrl Pts',(-38.2325507242889,-4.50445013822686,
-0.56349661064248));
#32455=CARTESIAN_POINT('Ctrl Pts',(-38.1136417252939,-3.68794839987019,
-2.64700511289908));
#32456=CARTESIAN_POINT('Ctrl Pts',(-37.9947327262989,-1.97526873561246,
-4.0872867413949));
#32457=CARTESIAN_POINT('Ctrl Pts',(-37.875823727304,0.217404693160681,-4.53435052369439));
#32458=CARTESIAN_POINT('Ctrl Pts',(-37.756914728309,2.35724840062552,-3.8795591832657));
#32459=CARTESIAN_POINT('Ctrl Pts',(-37.638005729314,3.92427661500994,-2.28202816042688));
#32460=CARTESIAN_POINT('Ctrl Pts',(-37.5190967303191,4.53769873376776,-0.12996029532479));
#32461=CARTESIAN_POINT('Ctrl Pts',(-37.4001877313241,4.04845210680413,2.05368814958598));
#32462=CARTESIAN_POINT('Ctrl Pts',(-37.2812787323292,2.57542452202649,3.7382867744424));
#32463=CARTESIAN_POINT('Ctrl Pts',(-37.1623697333342,0.476564264348535,
4.51447516094041));
#32464=CARTESIAN_POINT('Ctrl Pts',(-37.0434607343392,-1.73810194485508,
4.19363817060929));
#32465=CARTESIAN_POINT('Ctrl Pts',(-36.9245517353443,-3.53040633502461,
2.85373975449125));
#32466=CARTESIAN_POINT('Ctrl Pts',(-36.8056427363493,-4.4648157979083,0.820377576168181));
#32467=CARTESIAN_POINT('Ctrl Pts',(-36.6867337373543,-4.31426719625242,
-1.41233779106585));
#32468=CARTESIAN_POINT('Ctrl Pts',(-36.5678247383594,-3.11534410413089,
-3.30185259961615));
#32469=CARTESIAN_POINT('Ctrl Pts',(-36.4489157393644,-1.15938693432648,
-4.38901143917916));
#32470=CARTESIAN_POINT('Ctrl Pts',(-36.3300067403695,1.07830329261979,-4.40963280623902));
#32471=CARTESIAN_POINT('Ctrl Pts',(-36.2110977413745,3.05396392947723,-3.35870567245557));
#32472=CARTESIAN_POINT('Ctrl Pts',(-36.0921887423796,4.28750597867589,-1.49160717333758));
#32473=CARTESIAN_POINT('Ctrl Pts',(-35.9732797433846,4.47917656018556,0.73795448329676));
#32474=CARTESIAN_POINT('Ctrl Pts',(-35.8543707443897,3.58239938675126,2.78819190704975));
#32475=CARTESIAN_POINT('Ctrl Pts',(-35.7354617453947,1.81509288333212,4.1608938104223));
#32476=CARTESIAN_POINT('Ctrl Pts',(-35.6165527463997,-0.393284372117317,
4.52249122490932));
#32477=CARTESIAN_POINT('Ctrl Pts',(-35.4976437474047,-2.50609283581814,
3.78511534500529));
#32478=CARTESIAN_POINT('Ctrl Pts',(-35.3787347484098,-4.00991634789332,
2.12794980195292));
#32479=CARTESIAN_POINT('Ctrl Pts',(-35.2598257494148,-4.53932315910131,
-0.0463112727105621));
#32480=CARTESIAN_POINT('Ctrl Pts',(-35.1409167504199,-3.96566648640761,
-2.20931862693388));
#32481=CARTESIAN_POINT('Ctrl Pts',(-35.0220077514249,-2.42834590674615,
-3.83545768245756));
#32482=CARTESIAN_POINT('Ctrl Pts',(-34.9030987524299,-0.300933015493449,
-4.52957379859513));
#32483=CARTESIAN_POINT('Ctrl Pts',(-34.784189753435,1.89960712598062,-4.12299554252211));
#32484=CARTESIAN_POINT('Ctrl Pts',(-34.66528075444,3.63853940632953,-2.71452214308902));
#32485=CARTESIAN_POINT('Ctrl Pts',(-34.5463717554451,4.49330023353743,-0.646415105041655));
#32486=CARTESIAN_POINT('Ctrl Pts',(-34.4274627564501,4.25618122842175,1.57877193652657));
#32487=CARTESIAN_POINT('Ctrl Pts',(-34.3085537574552,2.98480272483288,3.4203146303467));
#32488=CARTESIAN_POINT('Ctrl Pts',(-34.1896447584602,0.988111927535212,
4.43071487408027));
#32489=CARTESIAN_POINT('Ctrl Pts',(-34.0707357594652,-1.24869180005395,
4.36444363753406));
#32490=CARTESIAN_POINT('Ctrl Pts',(-33.9518267604703,-3.18206123160157,
3.23760494734484));
#32491=CARTESIAN_POINT('Ctrl Pts',(-33.8329177614753,-4.3421842065533,1.32402258028056));
#32492=CARTESIAN_POINT('Ctrl Pts',(-33.7140087624803,-4.44714880860522,
-0.911299594455427));
#32493=CARTESIAN_POINT('Ctrl Pts',(-33.5950997634854,-3.47144845548349,
-2.92517437047002));
#32494=CARTESIAN_POINT('Ctrl Pts',(-33.4761907644904,-1.65218004314271,
-4.22822664739902));
#32495=CARTESIAN_POINT('Ctrl Pts',(-33.3572817654955,0.568571015518742,
-4.50381243803997));
#32496=CARTESIAN_POINT('Ctrl Pts',(-33.2383727665005,2.65115832085412,-3.68496391223899));
#32497=CARTESIAN_POINT('Ctrl Pts',(-33.1194637675055,4.08950950743749,-1.97066269698927));
#32498=CARTESIAN_POINT('Ctrl Pts',(-33.0005547685106,4.53410271588046,0.222513007678954));
#32499=CARTESIAN_POINT('Ctrl Pts',(-32.8816457695156,3.87690101727068,2.36161766148137));
#32500=CARTESIAN_POINT('Ctrl Pts',(-32.7627367705207,2.27760557628349,3.92684508423502));
#32501=CARTESIAN_POINT('Ctrl Pts',(-32.6438277715256,0.124847988200563,
4.53784226882032));
#32502=CARTESIAN_POINT('Ctrl Pts',(-32.5249187725308,-2.05824787981073,
4.04613582838238));
#32503=CARTESIAN_POINT('Ctrl Pts',(-32.4060097735357,-3.7411859055206,2.57121128994584));
#32504=CARTESIAN_POINT('Ctrl Pts',(-32.2871007745408,-4.51500919875398,
0.471477901174332));
#32505=CARTESIAN_POINT('Ctrl Pts',(-32.1681917755458,-4.19167734330492,
-1.74282544351886));
#32506=CARTESIAN_POINT('Ctrl Pts',(-32.0492827765509,-2.84976054604786,
-3.53361915160113));
#32507=CARTESIAN_POINT('Ctrl Pts',(-31.9303737775559,-0.815346942171119,
-4.46573721058515));
#32508=CARTESIAN_POINT('Ctrl Pts',(-31.8114647785609,1.41719739963958,-4.31267330363336));
#32509=CARTESIAN_POINT('Ctrl Pts',(-31.692555779566,3.30536028557706,-3.11162221793306));
#32510=CARTESIAN_POINT('Ctrl Pts',(-31.573646780571,4.39031483624702,-1.15444149335352));
#32511=CARTESIAN_POINT('Ctrl Pts',(-31.4547377815761,4.40841517156554,1.08327056534746));
#32512=CARTESIAN_POINT('Ctrl Pts',(-31.3358287825811,3.35526292348304,3.0577459225003));
#32513=CARTESIAN_POINT('Ctrl Pts',(-31.2169197835862,1.48677584407451,4.28918377176597));
#32514=CARTESIAN_POINT('Ctrl Pts',(-31.0980107845911,-0.743000251595862,
4.4783422257804));
#32515=CARTESIAN_POINT('Ctrl Pts',(-30.9791017855963,-2.79222622284383,
3.57925611035811));
#32516=CARTESIAN_POINT('Ctrl Pts',(-30.8601927866012,-4.16293585100342,
1.81040360708402));
#32517=CARTESIAN_POINT('Ctrl Pts',(-30.7412837876063,-4.52204572243967,
-0.398378390841908));
#32518=CARTESIAN_POINT('Ctrl Pts',(-30.6223747886113,-3.78228865854103,
-2.51035724352461));
#32519=CARTESIAN_POINT('Ctrl Pts',(-30.5034657896164,-2.12343261016916,
-4.01230789818306));
#32520=CARTESIAN_POINT('Ctrl Pts',(-30.3845567906214,0.0514288446811627,
-4.53927464464667));
#32521=CARTESIAN_POINT('Ctrl Pts',(-30.2656477916264,2.21377791403734,-3.96316187270984));
#32522=CARTESIAN_POINT('Ctrl Pts',(-30.1467387926315,3.83820517441539,-2.42404934636619));
#32523=CARTESIAN_POINT('Ctrl Pts',(-30.0278297936365,4.52988175982226,-0.295777679389505));
#32524=CARTESIAN_POINT('Ctrl Pts',(-29.9089207946416,4.12090930177574,1.90414584112476));
#32525=CARTESIAN_POINT('Ctrl Pts',(-29.7900117956466,2.71030542569923,3.64181896201337));
#32526=CARTESIAN_POINT('Ctrl Pts',(-29.71073912965,1.3311803135326,4.20948611409121));
#32527=CARTESIAN_POINT('Ctrl Pts',(-29.6711027966516,0.615324888853963,
4.3116474491314));
#32528=CARTESIAN_POINT('Ctrl Pts',(-52.575,2.36230756092333,-3.31488661006745));
#32529=CARTESIAN_POINT('Ctrl Pts',(-52.5353636670017,2.91267249451488,-2.92267674082431));
#32530=CARTESIAN_POINT('Ctrl Pts',(-52.456091001005,3.81372197207604,-1.85922435845946));
#32531=CARTESIAN_POINT('Ctrl Pts',(-52.3371820020101,4.2384739899776,0.188973964574656));
#32532=CARTESIAN_POINT('Ctrl Pts',(-52.2182730030151,3.63326518569111,2.1907646706185));
#32533=CARTESIAN_POINT('Ctrl Pts',(-52.0993640040202,2.14517071451495,3.66043213853357));
#32534=CARTESIAN_POINT('Ctrl Pts',(-51.9804550050252,0.135793741969793,
4.240490317549));
#32535=CARTESIAN_POINT('Ctrl Pts',(-51.8615460060302,-1.90658020276247,
3.79016093772832));
#32536=CARTESIAN_POINT('Ctrl Pts',(-51.7426370070353,-3.48565239142985,
2.41878623204276));
#32537=CARTESIAN_POINT('Ctrl Pts',(-51.6237280080403,-4.21770465133279,
0.459657053727601));
#32538=CARTESIAN_POINT('Ctrl Pts',(-51.5048190090453,-3.9248474328806,-1.61117702200155));
#32539=CARTESIAN_POINT('Ctrl Pts',(-51.3859100100504,-2.67824533662262,
-3.29048853499884));
#32540=CARTESIAN_POINT('Ctrl Pts',(-51.2670010110555,-0.78082496558402,
-4.17020743213141));
#32541=CARTESIAN_POINT('Ctrl Pts',(-51.1480920120604,1.30633725885353,-4.03655767907646));
#32542=CARTESIAN_POINT('Ctrl Pts',(-51.0291830130655,3.07605723061235,-2.9220178035111));
#32543=CARTESIAN_POINT('Ctrl Pts',(-50.9102740140706,4.09828990837908,-1.0974222453584));
#32544=CARTESIAN_POINT('Ctrl Pts',(-50.7913650150755,4.12463095289654,0.993848724235651));
#32545=CARTESIAN_POINT('Ctrl Pts',(-50.6724560160807,3.14867944761336,2.84361277085736));
#32546=CARTESIAN_POINT('Ctrl Pts',(-50.5535470170857,1.40759331717813,4.00237390050092));
#32547=CARTESIAN_POINT('Ctrl Pts',(-50.4346380180907,-0.675540456184353,
4.18855117202478));
#32548=CARTESIAN_POINT('Ctrl Pts',(-50.3157290190957,-2.59451671479358,
3.35690315989496));
#32549=CARTESIAN_POINT('Ctrl Pts',(-50.1968200201008,-3.88302086412996,
1.7095217998619));
#32550=CARTESIAN_POINT('Ctrl Pts',(-50.0779110211058,-4.22794413760432,
-0.353276355744105));
#32551=CARTESIAN_POINT('Ctrl Pts',(-49.9590020221109,-3.54546957514818,
-2.33022773676946));
#32552=CARTESIAN_POINT('Ctrl Pts',(-49.8400930231158,-2.00143969166412,
-3.74092969395146));
#32553=CARTESIAN_POINT('Ctrl Pts',(-49.721184024121,0.0289435448964663,
-4.2425791784024));
#32554=CARTESIAN_POINT('Ctrl Pts',(-49.6022750251259,2.05229344931449,-3.71327448649327));
#32555=CARTESIAN_POINT('Ctrl Pts',(-49.4833660261311,3.57693244841941,-2.28163758591345));
#32556=CARTESIAN_POINT('Ctrl Pts',(-49.364457027136,4.23237059313566,-0.295558752875362));
#32557=CARTESIAN_POINT('Ctrl Pts',(-49.2455480281411,3.85933526548734,1.76234137516302));
#32558=CARTESIAN_POINT('Ctrl Pts',(-49.1266390291461,2.54847470392539,3.39198946010828));
#32559=CARTESIAN_POINT('Ctrl Pts',(-49.0077300301511,0.618330322503512,
4.19737816098522));
#32560=CARTESIAN_POINT('Ctrl Pts',(-48.8888210311563,-1.46206941105725,
3.98279661184051));
#32561=CARTESIAN_POINT('Ctrl Pts',(-48.7699120321612,-3.18718371510779,
2.80038850522416));
#32562=CARTESIAN_POINT('Ctrl Pts',(-48.6510030331662,-4.13780679009204,
0.937481083493075));
#32563=CARTESIAN_POINT('Ctrl Pts',(-48.5320940341714,-4.08293556259652,
-1.15323588468445));
#32564=CARTESIAN_POINT('Ctrl Pts',(-48.4131850351763,-3.03590383707744,
-2.96371451156447));
#32565=CARTESIAN_POINT('Ctrl Pts',(-48.2942760361814,-1.2511421580073,-4.05400531752194));
#32566=CARTESIAN_POINT('Ctrl Pts',(-48.1753670371864,0.837649258381883,
-4.15916572571611));
#32567=CARTESIAN_POINT('Ctrl Pts',(-48.0564580381915,2.72289043680534,-3.25364157263724));
#32568=CARTESIAN_POINT('Ctrl Pts',(-47.9375490391965,3.94646446657405,-1.55747681462926));
#32569=CARTESIAN_POINT('Ctrl Pts',(-47.8186400402015,4.21104071385062,0.517157539180999));
#32570=CARTESIAN_POINT('Ctrl Pts',(-47.6997310412066,3.45232668681426,2.46612170452907));
#32571=CARTESIAN_POINT('Ctrl Pts',(-47.5808220422116,1.85469122386101,3.81581397321361));
#32572=CARTESIAN_POINT('Ctrl Pts',(-47.4619130432167,-0.193637457276558,
4.23825675828857));
#32573=CARTESIAN_POINT('Ctrl Pts',(-47.3430040442216,-2.19491189690037,
3.6307957225496));
#32574=CARTESIAN_POINT('Ctrl Pts',(-47.2240950452268,-3.66281889847391,
2.14104496240076));
#32575=CARTESIAN_POINT('Ctrl Pts',(-47.1051860462317,-4.24065448775976,
0.131016523699623));
#32576=CARTESIAN_POINT('Ctrl Pts',(-46.9862770472369,-3.78800360376758,
-1.91084915989804));
#32577=CARTESIAN_POINT('Ctrl Pts',(-46.8673680482418,-2.41486120468549,
-3.4883751484243));
#32578=CARTESIAN_POINT('Ctrl Pts',(-46.748459049247,-0.454903300248022,
-4.21821986167895));
#32579=CARTESIAN_POINT('Ctrl Pts',(-46.6295500502518,1.61559690347559,-3.92302975511522));
#32580=CARTESIAN_POINT('Ctrl Pts',(-46.510641051257,3.29350422793804,-2.67453654201874));
#32581=CARTESIAN_POINT('Ctrl Pts',(-46.391732052262,4.17108425236453,-0.776126261452312));
#32582=CARTESIAN_POINT('Ctrl Pts',(-46.2728230532671,4.03508349265237,1.3108840609923));
#32583=CARTESIAN_POINT('Ctrl Pts',(-46.153914054272,2.91855037178518,3.0793472589807));
#32584=CARTESIAN_POINT('Ctrl Pts',(-46.0350050552771,1.09280439512275,4.09952367575057));
#32585=CARTESIAN_POINT('Ctrl Pts',(-45.9160960562821,-0.998494964953347,
4.123508653926));
#32586=CARTESIAN_POINT('Ctrl Pts',(-45.7971870572872,-2.84715829844654,
3.14547380177063));
#32587=CARTESIAN_POINT('Ctrl Pts',(-45.6782780582922,-4.00395717509747,
1.40308330259685));
#32588=CARTESIAN_POINT('Ctrl Pts',(-45.5593690592973,-4.18778744031509,
-0.680258898345004));
#32589=CARTESIAN_POINT('Ctrl Pts',(-45.4404600603022,-3.35397801744653,
-2.59829699467222));
#32590=CARTESIAN_POINT('Ctrl Pts',(-45.3215510613074,-1.70514605769533,
-3.88494436716616));
#32591=CARTESIAN_POINT('Ctrl Pts',(-45.2026420623123,0.358039382745663,
-4.22754344914553));
#32592=CARTESIAN_POINT('Ctrl Pts',(-45.0837330633174,2.33422062563635,-3.54284206322451));
#32593=CARTESIAN_POINT('Ctrl Pts',(-44.9648240643225,3.74318216521078,-1.997223846241));
#32594=CARTESIAN_POINT('Ctrl Pts',(-44.8459150653275,4.24254387784786,0.0337232659310005));
#32595=CARTESIAN_POINT('Ctrl Pts',(-44.7270060663325,3.71095999205786,2.05647556548625));
#32596=CARTESIAN_POINT('Ctrl Pts',(-44.6080970673375,2.27760632395248,3.57950069794286));
#32597=CARTESIAN_POINT('Ctrl Pts',(-44.4891880683426,0.290790326898236,
4.23270088732366));
#32598=CARTESIAN_POINT('Ctrl Pts',(-44.3702790693477,-1.76668822890541,
3.85734734137919));
#32599=CARTESIAN_POINT('Ctrl Pts',(-44.2513700703527,-3.39485844927514,
2.54465163234734));
#32600=CARTESIAN_POINT('Ctrl Pts',(-44.1324610713577,-4.19807211471991,
0.61360111299095));
#32601=CARTESIAN_POINT('Ctrl Pts',(-44.0135520723628,-3.98114690107788,
-1.46655554520236));
#32602=CARTESIAN_POINT('Ctrl Pts',(-43.8946430733678,-2.79679600676983,
-3.19033664959511));
#32603=CARTESIAN_POINT('Ctrl Pts',(-43.7757340743728,-0.932818792342456,
-4.1388603280403));
#32604=CARTESIAN_POINT('Ctrl Pts',(-43.6568250753779,1.15783504670461,-4.0816337488567));
#32605=CARTESIAN_POINT('Ctrl Pts',(-43.5379160763829,2.96713289393957,-3.03256290209179));
#32606=CARTESIAN_POINT('Ctrl Pts',(-43.4190070773879,4.05541233929616,-1.24657417947145));
#32607=CARTESIAN_POINT('Ctrl Pts',(-43.300098078393,4.15821929464979,0.842334701919917));
#32608=CARTESIAN_POINT('Ctrl Pts',(-43.181189079398,3.25057203925852,2.72655387993142));
#32609=CARTESIAN_POINT('Ctrl Pts',(-43.0622800804031,1.55302935037421,3.94821747091449));
#32610=CARTESIAN_POINT('Ctrl Pts',(-42.9433710814082,-0.521900734955894,
4.21045373503939));
#32611=CARTESIAN_POINT('Ctrl Pts',(-42.824462082413,-2.47001093572135,3.44954946781609));
#32612=CARTESIAN_POINT('Ctrl Pts',(-42.7055530834183,-3.81789834564735,
1.85038445430061));
#32613=CARTESIAN_POINT('Ctrl Pts',(-42.5866440844232,-4.23804134745061,
-0.198398931197613));
#32614=CARTESIAN_POINT('Ctrl Pts',(-42.4677350854283,-3.62830976367934,
-2.19902748573468));
#32615=CARTESIAN_POINT('Ctrl Pts',(-42.3488260864333,-2.13693866142688,
-3.66517585267858));
#32616=CARTESIAN_POINT('Ctrl Pts',(-42.2299170874383,-0.126195704091931,
-4.24090485322945));
#32617=CARTESIAN_POINT('Ctrl Pts',(-42.1110080884434,1.91502942438633,-3.78563799657268));
#32618=CARTESIAN_POINT('Ctrl Pts',(-41.9920990894484,3.49126541284734,-2.41134949120931));
#32619=CARTESIAN_POINT('Ctrl Pts',(-41.8731900904535,4.21838674592901,-0.449312978092323));
#32620=CARTESIAN_POINT('Ctrl Pts',(-41.7542810914585,3.92189134396604,1.61834472216421));
#32621=CARTESIAN_POINT('Ctrl Pts',(-41.6353720924635,2.66945995165433,3.29983980467131));
#32622=CARTESIAN_POINT('Ctrl Pts',(-41.5164630934686,0.77413855912781,4.16544090694865));
#32623=CARTESIAN_POINT('Ctrl Pts',(-41.3579177614753,-2.01888556396995,
4.00453083969612));
#32624=CARTESIAN_POINT('Ctrl Pts',(-41.1597360964837,-4.64876188570278,
1.24216369129613));
#32625=CARTESIAN_POINT('Ctrl Pts',(-40.9219180984938,-3.5582530284162,-3.23925810822545));
#32626=CARTESIAN_POINT('Ctrl Pts',(-40.7237364335021,0.0468138156189731,
-4.48441463662212));
#32627=CARTESIAN_POINT('Ctrl Pts',(-40.5651911015089,2.60148923263442,-3.34401588370882));
#32628=CARTESIAN_POINT('Ctrl Pts',(-40.4462821025139,3.88717861421759,-1.70434784922236));
#32629=CARTESIAN_POINT('Ctrl Pts',(-40.327373103519,4.22697739474136,0.364600408636661));
#32630=CARTESIAN_POINT('Ctrl Pts',(-40.208464104524,3.54029037696192,2.33730890925922));
#32631=CARTESIAN_POINT('Ctrl Pts',(-40.0895551055291,1.99296520133986,3.74588177308733));
#32632=CARTESIAN_POINT('Ctrl Pts',(-39.9706461065341,-0.0384827646914282,
4.24227672531885));
#32633=CARTESIAN_POINT('Ctrl Pts',(-39.8517371075391,-2.06066518446267,
3.70875428242689));
#32634=CARTESIAN_POINT('Ctrl Pts',(-39.7328281085442,-3.58205933615999,
2.27351529266644));
#32635=CARTESIAN_POINT('Ctrl Pts',(-39.6139191095492,-4.23302834867352,
0.28605003680078));
#32636=CARTESIAN_POINT('Ctrl Pts',(-39.4950101105542,-3.85535324924685,
-1.77104712588996));
#32637=CARTESIAN_POINT('Ctrl Pts',(-39.3761011115593,-2.54082596720782,
-3.39771596970325));
#32638=CARTESIAN_POINT('Ctrl Pts',(-39.2571921125643,-0.608870808304631,
-4.19876432921494));
#32639=CARTESIAN_POINT('Ctrl Pts',(-39.1382831135694,1.47103966436091,-3.97949033645411));
#32640=CARTESIAN_POINT('Ctrl Pts',(-39.0193741145744,3.19348560173252,-2.79320086500867));
#32641=CARTESIAN_POINT('Ctrl Pts',(-38.9004651155794,4.13990859901063,-0.928154854760866));
#32642=CARTESIAN_POINT('Ctrl Pts',(-38.7815561165844,4.08032672171768,1.16243249115508));
#32643=CARTESIAN_POINT('Ctrl Pts',(-38.6626471175895,3.02921821353002,2.97054766692245));
#32644=CARTESIAN_POINT('Ctrl Pts',(-38.5437381185945,1.24200441301907,4.05681407060795));
#32645=CARTESIAN_POINT('Ctrl Pts',(-38.4248291195996,-0.84701865830611,
4.15726778637903));
#32646=CARTESIAN_POINT('Ctrl Pts',(-38.3059201206046,-2.73021470026535,
3.2474980222978));
#32647=CARTESIAN_POINT('Ctrl Pts',(-38.1870111216096,-3.94996379012226,
1.5485806075101));
#32648=CARTESIAN_POINT('Ctrl Pts',(-38.0681021226147,-4.20986475301984,
-0.526644639588315));
#32649=CARTESIAN_POINT('Ctrl Pts',(-37.9491931236197,-3.44676120350641,
-2.47389430094654));
#32650=CARTESIAN_POINT('Ctrl Pts',(-37.8302841246248,-1.8460886395937,-3.81998331873136));
#32651=CARTESIAN_POINT('Ctrl Pts',(-37.7113751256298,0.203186699106992,
-4.23780969080775));
#32652=CARTESIAN_POINT('Ctrl Pts',(-37.5924661266349,2.20308731396286,-3.6258408821712));
#32653=CARTESIAN_POINT('Ctrl Pts',(-37.4735571276399,3.6676338500072,-2.13278638305928));
#32654=CARTESIAN_POINT('Ctrl Pts',(-37.3546481286449,4.24093893214488,-0.121461055132279));
#32655=CARTESIAN_POINT('Ctrl Pts',(-37.23573912965,3.78368842049889,1.91937952232278));
#32656=CARTESIAN_POINT('Ctrl Pts',(-37.116830130655,2.40699499087144,3.49380751156464));
#32657=CARTESIAN_POINT('Ctrl Pts',(-36.9979211316601,0.445397559627416,
4.219234151831));
#32658=CARTESIAN_POINT('Ctrl Pts',(-36.8790121326651,-1.62443225926818,
3.91937949796381));
#32659=CARTESIAN_POINT('Ctrl Pts',(-36.7601031336701,-3.2995221919603,2.66710875646485));
#32660=CARTESIAN_POINT('Ctrl Pts',(-36.6411941346751,-4.17282244881044,
0.766725912396867));
#32661=CARTESIAN_POINT('Ctrl Pts',(-36.5222851356802,-4.03211953673935,
-1.31997267224866));
#32662=CARTESIAN_POINT('Ctrl Pts',(-36.4033761366853,-2.91160450999496,
-3.08591558397465));
#32663=CARTESIAN_POINT('Ctrl Pts',(-36.2844671376902,-1.08356448404466,
-4.10197559999513));
#32664=CARTESIAN_POINT('Ctrl Pts',(-36.1655581386953,1.00778361073219,-4.1212483555325));
#32665=CARTESIAN_POINT('Ctrl Pts',(-36.0466491397003,2.85423852172137,-3.1390505372104));
#32666=CARTESIAN_POINT('Ctrl Pts',(-35.9277401407054,4.00710846920256,-1.394057936416));
#32667=CARTESIAN_POINT('Ctrl Pts',(-35.8088311417104,4.18624403525991,0.689693186344611));
#32668=CARTESIAN_POINT('Ctrl Pts',(-35.6899221427155,3.34811496336391,2.60584765597262));
#32669=CARTESIAN_POINT('Ctrl Pts',(-35.5710131437205,1.69638808700519,3.88877657783347));
#32670=CARTESIAN_POINT('Ctrl Pts',(-35.4521041447256,-0.36756406781807,
4.22672597527783));
#32671=CARTESIAN_POINT('Ctrl Pts',(-35.3331951457305,-2.34219750991838,
3.53757355239032));
#32672=CARTESIAN_POINT('Ctrl Pts',(-35.2142861467357,-3.74767285185209,
1.98878455583559));
#32673=CARTESIAN_POINT('Ctrl Pts',(-35.0953771477406,-4.24245712210054,
-0.0432825736036531));
#32674=CARTESIAN_POINT('Ctrl Pts',(-34.9764681487457,-3.70631687576659,
-2.06483196179423));
#32675=CARTESIAN_POINT('Ctrl Pts',(-34.8575591497507,-2.26953513242235,
-3.58462356416123));
#32676=CARTESIAN_POINT('Ctrl Pts',(-34.7386501507558,-0.281252374001066,
-4.2333453575344));
#32677=CARTESIAN_POINT('Ctrl Pts',(-34.6197411517608,1.77537520426393,-3.8533568090853));
#32678=CARTESIAN_POINT('Ctrl Pts',(-34.5008321527659,3.40058349612684,-2.5369958021071));
#32679=CARTESIAN_POINT('Ctrl Pts',(-34.3819231537709,4.19944403810212,-0.604140368530221));
#32680=CARTESIAN_POINT('Ctrl Pts',(-34.2630141547759,3.97783231829727,1.47552223349874));
#32681=CARTESIAN_POINT('Ctrl Pts',(-34.144105155781,2.78960037305193,3.19663034658495));
#32682=CARTESIAN_POINT('Ctrl Pts',(-34.025196156786,0.92349064771896,4.14095168259845));
#32683=CARTESIAN_POINT('Ctrl Pts',(-33.9062871577911,-1.16702892364603,
4.07901450174094));
#32684=CARTESIAN_POINT('Ctrl Pts',(-33.7873781587961,-2.97395842107017,
3.02586964752038));
#32685=CARTESIAN_POINT('Ctrl Pts',(-33.6684691598011,-4.05821080960704,
1.23743316539842));
#32686=CARTESIAN_POINT('Ctrl Pts',(-33.5495601608062,-4.15631085843277,
-0.851701744810404));
#32687=CARTESIAN_POINT('Ctrl Pts',(-33.4306511618112,-3.24442008373921,
-2.73387163822095));
#32688=CARTESIAN_POINT('Ctrl Pts',(-33.3117421628162,-1.5441295420815,-3.95170593178579));
#32689=CARTESIAN_POINT('Ctrl Pts',(-33.1928331638213,0.531387184754894,
-4.20926875762475));
#32690=CARTESIAN_POINT('Ctrl Pts',(-33.0739241648263,2.47777589431427,-3.44397189762026));
#32691=CARTESIAN_POINT('Ctrl Pts',(-32.9550151658313,3.82206071866471,-1.84178383011512));
#32692=CARTESIAN_POINT('Ctrl Pts',(-32.8361061668364,4.23757808931381,0.207960936267553));
#32693=CARTESIAN_POINT('Ctrl Pts',(-32.7171971678414,3.62335655689582,2.20717083064289));
#32694=CARTESIAN_POINT('Ctrl Pts',(-32.5982881688465,2.12865303036779,3.67003434456881));
#32695=CARTESIAN_POINT('Ctrl Pts',(-32.4793791698515,0.116683086477182,
4.24107308018517));
#32696=CARTESIAN_POINT('Ctrl Pts',(-32.3604701708566,-1.92364105191405,
3.78152362377861));
#32697=CARTESIAN_POINT('Ctrl Pts',(-32.2415611718616,-3.49651704310921,
2.40305729888056));
#32698=CARTESIAN_POINT('Ctrl Pts',(-32.1226521728666,-4.21973326424187,
0.440643838220576));
#32699=CARTESIAN_POINT('Ctrl Pts',(-32.0037431738717,-3.91754690630399,
-1.62884684704813));
#32700=CARTESIAN_POINT('Ctrl Pts',(-31.8848341748767,-2.66338978325909,
-3.30252489436533));
#32701=CARTESIAN_POINT('Ctrl Pts',(-31.7659251758817,-0.762024275548931,
-4.17368360225475));
#32702=CARTESIAN_POINT('Ctrl Pts',(-31.6470161768868,1.32451446852128,-4.03062988269698));
#32703=CARTESIAN_POINT('Ctrl Pts',(-31.5281071778918,3.08919387167645,-2.90812603048288));
#32704=CARTESIAN_POINT('Ctrl Pts',(-31.4091981788968,4.10319375653073,-1.07894246870398));
#32705=CARTESIAN_POINT('Ctrl Pts',(-31.2902891799019,4.12011035263834,1.01242603005823));
#32706=CARTESIAN_POINT('Ctrl Pts',(-31.1713801809069,3.13583293969945,2.85777317714776));
#32707=CARTESIAN_POINT('Ctrl Pts',(-31.0524711819119,1.38954257002262,4.00867653673046));
#32708=CARTESIAN_POINT('Ctrl Pts',(-30.933562182917,-0.694408967730227,
4.18546426527762));
#32709=CARTESIAN_POINT('Ctrl Pts',(-30.8146531839221,-2.6096181325775,3.34517725330154));
#32710=CARTESIAN_POINT('Ctrl Pts',(-30.6957441849271,-3.89068507152368,
1.6920054835379));
#32711=CARTESIAN_POINT('Ctrl Pts',(-30.5768351859321,-4.22630960811051,
-0.37232494411191));
#32712=CARTESIAN_POINT('Ctrl Pts',(-30.4579261869372,-3.53493172767287,
-2.34618303071339));
#32713=CARTESIAN_POINT('Ctrl Pts',(-30.3390171879422,-1.98456278272466,
-3.74990799775467));
#32714=CARTESIAN_POINT('Ctrl Pts',(-30.2201081889473,0.0480654627907762,
-4.24241178043034));
#32715=CARTESIAN_POINT('Ctrl Pts',(-30.1011991899523,2.06899961711827,-3.70397606066096));
#32716=CARTESIAN_POINT('Ctrl Pts',(-29.9822901909573,3.58719137359357,-2.26551956169834));
#32717=CARTESIAN_POINT('Ctrl Pts',(-29.8633811919623,4.23363317848382,-0.276434190407516));
#32718=CARTESIAN_POINT('Ctrl Pts',(-29.7444721929674,3.85140700586516,1.77961709313449));
#32719=CARTESIAN_POINT('Ctrl Pts',(-29.6255631939724,2.53305485274192,3.40364857298535));
#32720=CARTESIAN_POINT('Ctrl Pts',(-29.5462905279758,1.24412279187993,3.93419100583383));
#32721=CARTESIAN_POINT('Ctrl Pts',(-29.5066541949775,0.575083413457821,
4.02967111779183));
#32722=CARTESIAN_POINT('',(-30.,0.695807839646249,4.87560011181053));
#32723=CARTESIAN_POINT('Ctrl Pts',(-30.,3.27123863458584,-2.42269058837956));
#32724=CARTESIAN_POINT('Ctrl Pts',(-30.,3.33974878250541,-2.34761006208624));
#32725=CARTESIAN_POINT('Ctrl Pts',(-30.,3.40533192358328,-2.27003566591244));
#32726=CARTESIAN_POINT('Ctrl Pts',(-30.,3.46783702656801,-2.19012891506847));
#32727=CARTESIAN_POINT('Ctrl Pts',(-30.,3.54519073167044,-2.09123965730679));
#32728=CARTESIAN_POINT('Ctrl Pts',(-30.,3.61783178849963,-1.98877939676093));
#32729=CARTESIAN_POINT('Ctrl Pts',(-30.,3.68567008600155,-1.88315345760476));
#32730=CARTESIAN_POINT('Ctrl Pts',(-30.,3.72452568859522,-1.82265430496434));
#32731=CARTESIAN_POINT('Ctrl Pts',(-30.,3.76180511742509,-1.76111580012076));
#32732=CARTESIAN_POINT('Ctrl Pts',(-30.,3.79748638403424,-1.69860841143877));
#32733=CARTESIAN_POINT('Ctrl Pts',(-30.,3.81574456349527,-1.66662324867262));
#32734=CARTESIAN_POINT('Ctrl Pts',(-30.,3.8335842187764,-1.63438433328503));
#32735=CARTESIAN_POINT('Ctrl Pts',(-30.,3.85100199058494,-1.60190075176667));
#32736=CARTESIAN_POINT('Ctrl Pts',(-30.,3.86219018238585,-1.58103513563606));
#32737=CARTESIAN_POINT('Ctrl Pts',(-30.,3.87320429714474,-1.56006856433113));
#32738=CARTESIAN_POINT('Ctrl Pts',(-30.,3.8840433802687,-1.5390033991797));
#32739=CARTESIAN_POINT('Ctrl Pts',(-30.,3.8935038434821,-1.52061750641368));
#32740=CARTESIAN_POINT('Ctrl Pts',(-30.,3.90282656389723,-1.5021650534667));
#32741=CARTESIAN_POINT('Ctrl Pts',(-30.,3.91201089233721,-1.48364853923209));
#32742=CARTESIAN_POINT('Ctrl Pts',(-30.,3.96947385833632,-1.36779751813259));
#32743=CARTESIAN_POINT('Ctrl Pts',(-30.,4.02152672316031,-1.24943342811707));
#32744=CARTESIAN_POINT('Ctrl Pts',(-30.,4.06807409839169,-1.12898161068632));
#32745=CARTESIAN_POINT('Ctrl Pts',(-30.,4.11491088273489,-1.00778088199419));
#32746=CARTESIAN_POINT('Ctrl Pts',(-30.,4.1561739627056,-0.88446569930994));
#32747=CARTESIAN_POINT('Ctrl Pts',(-30.,4.19172616679095,-0.759434914895517));
#32748=CARTESIAN_POINT('Ctrl Pts',(-30.,4.2041994658364,-0.715568538562162));
#32749=CARTESIAN_POINT('Ctrl Pts',(-30.,4.21596941142744,-0.671490725785992));
#32750=CARTESIAN_POINT('Ctrl Pts',(-30.,4.22702875952034,-0.627217950078772));
#32751=CARTESIAN_POINT('Ctrl Pts',(-30.,4.23745336325369,-0.58548618261418));
#32752=CARTESIAN_POINT('Ctrl Pts',(-30.,4.24724659311391,-0.543581183826834));
#32753=CARTESIAN_POINT('Ctrl Pts',(-30.,4.25640178065254,-0.501516507038128));
#32754=CARTESIAN_POINT('Ctrl Pts',(-30.,4.26067116719361,-0.481900266062384));
#32755=CARTESIAN_POINT('Ctrl Pts',(-30.,4.26479982210057,-0.462258272543662));
#32756=CARTESIAN_POINT('Ctrl Pts',(-30.,4.26878682150122,-0.442595092139843));
#32757=CARTESIAN_POINT('Ctrl Pts',(-30.,4.27969785634821,-0.38878378568377));
#32758=CARTESIAN_POINT('Ctrl Pts',(-30.,4.28954967875665,-0.334806539222378));
#32759=CARTESIAN_POINT('Ctrl Pts',(-30.,4.29833606013692,-0.280694354437186));
#32760=CARTESIAN_POINT('Ctrl Pts',(-30.,4.31910350792121,-0.152795060816309));
#32761=CARTESIAN_POINT('Ctrl Pts',(-30.,4.33392210423418,-0.0241436844331786));
#32762=CARTESIAN_POINT('Ctrl Pts',(-30.,4.34293706986683,0.104855255691433));
#32763=CARTESIAN_POINT('Ctrl Pts',(-30.,4.35209692663439,0.235927504090205));
#32764=CARTESIAN_POINT('Ctrl Pts',(-30.,4.35526525016914,0.367359263948117));
#32765=CARTESIAN_POINT('Ctrl Pts',(-30.,4.3525451613485,0.498747926672244));
#32766=CARTESIAN_POINT('Ctrl Pts',(-30.,4.35009455980085,0.617119524603827));
#32767=CARTESIAN_POINT('Ctrl Pts',(-30.,4.342863896526,0.735456818994498));
#32768=CARTESIAN_POINT('Ctrl Pts',(-30.,4.33089384577612,0.85347290367371));
#32769=CARTESIAN_POINT('Ctrl Pts',(-30.,4.32191630771371,0.941984967183119));
#32770=CARTESIAN_POINT('Ctrl Pts',(-30.,4.3102721913265,1.03031653659682));
#32771=CARTESIAN_POINT('Ctrl Pts',(-30.,4.29596640419823,1.11834673365244));
#32772=CARTESIAN_POINT('Ctrl Pts',(-30.,4.29282291216298,1.1376901099256));
#32773=CARTESIAN_POINT('Ctrl Pts',(-30.,4.28955086420591,1.15701893097116));
#32774=CARTESIAN_POINT('Ctrl Pts',(-30.,4.28615024400599,1.17633190572179));
#32775=CARTESIAN_POINT('Ctrl Pts',(-30.,4.28275399423854,1.1956200596906));
#32776=CARTESIAN_POINT('Ctrl Pts',(-30.,4.27923068225399,1.21488549492892));
#32777=CARTESIAN_POINT('Ctrl Pts',(-30.,4.27558221590421,1.2341187299655));
#32778=CARTESIAN_POINT('Ctrl Pts',(-30.,4.25019481772672,1.36795079782698));
#32779=CARTESIAN_POINT('Ctrl Pts',(-30.,4.2187302622092,1.50034532596835));
#32780=CARTESIAN_POINT('Ctrl Pts',(-30.,4.18131898274086,1.63087582632965));
#32781=CARTESIAN_POINT('Ctrl Pts',(-30.,4.15599233816626,1.7192422130391));
#32782=CARTESIAN_POINT('Ctrl Pts',(-30.,4.1279392470965,1.80675472203661));
#32783=CARTESIAN_POINT('Ctrl Pts',(-30.,4.09718685463689,1.89328334475779));
#32784=CARTESIAN_POINT('Ctrl Pts',(-30.,4.05202657818314,2.02035171930402));
#32785=CARTESIAN_POINT('Ctrl Pts',(-30.,4.00104764212238,2.1452989823121));
#32786=CARTESIAN_POINT('Ctrl Pts',(-30.,3.9445356482452,2.26782052204027));
#32787=CARTESIAN_POINT('Ctrl Pts',(-30.,3.88754811032845,2.39137307100984));
#32788=CARTESIAN_POINT('Ctrl Pts',(-30.,3.82493372767001,2.51245961368684));
#32789=CARTESIAN_POINT('Ctrl Pts',(-30.,3.75693418422412,2.63075452573071));
#32790=CARTESIAN_POINT('Ctrl Pts',(-30.,3.737983670491,2.66372164935602));
#32791=CARTESIAN_POINT('Ctrl Pts',(-30.,3.71861462433676,2.6964718440802));
#32792=CARTESIAN_POINT('Ctrl Pts',(-30.,3.69883162247989,2.72899776234456));
#32793=CARTESIAN_POINT('Ctrl Pts',(-30.,3.68688439772594,2.74864060818989));
#32794=CARTESIAN_POINT('Ctrl Pts',(-30.,3.67478619315373,2.76820165491218));
#32795=CARTESIAN_POINT('Ctrl Pts',(-30.,3.66253796903456,2.78767925573459));
#32796=CARTESIAN_POINT('Ctrl Pts',(-30.,3.65179479048755,2.80476347474192));
#32797=CARTESIAN_POINT('Ctrl Pts',(-30.,3.64093530565375,2.82178475520501));
#32798=CARTESIAN_POINT('Ctrl Pts',(-30.,3.62997054880261,2.83872623143875));
#32799=CARTESIAN_POINT('Ctrl Pts',(-30.,3.55452366838117,2.95529803954384));
#32800=CARTESIAN_POINT('Ctrl Pts',(-30.,3.47399244884128,3.06826045209769));
#32801=CARTESIAN_POINT('Ctrl Pts',(-30.,3.38870779675817,3.17730699510021));
#32802=CARTESIAN_POINT('Ctrl Pts',(-30.,3.30236442727477,3.28770723386977));
#32803=CARTESIAN_POINT('Ctrl Pts',(-30.,3.2111485886733,3.39409451140229));
#32804=CARTESIAN_POINT('Ctrl Pts',(-30.,3.11535169160701,3.49613785110227));
#32805=CARTESIAN_POINT('Ctrl Pts',(-30.,3.02057348092696,3.59709608090682));
#32806=CARTESIAN_POINT('Ctrl Pts',(-30.,2.92131065748878,3.6938029330822));
#32807=CARTESIAN_POINT('Ctrl Pts',(-30.,2.81780079208004,3.78591489553778));
#32808=CARTESIAN_POINT('Ctrl Pts',(-30.,2.74290681629881,3.85256198331119));
#32809=CARTESIAN_POINT('Ctrl Pts',(-30.,2.66578849251642,3.91680311881087));
#32810=CARTESIAN_POINT('Ctrl Pts',(-30.,2.58658176109254,3.97857999207842));
#32811=CARTESIAN_POINT('Ctrl Pts',(-30.,2.55153627131115,4.00591353737064));
#32812=CARTESIAN_POINT('Ctrl Pts',(-30.,2.51608180945682,4.03276453049069));
#32813=CARTESIAN_POINT('Ctrl Pts',(-30.,2.48022957230527,4.05912727077957));
#32814=CARTESIAN_POINT('Ctrl Pts',(-30.,2.45986378047589,4.07410257283691));
#32815=CARTESIAN_POINT('Ctrl Pts',(-30.,2.4393696290117,4.08892031865678));
#32816=CARTESIAN_POINT('Ctrl Pts',(-30.,2.41874912476045,4.10357940212803));
#32817=CARTESIAN_POINT('Ctrl Pts',(-30.,2.40331171174522,4.11455383433459));
#32818=CARTESIAN_POINT('Ctrl Pts',(-30.,2.38780322466491,4.12543944891267));
#32819=CARTESIAN_POINT('Ctrl Pts',(-30.,2.37223705386536,4.13622726943165));
#32820=CARTESIAN_POINT('Ctrl Pts',(-30.,2.25664934302075,4.21633299966218));
#32821=CARTESIAN_POINT('Ctrl Pts',(-30.,2.13771882511829,4.291167679162));
#32822=CARTESIAN_POINT('Ctrl Pts',(-30.,2.01587786606652,4.36063638947179));
#32823=CARTESIAN_POINT('Ctrl Pts',(-30.,1.89144311327298,4.43158397443468));
#32824=CARTESIAN_POINT('Ctrl Pts',(-30.,1.76397219298052,4.49693520894599));
#32825=CARTESIAN_POINT('Ctrl Pts',(-30.,1.63388274786013,4.55655607176829));
#32826=CARTESIAN_POINT('Ctrl Pts',(-30.,1.50331560745686,4.61639586553387));
#32827=CARTESIAN_POINT('Ctrl Pts',(-30.,1.37011002491396,4.6704635809884));
#32828=CARTESIAN_POINT('Ctrl Pts',(-30.,1.23465431498687,4.71858368863437));
#32829=CARTESIAN_POINT('Ctrl Pts',(-30.,1.10035269443314,4.76629381057425));
#32830=CARTESIAN_POINT('Ctrl Pts',(-30.,0.96383842616513,4.80815761322486));
#32831=CARTESIAN_POINT('Ctrl Pts',(-30.,0.825466850475934,4.8439586961056));
#32832=CARTESIAN_POINT('Ctrl Pts',(-30.,0.782423564497787,4.85509534928808));
#32833=CARTESIAN_POINT('Ctrl Pts',(-30.,0.739200428308711,4.86564499042763));
#32834=CARTESIAN_POINT('Ctrl Pts',(-30.,0.695807839646249,4.87560011181053));
#32835=CARTESIAN_POINT('Ctrl Pts',(-30.,0.695807839646318,4.87560011181052));
#32836=CARTESIAN_POINT('Ctrl Pts',(-30.0396363329983,1.505295356838,4.76007633060594));
#32837=CARTESIAN_POINT('Ctrl Pts',(-30.0792726659966,2.28505096422592,4.43911803533769));
#32838=CARTESIAN_POINT('Ctrl Pts',(-30.118908998995,2.94077998825037,3.95114615387622));
#32839=CARTESIAN_POINT('Ctrl Pts',(-30.1585453319933,3.59650901227486,3.46317427241473));
#32840=CARTESIAN_POINT('Ctrl Pts',(-30.1981816649916,4.12821145293587,2.80818880476));
#32841=CARTESIAN_POINT('Ctrl Pts',(-30.2378179979899,4.47114017808342,2.06608473852283));
#32842=CARTESIAN_POINT('Ctrl Pts',(-30.2774543309882,4.81406890323096,1.32398067228571));
#32843=CARTESIAN_POINT('Ctrl Pts',(-30.3170906639866,4.96822391286505,0.494758007466152));
#32844=CARTESIAN_POINT('Ctrl Pts',(-30.3567269969849,4.91494372660875,-0.320960701335019));
#32845=CARTESIAN_POINT('Ctrl Pts',(-30.3963633299832,4.86166354035245,-1.13667941013621));
#32846=CARTESIAN_POINT('Ctrl Pts',(-30.4359996629815,4.60094815820575,-1.93889416291902));
#32847=CARTESIAN_POINT('Ctrl Pts',(-30.4756359959798,4.16444075576848,-2.63007230282805));
#32848=CARTESIAN_POINT('Ctrl Pts',(-30.5152723289782,3.72793335333121,-3.3212504427371));
#32849=CARTESIAN_POINT('Ctrl Pts',(-30.5549086619765,3.11563393060335,-3.90139196977236));
#32850=CARTESIAN_POINT('Ctrl Pts',(-30.5945449949748,2.40195440267049,-4.30004054600194));
#32851=CARTESIAN_POINT('Ctrl Pts',(-30.6341813279731,1.68827487473765,-4.69868912223151));
#32852=CARTESIAN_POINT('Ctrl Pts',(-30.6738176609715,0.873215241599798,
-4.91584474765542));
#32853=CARTESIAN_POINT('Ctrl Pts',(-30.7134539939698,0.0557974461108648,
-4.92510711469413));
#32854=CARTESIAN_POINT('Ctrl Pts',(-30.7530903269681,-0.761620349378092,
-4.93436948173283));
#32855=CARTESIAN_POINT('Ctrl Pts',(-30.7927266599664,-1.58139630721813,
-4.73573859038633));
#32856=CARTESIAN_POINT('Ctrl Pts',(-30.8323629929647,-2.30392266200803,
-4.35335613973094));
#32857=CARTESIAN_POINT('Ctrl Pts',(-30.8719993259631,-3.02644901679793,
-3.97097368907555));
#32858=CARTESIAN_POINT('Ctrl Pts',(-30.9116356589614,-3.65172576853768,
-3.40483967911129));
#32859=CARTESIAN_POINT('Ctrl Pts',(-30.9512719919597,-4.10378338287765,
-2.72373594332161));
#32860=CARTESIAN_POINT('Ctrl Pts',(-30.990908324958,-4.55584099721759,-2.04263220753197));
#32861=CARTESIAN_POINT('Ctrl Pts',(-31.0305446579563,-4.83467947415777,
-1.24655874591693));
#32862=CARTESIAN_POINT('Ctrl Pts',(-31.0701809909546,-4.90641862243869,
-0.432241158696399));
#32863=CARTESIAN_POINT('Ctrl Pts',(-31.0771734853352,-4.91907457603671,
-0.288582280038523));
#32864=CARTESIAN_POINT('Ctrl Pts',(-31.0841659797158,-4.92528503863494,
-0.144355594868911));
#32865=CARTESIAN_POINT('Ctrl Pts',(-31.0911584740964,-4.92514031288301,
-0.000116505347877993));
#32866=CARTESIAN_POINT('Origin',(-53.,4.5,0.));
#32867=CARTESIAN_POINT('',(-53.,-4.5,-5.51091059616309E-16));
#32868=CARTESIAN_POINT('Origin',(-53.,0.,0.));
#32869=CARTESIAN_POINT('Origin',(-52.75,0.,0.));
#32870=CARTESIAN_POINT('',(-52.75,-4.75,-5.81707229594993E-16));
#32871=CARTESIAN_POINT('Origin',(-41.25,0.,0.));
#32872=CARTESIAN_POINT('Origin',(-30.,0.,0.));
#32873=CARTESIAN_POINT('Origin',(-30.,8.,0.));
#32874=CARTESIAN_POINT('',(-30.,-8.,-9.79717439317883E-16));
#32875=CARTESIAN_POINT('Origin',(-30.,0.,0.));
#32876=CARTESIAN_POINT('Origin',(0.,0.,0.));
#32877=CARTESIAN_POINT('',(30.,-8.,-9.79717439317883E-16));
#32878=CARTESIAN_POINT('Origin',(30.,0.,0.));
#32879=CARTESIAN_POINT('',(0.,-8.,-9.79717439317883E-16));
#32880=CARTESIAN_POINT('Origin',(30.,5.,0.));
#32881=CARTESIAN_POINT('Origin',(52.75,0.,0.));
#32882=CARTESIAN_POINT('',(53.,-4.5,-5.51091059616309E-16));
#32883=CARTESIAN_POINT('Origin',(53.,0.,0.));
#32884=CARTESIAN_POINT('',(52.75,-4.75,-5.81707229594993E-16));
#32885=CARTESIAN_POINT('Origin',(53.,0.,0.));
#32886=CARTESIAN_POINT('',(0.,0.,0.));
#32887=CARTESIAN_POINT('Origin',(8.31492550064808,0.,-2.41787080875326E-16));
#32888=CARTESIAN_POINT('',(8.4,-7.26300281800529,8.89461315326838E-16));
#32889=CARTESIAN_POINT('Origin',(8.4,0.,0.));
#32890=CARTESIAN_POINT('',(8.27136742382219,-7.74615915544327,-0.000941532553519379));
#32891=CARTESIAN_POINT('',(8.31492550064808,-7.580184099288,-1.41187898116472E-15));
#32892=CARTESIAN_POINT('',(8.23004515173475,-7.70339232440972,-1.73638161370287));
#32893=CARTESIAN_POINT('Ctrl Pts',(8.27136742382219,-7.74615915544327,-0.000941532553519405));
#32894=CARTESIAN_POINT('Ctrl Pts',(8.27114725188007,-7.74616681794042,-0.064564222478092));
#32895=CARTESIAN_POINT('Ctrl Pts',(8.27077282593737,-7.74599899203376,-0.128189559455883));
#32896=CARTESIAN_POINT('Ctrl Pts',(8.27025171390506,-7.7456553806079,-0.191831784430464));
#32897=CARTESIAN_POINT('Ctrl Pts',(8.26916283644786,-7.74493739539079,-0.324813906898557));
#32898=CARTESIAN_POINT('Ctrl Pts',(8.26743494441316,-7.74345241079881,-0.457721426103084));
#32899=CARTESIAN_POINT('Ctrl Pts',(8.26514537190407,-7.741203690555,-0.590678771338576));
#32900=CARTESIAN_POINT('Ctrl Pts',(8.26401462256671,-7.74009311689312,-0.656342308712543));
#32901=CARTESIAN_POINT('Ctrl Pts',(8.26274700585539,-7.73879620770269,-0.722017728961687));
#32902=CARTESIAN_POINT('Ctrl Pts',(8.2613337016924,-7.73731374873599,-0.787718335582255));
#32903=CARTESIAN_POINT('Ctrl Pts',(8.25841332256419,-7.73425047167353,-0.923478694398744));
#32904=CARTESIAN_POINT('Ctrl Pts',(8.25487528348693,-7.73039901514795,-1.05914211268319));
#32905=CARTESIAN_POINT('Ctrl Pts',(8.25065191470568,-7.72577657208149,-1.19484477917841));
#32906=CARTESIAN_POINT('Ctrl Pts',(8.2466296968618,-7.72137428709354,-1.32408418850076));
#32907=CARTESIAN_POINT('Ctrl Pts',(8.24198575526578,-7.71627263760997,-1.45335936506934));
#32908=CARTESIAN_POINT('Ctrl Pts',(8.23668284834012,-7.7104847667795,-1.58274529764113));
#32909=CARTESIAN_POINT('Ctrl Pts',(8.23461699541548,-7.7082299865146,-1.63315016254979));
#32910=CARTESIAN_POINT('Ctrl Pts',(8.23245137951942,-7.7058710484806,-1.68357135020396));
#32911=CARTESIAN_POINT('Ctrl Pts',(8.23018478415278,-7.7034086872879,-1.73401135130111));
#32912=CARTESIAN_POINT('',(8.23406708607797,-5.35358430006243,-5.80403694227773));
#32913=CARTESIAN_POINT('Origin',(8.22985100129616,0.,-4.83574161750652E-16));
#32914=CARTESIAN_POINT('',(8.23005205545796,-2.349628256023,-7.53857080762849));
#32915=CARTESIAN_POINT('Ctrl Pts',(8.23529955888936,-5.35220883424223,-5.80478584085023));
#32916=CARTESIAN_POINT('Ctrl Pts',(8.24135251359355,-5.24157560348415,-5.87606344132463));
#32917=CARTESIAN_POINT('Ctrl Pts',(8.24663904490831,-5.13069470185511,-5.94667945173788));
#32918=CARTESIAN_POINT('Ctrl Pts',(8.25115307889962,-5.01950382509813,-6.01665379089667));
#32919=CARTESIAN_POINT('Ctrl Pts',(8.25514467229576,-4.92118184297989,-6.07852951239622));
#32920=CARTESIAN_POINT('Ctrl Pts',(8.25853265795554,-4.82261664919146,-6.13990399257126));
#32921=CARTESIAN_POINT('Ctrl Pts',(8.26132675188252,-4.72373802018084,-6.20080573283235));
#32922=CARTESIAN_POINT('Ctrl Pts',(8.26482295844291,-4.60001271943482,-6.27701113945212));
#32923=CARTESIAN_POINT('Ctrl Pts',(8.2673830227026,-4.47597208224258,-6.3523685972828));
#32924=CARTESIAN_POINT('Ctrl Pts',(8.26904864667115,-4.35149112259367,-6.42693880010717));
#32925=CARTESIAN_POINT('Ctrl Pts',(8.26988529460047,-4.28896396214428,-6.46439563728045));
#32926=CARTESIAN_POINT('Ctrl Pts',(8.27049679382362,-4.22632502082287,-6.50165417994343));
#32927=CARTESIAN_POINT('Ctrl Pts',(8.2708913591938,-4.16355502052887,-6.53872370512012));
#32928=CARTESIAN_POINT('Ctrl Pts',(8.27184482310895,-4.01187184010239,-6.62830190249728));
#32929=CARTESIAN_POINT('Ctrl Pts',(8.27152555460945,-3.85965879652205,-6.71663856576674));
#32930=CARTESIAN_POINT('Ctrl Pts',(8.27008277805002,-3.70666429170934,-6.80387205524455));
#32931=CARTESIAN_POINT('Ctrl Pts',(8.26899334829348,-3.59113928886561,-6.86974140873753));
#32932=CARTESIAN_POINT('Ctrl Pts',(8.26726627003468,-3.47529564565701,-6.93490905860148));
#32933=CARTESIAN_POINT('Ctrl Pts',(8.264979096865,-3.35902727876003,-6.99944001442568));
#32934=CARTESIAN_POINT('Ctrl Pts',(8.26384953248748,-3.30160591372285,-7.03130986578313));
#32935=CARTESIAN_POINT('Ctrl Pts',(8.26258348671553,-3.24408116185127,-7.0630242403131));
#32936=CARTESIAN_POINT('Ctrl Pts',(8.26117208730693,-3.18644188536852,-7.09459047623395));
#32937=CARTESIAN_POINT('Ctrl Pts',(8.25825582835368,-3.06734657111715,-7.1598132030989));
#32938=CARTESIAN_POINT('Ctrl Pts',(8.25472340542738,-2.94794142432279,-7.22430479440537));
#32939=CARTESIAN_POINT('Ctrl Pts',(8.25050669481373,-2.82811703428188,-7.28814827091774));
#32940=CARTESIAN_POINT('Ctrl Pts',(8.24649089566865,-2.71400185608383,-7.34894982973649));
#32941=CARTESIAN_POINT('Ctrl Pts',(8.24185434137902,-2.59950625281144,-7.4091635865651));
#32942=CARTESIAN_POINT('Ctrl Pts',(8.23655941543651,-2.48457179585488,-7.46883845050572));
#32943=CARTESIAN_POINT('Ctrl Pts',(8.23449571308963,-2.43977598357458,-7.49209678463563));
#32944=CARTESIAN_POINT('Ctrl Pts',(8.23233224536128,-2.3949139212779,-7.51527300286226));
#32945=CARTESIAN_POINT('Ctrl Pts',(8.23006777285707,-2.34998381317915,-7.53836899137533));
#32946=CARTESIAN_POINT('',(8.23406708607796,2.3496512864847,-7.53835847629444));
#32947=CARTESIAN_POINT('Origin',(8.22985100129616,0.,-4.83574161750652E-16));
#32948=CARTESIAN_POINT('',(8.23005205545723,5.35377969962258,-5.80412316297992));
#32949=CARTESIAN_POINT('Ctrl Pts',(8.23529955888937,2.35098758458347,-7.53754173723834));
#32950=CARTESIAN_POINT('Ctrl Pts',(8.24135251359366,2.46803241269599,-7.47736934913535));
#32951=CARTESIAN_POINT('Ctrl Pts',(8.24663904490848,2.58462812244407,-7.41665167673576));
#32952=CARTESIAN_POINT('Ctrl Pts',(8.25115307889983,2.70082311614886,-7.35534472237359));
#32953=CARTESIAN_POINT('Ctrl Pts',(8.25514467229588,2.8035700539023,-7.30113324885945));
#32954=CARTESIAN_POINT('Ctrl Pts',(8.25853265795559,2.90600450977038,-7.24646052719819));
#32955=CARTESIAN_POINT('Ctrl Pts',(8.26132675188253,3.00818627847469,-7.19127999271513));
#32956=CARTESIAN_POINT('Ctrl Pts',(8.26482295844286,3.13604474688414,-7.12223344248917));
#32957=CARTESIAN_POINT('Ctrl Pts',(8.26738302270252,3.2633265383243,-7.05248982849551));
#32958=CARTESIAN_POINT('Ctrl Pts',(8.26904864667108,3.39014670815809,-6.98197125656537));
#32959=CARTESIAN_POINT('Ctrl Pts',(8.26988529460043,3.45384886092223,-6.94654956577526));
#32960=CARTESIAN_POINT('Ctrl Pts',(8.27049679382361,3.51743517603901,-6.91093192265516));
#32961=CARTESIAN_POINT('Ctrl Pts',(8.2708913591938,3.5809233266972,-6.87510627039224));
#32962=CARTESIAN_POINT('Ctrl Pts',(8.27184482310895,3.73434191146413,-6.78853388150475));
#32963=CARTESIAN_POINT('Ctrl Pts',(8.27152555460945,3.88695022773128,-6.70088185061152));
#32964=CARTESIAN_POINT('Ctrl Pts',(8.27008277805002,4.03899389808625,-6.61200146754316));
#32965=CARTESIAN_POINT('Ctrl Pts',(8.26899334829347,4.15380093296388,-6.54488855705472));
#32966=CARTESIAN_POINT('Ctrl Pts',(8.26726627003468,4.26815959485526,-6.47714884410112));
#32967=CARTESIAN_POINT('Ctrl Pts',(8.264979096865,4.38217922537795,-6.40872296262395));
#32968=CARTESIAN_POINT('Ctrl Pts',(8.26384953248747,4.43849000878697,-6.37492952746046));
#32969=CARTESIAN_POINT('Ctrl Pts',(8.26258348671552,4.49471783873088,-6.34096881825824));
#32970=CARTESIAN_POINT('Ctrl Pts',(8.26117208730692,4.5508746391816,-6.30683485852883));
#32971=CARTESIAN_POINT('Ctrl Pts',(8.25825582835373,4.66690683467426,-6.23630665434924));
#32972=CARTESIAN_POINT('Ctrl Pts',(8.2547234054275,4.78246076447121,-6.16514455953727));
#32973=CARTESIAN_POINT('Ctrl Pts',(8.25050669481395,4.89766303201517,-6.09329533202641));
#32974=CARTESIAN_POINT('Ctrl Pts',(8.2464908956689,5.0073763156408,-6.02486946815899));
#32975=CARTESIAN_POINT('Ctrl Pts',(8.24185434137931,5.11677076034776,-5.95582024551788));
#32976=CARTESIAN_POINT('Ctrl Pts',(8.23655941543682,5.22591793696589,-5.88612151799374));
#32977=CARTESIAN_POINT('Ctrl Pts',(8.23449571308984,5.26845815131449,-5.85895637363939));
#32978=CARTESIAN_POINT('Ctrl Pts',(8.23233224536139,5.31096037621297,-5.83169279713619));
#32979=CARTESIAN_POINT('Ctrl Pts',(8.23006777285706,5.35342714304242,-5.80433017638299));
#32980=CARTESIAN_POINT('',(8.23016251323912,7.70340607746227,-1.73438940040554));
#32981=CARTESIAN_POINT('Origin',(8.22985100129616,0.,-4.83574161750652E-16));
#32982=CARTESIAN_POINT('',(8.23416387505949,7.7032334399193,1.73431147348199));
#32983=CARTESIAN_POINT('Ctrl Pts',(8.23018478415278,7.70340868728788,-1.73401135130117));
#32984=CARTESIAN_POINT('Ctrl Pts',(8.23606248521678,7.70979404535193,-1.60321109798711));
#32985=CARTESIAN_POINT('Ctrl Pts',(8.24125906760293,7.71548549605284,-1.47252342627014));
#32986=CARTESIAN_POINT('Ctrl Pts',(8.24580484326341,7.72046864985948,-1.34188213816602));
#32987=CARTESIAN_POINT('Ctrl Pts',(8.24986158901183,7.72491572105892,-1.22529510667363));
#32988=CARTESIAN_POINT('Ctrl Pts',(8.25340050977611,7.72879871129239,-1.10874408188086));
#32989=CARTESIAN_POINT('Ctrl Pts',(8.25645834823089,7.73210645326191,-0.99215053002542));
#32990=CARTESIAN_POINT('Ctrl Pts',(8.25997021137989,7.7359053253413,-0.858245288062264));
#32991=CARTESIAN_POINT('Ctrl Pts',(8.26284235113813,7.73894065122346,-0.724458427579585));
#32992=CARTESIAN_POINT('Ctrl Pts',(8.26514559776231,7.74120355991351,-0.590678780796379));
#32993=CARTESIAN_POINT('Ctrl Pts',(8.26659397190069,7.74262656793607,-0.506552756858444));
#32994=CARTESIAN_POINT('Ctrl Pts',(8.26781796450162,7.74374408224676,-0.422428818173793));
#32995=CARTESIAN_POINT('Ctrl Pts',(8.26879776569929,7.74455470315058,-0.338274320859049));
#32996=CARTESIAN_POINT('Ctrl Pts',(8.27084831243718,7.74625118612486,-0.162154174894971));
#32997=CARTESIAN_POINT('Ctrl Pts',(8.27182204063112,7.74660194359562,0.0138274237015491));
#32998=CARTESIAN_POINT('Ctrl Pts',(8.27155825637708,7.74560977596245,0.189957727593904));
#32999=CARTESIAN_POINT('Ctrl Pts',(8.27133104131297,7.74475515545753,0.341670567454257));
#33000=CARTESIAN_POINT('Ctrl Pts',(8.27018653488307,7.74290486336108,0.493304050874034));
#33001=CARTESIAN_POINT('Ctrl Pts',(8.26805044484228,7.74006940953455,0.645040539895604));
#33002=CARTESIAN_POINT('Ctrl Pts',(8.26738920277765,7.73919167437049,0.692011663473354));
#33003=CARTESIAN_POINT('Ctrl Pts',(8.26663319490192,7.73821950084626,0.738992406975978));
#33004=CARTESIAN_POINT('Ctrl Pts',(8.26578093504743,7.73715311288952,0.785987382532037));
#33005=CARTESIAN_POINT('Ctrl Pts',(8.26331387784144,7.73406621388893,0.922024874477323));
#33006=CARTESIAN_POINT('Ctrl Pts',(8.26004379084571,7.73019397599313,1.05797667576818));
#33007=CARTESIAN_POINT('Ctrl Pts',(8.25594566859687,7.7255526051338,1.19397572905201));
#33008=CARTESIAN_POINT('Ctrl Pts',(8.25203090646028,7.72111890067145,1.32388984875875));
#33009=CARTESIAN_POINT('Ctrl Pts',(8.24736050788044,7.71598329279669,1.45384728169982));
#33010=CARTESIAN_POINT('Ctrl Pts',(8.24193338497957,7.71015840635703,1.58392070057521));
#33011=CARTESIAN_POINT('Ctrl Pts',(8.23986380764802,7.70793714600331,1.63352285701424));
#33012=CARTESIAN_POINT('Ctrl Pts',(8.23768441207748,7.70561563896657,1.68314140347541));
#33013=CARTESIAN_POINT('Ctrl Pts',(8.23539599829651,7.70319454879583,1.73277853165711));
#33014=CARTESIAN_POINT('',(8.23406708607805,5.35358430006271,5.80403694227756));
#33015=CARTESIAN_POINT('Origin',(8.22985100129616,0.,-4.83574161750652E-16));
#33016=CARTESIAN_POINT('',(8.23005205545717,2.34962825602276,7.53857080762868));
#33017=CARTESIAN_POINT('Ctrl Pts',(8.23529955888929,5.35220883424264,5.80478584084999));
#33018=CARTESIAN_POINT('Ctrl Pts',(8.24135251359347,5.24157560348494,5.87606344132415));
#33019=CARTESIAN_POINT('Ctrl Pts',(8.24663904490822,5.13069470185628,5.94667945173717));
#33020=CARTESIAN_POINT('Ctrl Pts',(8.25115307889952,5.01950382509967,6.01665379089573));
#33021=CARTESIAN_POINT('Ctrl Pts',(8.25514467229569,4.92118184298078,6.07852951239569));
#33022=CARTESIAN_POINT('Ctrl Pts',(8.25853265795549,4.8226166491917,6.13990399257113));
#33023=CARTESIAN_POINT('Ctrl Pts',(8.26132675188249,4.72373802018044,6.20080573283262));
#33024=CARTESIAN_POINT('Ctrl Pts',(8.26482295844295,4.60001271943165,6.27701113945411));
#33025=CARTESIAN_POINT('Ctrl Pts',(8.26738302270268,4.47597208223666,6.35236859728643));
#33026=CARTESIAN_POINT('Ctrl Pts',(8.26904864667122,4.35149112258499,6.4269388001124));
#33027=CARTESIAN_POINT('Ctrl Pts',(8.26988529460048,4.28896396213838,6.46439563728399));
#33028=CARTESIAN_POINT('Ctrl Pts',(8.2704967938236,4.22632502081977,6.50165417994529));
#33029=CARTESIAN_POINT('Ctrl Pts',(8.27089135919375,4.16355502052857,6.53872370512033));
#33030=CARTESIAN_POINT('Ctrl Pts',(8.2718448231089,4.01187184010217,6.62830190249743));
#33031=CARTESIAN_POINT('Ctrl Pts',(8.2715255546094,3.8596587965218,6.71663856576692));
#33032=CARTESIAN_POINT('Ctrl Pts',(8.27008277804997,3.70666429170905,6.80387205524474));
#33033=CARTESIAN_POINT('Ctrl Pts',(8.26899334829342,3.59113928886542,6.86974140873767));
#33034=CARTESIAN_POINT('Ctrl Pts',(8.26726627003463,3.47529564565692,6.93490905860157));
#33035=CARTESIAN_POINT('Ctrl Pts',(8.26497909686495,3.35902727876005,6.99944001442571));
#33036=CARTESIAN_POINT('Ctrl Pts',(8.26384953248743,3.30160591372274,7.03130986578322));
#33037=CARTESIAN_POINT('Ctrl Pts',(8.26258348671547,3.24408116185103,7.06302424031326));
#33038=CARTESIAN_POINT('Ctrl Pts',(8.26117208730687,3.18644188536816,7.09459047623419));
#33039=CARTESIAN_POINT('Ctrl Pts',(8.25825582835368,3.06734657111932,7.15981320309774));
#33040=CARTESIAN_POINT('Ctrl Pts',(8.25472340542746,2.9479414243275,7.22430479440286));
#33041=CARTESIAN_POINT('Ctrl Pts',(8.25050669481393,2.82811703428916,7.2881482709139));
#33042=CARTESIAN_POINT('Ctrl Pts',(8.24649089566889,2.71400185609146,7.34894982973249));
#33043=CARTESIAN_POINT('Ctrl Pts',(8.24185434137931,2.59950625281942,7.40916358656095));
#33044=CARTESIAN_POINT('Ctrl Pts',(8.23655941543684,2.48457179586321,7.46883845050143));
#33045=CARTESIAN_POINT('Ctrl Pts',(8.23449571308983,2.43977598357996,7.49209678463289));
#33046=CARTESIAN_POINT('Ctrl Pts',(8.23233224536135,2.3949139212803,7.51527300286106));
#33047=CARTESIAN_POINT('Ctrl Pts',(8.23006777285699,2.34998381317858,7.53836899137566));
#33048=CARTESIAN_POINT('',(8.23005205545787,-2.34962825602266,7.53857080762868));
#33049=CARTESIAN_POINT('Origin',(8.22985100129616,0.,-4.83574161750652E-16));
#33050=CARTESIAN_POINT('',(8.23406708607805,-5.35358430006267,5.8040369422776));
#33051=CARTESIAN_POINT('Ctrl Pts',(8.23006777285699,-2.34998381317852,7.53836899137568));
#33052=CARTESIAN_POINT('Ctrl Pts',(8.23593724524199,-2.46644185285449,7.47850460064909));
#33053=CARTESIAN_POINT('Ctrl Pts',(8.24112605624522,-2.58245558527781,7.41809559395111));
#33054=CARTESIAN_POINT('Ctrl Pts',(8.24566489205474,-2.69807519938032,7.35709638054601));
#33055=CARTESIAN_POINT('Ctrl Pts',(8.24971614773269,-2.80127448610756,7.30264994978083));
#33056=CARTESIAN_POINT('Ctrl Pts',(8.25325006140408,-2.90416059898131,7.24773285475222));
#33057=CARTESIAN_POINT('Ctrl Pts',(8.25630367580332,-3.00679603469776,7.19229611263911));
#33058=CARTESIAN_POINT('Ctrl Pts',(8.2598103660455,-3.12465986223869,7.12863402004664));
#33059=CARTESIAN_POINT('Ctrl Pts',(8.26267849028981,-3.24203961276667,7.06436972340848));
#33060=CARTESIAN_POINT('Ctrl Pts',(8.26497932272721,-3.35902720524777,6.99943990601788));
#33061=CARTESIAN_POINT('Ctrl Pts',(8.26642617872781,-3.43259370988549,6.95860942467462));
#33062=CARTESIAN_POINT('Ctrl Pts',(8.26764928689471,-3.5060057796466,6.9175153435751));
#33063=CARTESIAN_POINT('Ctrl Pts',(8.26862878428063,-3.57929097436323,6.87614013651681));
#33064=CARTESIAN_POINT('Ctrl Pts',(8.27067869519549,-3.73266363538966,6.78954930965762));
#33065=CARTESIAN_POINT('Ctrl Pts',(8.27165433670821,-3.88524391789899,6.70186202116604));
#33066=CARTESIAN_POINT('Ctrl Pts',(8.27139442937721,-4.03728187947163,6.61293714414642));
#33067=CARTESIAN_POINT('Ctrl Pts',(8.27117054495976,-4.16824752143661,6.5363371721061));
#33068=CARTESIAN_POINT('Ctrl Pts',(8.27003074605399,-4.29864682375577,6.45891436751854));
#33069=CARTESIAN_POINT('Ctrl Pts',(8.26790031375505,-4.42864291466266,6.38058668870114));
#33070=CARTESIAN_POINT('Ctrl Pts',(8.26724093283417,-4.46887744461066,6.35634382634158));
#33071=CARTESIAN_POINT('Ctrl Pts',(8.2664869086185,-4.5090731150744,6.33201437801959));
#33072=CARTESIAN_POINT('Ctrl Pts',(8.26563674296381,-4.54923402841569,6.30759623376819));
#33073=CARTESIAN_POINT('Ctrl Pts',(8.2631754786934,-4.66550151173327,6.23690470951749));
#33074=CARTESIAN_POINT('Ctrl Pts',(8.25991192457676,-4.78130226349205,6.16557584420391));
#33075=CARTESIAN_POINT('Ctrl Pts',(8.25582077331136,-4.89675945875543,6.093557235874));
#33076=CARTESIAN_POINT('Ctrl Pts',(8.2519127078451,-5.00704975319055,6.02476157961894));
#33077=CARTESIAN_POINT('Ctrl Pts',(8.24724941988421,-5.11702669300951,5.95533638684039));
#33078=CARTESIAN_POINT('Ctrl Pts',(8.24182957345511,-5.22675947892738,5.88525628231459));
#33079=CARTESIAN_POINT('Ctrl Pts',(8.23976246583453,-5.26861112195184,5.85852801242517));
#33080=CARTESIAN_POINT('Ctrl Pts',(8.23758553184529,-5.31042683092239,5.83170470527504));
#33081=CARTESIAN_POINT('Ctrl Pts',(8.23529955888929,-5.3522088342426,5.80478584085003));
#33082=CARTESIAN_POINT('',(8.23416387505187,-7.70323343991956,1.73431147348703));
#33083=CARTESIAN_POINT('Origin',(8.22985100129616,0.,-4.83574161750652E-16));
#33084=CARTESIAN_POINT('Ctrl Pts',(8.23539599829651,-7.70319454879582,1.73277853165718));
#33085=CARTESIAN_POINT('Ctrl Pts',(8.24145629544956,-7.7096062065087,1.6013268907403));
#33086=CARTESIAN_POINT('Ctrl Pts',(8.24675009530479,-7.71532104571645,1.46999154471252));
#33087=CARTESIAN_POINT('Ctrl Pts',(8.25127107718454,-7.72032516451686,1.33870852056237));
#33088=CARTESIAN_POINT('Ctrl Pts',(8.25526860263604,-7.72474988746401,1.2226259428503));
#33089=CARTESIAN_POINT('Ctrl Pts',(8.25866233313259,-7.72861895281961,1.10658330096045));
#33090=CARTESIAN_POINT('Ctrl Pts',(8.26146180005289,-7.73192193321259,0.990505496974222));
#33091=CARTESIAN_POINT('Ctrl Pts',(8.26496480270566,-7.73605498761474,0.84525610954886));
#33092=CARTESIAN_POINT('Ctrl Pts',(8.26753103166903,-7.73929605042608,0.700157460155893));
#33093=CARTESIAN_POINT('Ctrl Pts',(8.26920181683445,-7.74163519278412,0.555070887179658));
#33094=CARTESIAN_POINT('Ctrl Pts',(8.27004107552342,-7.74281017661169,0.482191878230534));
#33095=CARTESIAN_POINT('Ctrl Pts',(8.27065492237978,-7.74375753797758,0.40931515587787));
#33096=CARTESIAN_POINT('Ctrl Pts',(8.27105152573793,-7.74447567221088,0.336419375462664));
#33097=CARTESIAN_POINT('Ctrl Pts',(8.27166357551873,-7.74558391774399,0.223924497373578));
#33098=CARTESIAN_POINT('Ctrl Pts',(8.27175674710727,-7.74614548493137,0.111495968856029));
#33099=CARTESIAN_POINT('Ctrl Pts',(8.27136742382219,-7.74615915544327,-0.000941532553519405));
#33100=CARTESIAN_POINT('Ctrl Pts',(7.18908433792779,0.266497816746017,9.08374172079725));
#33101=CARTESIAN_POINT('Ctrl Pts',(7.58326629775444,1.49147728388782,8.37649949569117));
#33102=CARTESIAN_POINT('Ctrl Pts',(8.01233031911798,3.87343953744646,7.00127294739956));
#33103=CARTESIAN_POINT('Ctrl Pts',(7.71466028436332,6.10019622706514,5.71565437322842));
#33104=CARTESIAN_POINT('Ctrl Pts',(7.1890843379278,7.73350218325398,4.77266473975377));
#33105=CARTESIAN_POINT('Ctrl Pts',(7.34585286708095,0.177665211164012,9.01725418637031));
#33106=CARTESIAN_POINT('Ctrl Pts',(7.74659985034045,1.41147052678102,8.3070863945685));
#33107=CARTESIAN_POINT('Ctrl Pts',(8.18799973158063,3.82236863432499,6.91940076517965));
#33108=CARTESIAN_POINT('Ctrl Pts',(7.88018217809361,6.07777058358531,5.61372014708539));
#33109=CARTESIAN_POINT('Ctrl Pts',(7.34585286708095,7.72033859219626,4.66248967942191));
#33110=CARTESIAN_POINT('Ctrl Pts',(7.5026213962341,0.0888326055820073,8.95076665194336));
#33111=CARTESIAN_POINT('Ctrl Pts',(7.90993340292647,1.33146376967423,8.23767329344583));
#33112=CARTESIAN_POINT('Ctrl Pts',(8.36366914404328,3.77129773120352,6.83752858295973));
#33113=CARTESIAN_POINT('Ctrl Pts',(8.04570407182389,6.05534494010548,5.51178592094237));
#33114=CARTESIAN_POINT('Ctrl Pts',(7.5026213962341,7.70717500113854,4.55231461909006));
#33115=CARTESIAN_POINT('Ctrl Pts',(7.65938992538726,2.4980018054066E-15,
8.88427911751642));
#33116=CARTESIAN_POINT('Ctrl Pts',(8.07326695551249,1.25145701256744,8.16826019232316));
#33117=CARTESIAN_POINT('Ctrl Pts',(8.53933855650593,3.72022682808205,6.75565640073981));
#33118=CARTESIAN_POINT('Ctrl Pts',(8.21122596555418,6.03291929662566,5.40985169479934));
#33119=CARTESIAN_POINT('Ctrl Pts',(7.65938992538726,7.69401141008081,4.4421395587582));
#33120=CARTESIAN_POINT('',(7.65938992538726,7.69401141008081,4.4421395587582));
#33121=CARTESIAN_POINT('Ctrl Pts',(8.2352995588869,5.35220883425915,5.8047858408404));
#33122=CARTESIAN_POINT('Ctrl Pts',(8.12981699914252,6.07857291110272,5.38302716017364));
#33123=CARTESIAN_POINT('Ctrl Pts',(7.94257793183433,6.84158182974382,4.93874443896362));
#33124=CARTESIAN_POINT('Ctrl Pts',(7.65938992538726,7.69401141008081,4.4421395587582));
#33125=CARTESIAN_POINT('',(7.1980528062909,7.70555136271414,4.78880215351652));
#33126=CARTESIAN_POINT('Ctrl Pts',(7.1980528062909,7.70555136271414,4.78880215351652));
#33127=CARTESIAN_POINT('Ctrl Pts',(7.27501095230305,7.70355337375233,4.73109983436028));
#33128=CARTESIAN_POINT('Ctrl Pts',(7.35194075983994,7.70159253788117,4.67335568633266));
#33129=CARTESIAN_POINT('Ctrl Pts',(7.5057189835248,7.69774589003655,4.55780213135815));
#33130=CARTESIAN_POINT('Ctrl Pts',(7.58257003626918,7.69585999385014,4.49999077482194));
#33131=CARTESIAN_POINT('Ctrl Pts',(7.65938992538726,7.69401141008081,4.4421395587582));
#33132=CARTESIAN_POINT('',(7.19805280629065,0.29444863728671,9.06760430703401));
#33133=CARTESIAN_POINT('Ctrl Pts',(7.19805611451105,7.70554822452627,4.78880396535013));
#33134=CARTESIAN_POINT('Ctrl Pts',(7.71659579227932,6.08565785082646,5.7240481086634));
#33135=CARTESIAN_POINT('Ctrl Pts',(8.009965927807,3.87293458424719,7.00156448226508));
#33136=CARTESIAN_POINT('Ctrl Pts',(7.58605957246042,1.50702556652582,8.36752269052469));
#33137=CARTESIAN_POINT('Ctrl Pts',(7.19805432694391,0.294451576737634,9.06760260994123));
#33138=CARTESIAN_POINT('',(7.65938992538726,2.51671144589255E-15,8.88427911751642));
#33139=CARTESIAN_POINT('Ctrl Pts',(7.65938992538726,2.51671144589255E-15,
8.88427911751642));
#33140=CARTESIAN_POINT('Ctrl Pts',(7.58256899052649,0.04917700029988,8.91480606160851));
#33141=CARTESIAN_POINT('Ctrl Pts',(7.50571689117296,0.0983008235915428,
8.94534538978223));
#33142=CARTESIAN_POINT('Ctrl Pts',(7.35193866587405,0.196449810832569,9.00645346266353));
#33143=CARTESIAN_POINT('Ctrl Pts',(7.27500990494312,0.245476624013931,9.03702325445621));
#33144=CARTESIAN_POINT('Ctrl Pts',(7.1980528062913,0.294448637287157,9.06760430703376));
#33145=CARTESIAN_POINT('Ctrl Pts',(7.65938992538726,2.4980018054066E-15,
8.88427911751642));
#33146=CARTESIAN_POINT('Ctrl Pts',(7.94257793183434,0.856287232069759,8.39435588610997));
#33147=CARTESIAN_POINT('Ctrl Pts',(8.12551492847749,1.62202366451198,7.95622077152865));
#33148=CARTESIAN_POINT('Ctrl Pts',(8.23006777285462,2.34998381316211,7.53836899138512));
#33149=CARTESIAN_POINT('Ctrl Pts',(7.18908433792779,8.,4.31107698104349));
#33150=CARTESIAN_POINT('Ctrl Pts',(7.71466028436332,8.,2.42509771409394));
#33151=CARTESIAN_POINT('Ctrl Pts',(8.01268601649393,8.,-0.14606847802148));
#33152=CARTESIAN_POINT('Ctrl Pts',(7.58326629775444,8.,-2.89659253083151));
#33153=CARTESIAN_POINT('Ctrl Pts',(7.1890843379278,8.,-4.31107698104348));
#33154=CARTESIAN_POINT('Ctrl Pts',(7.34585286708095,7.89800380336027,4.35476450694839));
#33155=CARTESIAN_POINT('Ctrl Pts',(7.88018217809362,7.90050954890513,2.45664365021571));
#33156=CARTESIAN_POINT('Ctrl Pts',(8.18834927452041,7.90355897903611,-0.149358354443887));
#33157=CARTESIAN_POINT('Ctrl Pts',(7.74659985034045,7.89988311251891,-2.93117386439906));
#33158=CARTESIAN_POINT('Ctrl Pts',(7.34585286708095,7.89800380336027,-4.35476450694839));
#33159=CARTESIAN_POINT('Ctrl Pts',(7.5026213962341,7.79600760672054,4.3984520328533));
#33160=CARTESIAN_POINT('Ctrl Pts',(8.04570407182393,7.80101909781026,2.48818958633749));
#33161=CARTESIAN_POINT('Ctrl Pts',(8.36401253254689,7.80711795807222,-0.152648230866291));
#33162=CARTESIAN_POINT('Ctrl Pts',(7.90993340292645,7.79976622503781,-2.96575519796661));
#33163=CARTESIAN_POINT('Ctrl Pts',(7.50262139623411,7.79600760672054,-4.3984520328533));
#33164=CARTESIAN_POINT('Ctrl Pts',(7.65938992538726,7.69401141008081,4.44213955875821));
#33165=CARTESIAN_POINT('Ctrl Pts',(8.21122596555423,7.70152864671539,2.51973552245926));
#33166=CARTESIAN_POINT('Ctrl Pts',(8.53967579057337,7.71067693710833,-0.155938107288697));
#33167=CARTESIAN_POINT('Ctrl Pts',(8.07326695551245,7.69964933755672,-3.00033653153417));
#33168=CARTESIAN_POINT('Ctrl Pts',(7.65938992538726,7.69401141008081,-4.44213955875822));
#33169=CARTESIAN_POINT('',(7.65938992538726,7.69401141008081,-4.44213955875821));
#33170=CARTESIAN_POINT('Ctrl Pts',(8.23018478415036,7.70340868728783,-1.73401135132057));
#33171=CARTESIAN_POINT('Ctrl Pts',(8.12558259310879,7.7012998264511,-2.57338080520911));
#33172=CARTESIAN_POINT('Ctrl Pts',(7.94257793183433,7.69786906181353,-3.45561144714637));
#33173=CARTESIAN_POINT('Ctrl Pts',(7.65938992538726,7.69401141008081,-4.44213955875822));
#33174=CARTESIAN_POINT('',(7.1980528062909,8.,-4.27880215351799));
#33175=CARTESIAN_POINT('Ctrl Pts',(7.1980528062909,8.,-4.27880215351799));
#33176=CARTESIAN_POINT('Ctrl Pts',(7.27501095230391,7.94902933127194,-4.305923003899));
#33177=CARTESIAN_POINT('Ctrl Pts',(7.35194075984025,7.89804101422492,-4.33309694423554));
#33178=CARTESIAN_POINT('Ctrl Pts',(7.50571898351011,7.79604537620704,-4.38754242696464));
#33179=CARTESIAN_POINT('Ctrl Pts',(7.58257003626179,7.7450363247214,-4.41481487122897));
#33180=CARTESIAN_POINT('Ctrl Pts',(7.65938992538726,7.69401141008081,-4.44213955875821));
#33181=CARTESIAN_POINT('',(7.19805280629065,8.,4.27880215351701));
#33182=CARTESIAN_POINT('Ctrl Pts',(7.19805435334672,8.,-4.27879875406529));
#33183=CARTESIAN_POINT('Ctrl Pts',(7.58606188694604,8.,-2.87863845879425));
#33184=CARTESIAN_POINT('Ctrl Pts',(8.01031931069726,8.,-0.146652009457745));
#33185=CARTESIAN_POINT('Ctrl Pts',(7.71659810676505,8.,2.4083107049283));
#33186=CARTESIAN_POINT('Ctrl Pts',(7.19805613432617,8.,4.27879853380268));
#33187=CARTESIAN_POINT('Ctrl Pts',(7.65938992538726,7.69401141008081,4.44213955875821));
#33188=CARTESIAN_POINT('Ctrl Pts',(7.58256899052929,7.74503701931255,4.41481449926364));
#33189=CARTESIAN_POINT('Ctrl Pts',(7.50571689117867,7.79604676496941,4.38754168444993));
#33190=CARTESIAN_POINT('Ctrl Pts',(7.35193866587471,7.89804240208479,4.33309620458235));
#33191=CARTESIAN_POINT('Ctrl Pts',(7.27500990494514,7.94903002495543,4.30592263479751));
#33192=CARTESIAN_POINT('Ctrl Pts',(7.1980528062913,8.,4.27880215351649));
#33193=CARTESIAN_POINT('Ctrl Pts',(7.65938992538726,7.69401141008081,4.44213955875821));
#33194=CARTESIAN_POINT('Ctrl Pts',(7.94257793183433,7.69786906181355,3.45561144714631));
#33195=CARTESIAN_POINT('Ctrl Pts',(8.129867747616,7.70112374147377,2.57269689084528));
#33196=CARTESIAN_POINT('Ctrl Pts',(8.23539599829409,7.70319454879578,1.73277853167637));
#33197=CARTESIAN_POINT('Origin',(7.68856688596016,0.,0.));
#33198=CARTESIAN_POINT('Origin',(7.68856688596016,0.,0.));
#33199=CARTESIAN_POINT('Ctrl Pts',(7.65938992538726,7.69401141008081,-4.44213955875821));
#33200=CARTESIAN_POINT('Ctrl Pts',(7.94257793183433,6.84158182974378,-4.93874443896366));
#33201=CARTESIAN_POINT('Ctrl Pts',(8.12551492847749,6.07927747400524,-5.38282408477123));
#33202=CARTESIAN_POINT('Ctrl Pts',(8.23006777285462,5.35342714305933,-5.80433017637318));
#33203=CARTESIAN_POINT('Origin',(7.68856688596016,0.,0.));
#33204=CARTESIAN_POINT('',(7.65938992538726,-5.37411354087801E-15,-8.88427911751642));
#33205=CARTESIAN_POINT('Ctrl Pts',(7.65938992538726,-6.93889390390723E-15,
-8.88427911751642));
#33206=CARTESIAN_POINT('Ctrl Pts',(7.94257793183433,-0.856287232069766,
-8.39435588610997));
#33207=CARTESIAN_POINT('Ctrl Pts',(8.12551492847749,-1.62202366451198,-7.95622077152864));
#33208=CARTESIAN_POINT('Ctrl Pts',(8.23006777285462,-2.34998381316212,-7.53836899138511));
#33209=CARTESIAN_POINT('Ctrl Pts',(8.2352995588869,2.35098758456643,-7.53754173724812));
#33210=CARTESIAN_POINT('Ctrl Pts',(8.12981699914252,1.62255181442061,-7.9557121398577));
#33211=CARTESIAN_POINT('Ctrl Pts',(7.94257793183433,0.85628723206971,-8.39435588610998));
#33212=CARTESIAN_POINT('Ctrl Pts',(7.65938992538726,-3.05311331771918E-15,
-8.88427911751642));
#33213=CARTESIAN_POINT('Origin',(7.68856688596016,0.,0.));
#33214=CARTESIAN_POINT('',(7.65938992538726,-7.69401141008081,-4.44213955875821));
#33215=CARTESIAN_POINT('Ctrl Pts',(7.65938992538726,-7.69401141008081,-4.44213955875821));
#33216=CARTESIAN_POINT('Ctrl Pts',(7.94257793183434,-7.69786906181355,-3.45561144714631));
#33217=CARTESIAN_POINT('Ctrl Pts',(8.12558259310879,-7.70129982645112,-2.57338080520902));
#33218=CARTESIAN_POINT('Ctrl Pts',(8.23018478415036,-7.70340868728785,-1.73401135132049));
#33219=CARTESIAN_POINT('Ctrl Pts',(8.2352995588869,-5.35220883425914,-5.8047858408404));
#33220=CARTESIAN_POINT('Ctrl Pts',(8.12981699914252,-6.07857291110272,-5.38302716017364));
#33221=CARTESIAN_POINT('Ctrl Pts',(7.94257793183433,-6.84158182974382,-4.93874443896362));
#33222=CARTESIAN_POINT('Ctrl Pts',(7.65938992538726,-7.69401141008081,-4.44213955875821));
#33223=CARTESIAN_POINT('Origin',(7.68856688596016,0.,0.));
#33224=CARTESIAN_POINT('',(7.65938992538726,-7.69401141008081,4.44213955875821));
#33225=CARTESIAN_POINT('Ctrl Pts',(7.65938992538726,-7.69401141008081,4.44213955875821));
#33226=CARTESIAN_POINT('Ctrl Pts',(7.94257793183433,-6.84158182974379,4.93874443896366));
#33227=CARTESIAN_POINT('Ctrl Pts',(8.12981699914252,-6.07857291110267,5.38302716017369));
#33228=CARTESIAN_POINT('Ctrl Pts',(8.2352995588869,-5.3522088342591,5.80478584084045));
#33229=CARTESIAN_POINT('Ctrl Pts',(8.23539599829409,-7.70319454879577,1.73277853167643));
#33230=CARTESIAN_POINT('Ctrl Pts',(8.12986774761599,-7.70112374147376,2.57269689084535));
#33231=CARTESIAN_POINT('Ctrl Pts',(7.94257793183433,-7.69786906181353,3.45561144714636));
#33232=CARTESIAN_POINT('Ctrl Pts',(7.65938992538726,-7.69401141008081,4.44213955875821));
#33233=CARTESIAN_POINT('Origin',(7.68856688596016,0.,0.));
#33234=CARTESIAN_POINT('Ctrl Pts',(8.23006777285462,-2.34998381316205,7.53836899138514));
#33235=CARTESIAN_POINT('Ctrl Pts',(8.12551492847749,-1.62202366451191,7.95622077152867));
#33236=CARTESIAN_POINT('Ctrl Pts',(7.94257793183433,-0.856287232069709,
8.39435588610998));
#33237=CARTESIAN_POINT('Ctrl Pts',(7.65938992538726,5.55111512312578E-15,
8.88427911751642));
#33238=CARTESIAN_POINT('Ctrl Pts',(7.18908433792779,7.73350218325398,-4.77266473975377));
#33239=CARTESIAN_POINT('Ctrl Pts',(7.58326629775444,6.50852271611219,-5.47990696485985));
#33240=CARTESIAN_POINT('Ctrl Pts',(8.01233031911798,4.12656046255355,-6.85513351315146));
#33241=CARTESIAN_POINT('Ctrl Pts',(7.71466028436332,1.89980377293487,-8.1407520873226));
#33242=CARTESIAN_POINT('Ctrl Pts',(7.1890843379278,0.266497816746022,-9.08374172079725));
#33243=CARTESIAN_POINT('Ctrl Pts',(7.34585286708095,7.72033859219626,-4.66248967942192));
#33244=CARTESIAN_POINT('Ctrl Pts',(7.74659985034045,6.48841258573789,-5.37591253016962));
#33245=CARTESIAN_POINT('Ctrl Pts',(8.18799973158063,4.08119252444856,-6.76996872254409));
#33246=CARTESIAN_POINT('Ctrl Pts',(7.88018217809361,1.82273896531981,-8.07036379730134));
#33247=CARTESIAN_POINT('Ctrl Pts',(7.34585286708095,0.177665211164014,-9.0172541863703));
#33248=CARTESIAN_POINT('Ctrl Pts',(7.5026213962341,7.70717500113853,-4.55231461909007));
#33249=CARTESIAN_POINT('Ctrl Pts',(7.90993340292647,6.4683024553636,-5.2719180954794));
#33250=CARTESIAN_POINT('Ctrl Pts',(8.36366914404328,4.03582458634359,-6.68480393193673));
#33251=CARTESIAN_POINT('Ctrl Pts',(8.0457040718239,1.74567415770476,-7.99997550728009));
#33252=CARTESIAN_POINT('Ctrl Pts',(7.50262139623411,0.0888326055820055,
-8.95076665194336));
#33253=CARTESIAN_POINT('Ctrl Pts',(7.65938992538726,7.69401141008081,-4.44213955875821));
#33254=CARTESIAN_POINT('Ctrl Pts',(8.07326695551249,6.4481923249893,-5.16792366078917));
#33255=CARTESIAN_POINT('Ctrl Pts',(8.53933855650593,3.9904566482386,-6.59963914132936));
#33256=CARTESIAN_POINT('Ctrl Pts',(8.21122596555418,1.66860935008971,-7.92958721725884));
#33257=CARTESIAN_POINT('Ctrl Pts',(7.65938992538726,-3.05311331771918E-15,
-8.88427911751642));
#33258=CARTESIAN_POINT('',(7.1980528062909,0.294448637285861,-9.0676043070345));
#33259=CARTESIAN_POINT('Ctrl Pts',(7.1980528062909,0.29444863728586,-9.0676043070345));
#33260=CARTESIAN_POINT('Ctrl Pts',(7.27501095230383,0.245475957519695,-9.03702283825866));
#33261=CARTESIAN_POINT('Ctrl Pts',(7.35194075984032,0.196448476343717,-9.00645263056793));
#33262=CARTESIAN_POINT('Ctrl Pts',(7.5057189835217,0.0982994861627256,-8.94534455832922));
#33263=CARTESIAN_POINT('Ctrl Pts',(7.58257003626746,0.0491763308674533,
-8.91480564605423));
#33264=CARTESIAN_POINT('Ctrl Pts',(7.65938992538726,-1.42870104749273E-15,
-8.88427911751642));
#33265=CARTESIAN_POINT('',(7.19805280629066,7.70555136271329,-4.78880215351701));
#33266=CARTESIAN_POINT('Ctrl Pts',(7.19805611451105,0.294451775473735,-9.06760249520089));
#33267=CARTESIAN_POINT('Ctrl Pts',(7.71659579227932,1.91434214917355,-8.13235835188762));
#33268=CARTESIAN_POINT('Ctrl Pts',(8.009965927807,4.12706541575281,-6.85484197828594));
#33269=CARTESIAN_POINT('Ctrl Pts',(7.58605957246042,6.49297443347419,-5.48888377002634));
#33270=CARTESIAN_POINT('Ctrl Pts',(7.19805432694391,7.70554842326237,-4.78880385060979));
#33271=CARTESIAN_POINT('Ctrl Pts',(7.65938992538726,7.69401141008081,-4.44213955875821));
#33272=CARTESIAN_POINT('Ctrl Pts',(7.58256899052918,7.69586001901446,-4.49999156234384));
#33273=CARTESIAN_POINT('Ctrl Pts',(7.50571689117887,7.6977459413815,-4.55780370532989));
#33274=CARTESIAN_POINT('Ctrl Pts',(7.35193866587394,7.70159259125265,-4.6733572580815));
#33275=CARTESIAN_POINT('Ctrl Pts',(7.27500990494294,7.70355340094283,-4.73110061965955));
#33276=CARTESIAN_POINT('Ctrl Pts',(7.1980528062913,7.70555136271284,-4.78880215351727));
#33277=CARTESIAN_POINT('Origin',(8.4,0.,0.));
#33278=CARTESIAN_POINT('',(8.4,-5.37,6.57635331142129E-16));
#33279=CARTESIAN_POINT('Origin',(8.4,0.,0.));
#33280=CARTESIAN_POINT('Origin',(7.1980528062909,8.,-4.27880215351799));
#33281=CARTESIAN_POINT('',(7.19805280629066,8.,-4.27880215351701));
#33282=CARTESIAN_POINT('Origin',(7.65938992538726,-5.37411354087801E-15,
-8.88427911751642));
#33283=CARTESIAN_POINT('',(7.19805280629066,-0.294448637286711,-9.06760430703401));
#33284=CARTESIAN_POINT('Ctrl Pts',(7.65938992538726,-7.34681978757065E-15,
-8.88427911751642));
#33285=CARTESIAN_POINT('Ctrl Pts',(7.58256899052983,-0.0491770002977431,
-8.91480606160718));
#33286=CARTESIAN_POINT('Ctrl Pts',(7.50571689118011,-0.0983008235869914,
-8.94534538977939));
#33287=CARTESIAN_POINT('Ctrl Pts',(7.35193866587446,-0.196449810832315,
-9.00645346266337));
#33288=CARTESIAN_POINT('Ctrl Pts',(7.27500990494381,-0.245476624013499,
-9.03702325445593));
#33289=CARTESIAN_POINT('Ctrl Pts',(7.1980528062913,-0.294448637287159,-9.06760430703376));
#33290=CARTESIAN_POINT('',(7.19805280629066,0.294448637286708,-9.06760430703401));
#33291=CARTESIAN_POINT('Origin',(7.1980528062909,7.70555136271414,4.78880215351652));
#33292=CARTESIAN_POINT('',(7.19805280629066,7.70555136271329,4.78880215351701));
#33293=CARTESIAN_POINT('Origin',(7.65938992538726,-7.69401141008081,-4.44213955875821));
#33294=CARTESIAN_POINT('',(7.1980528062909,-7.70555136271414,-4.78880215351652));
#33295=CARTESIAN_POINT('Ctrl Pts',(7.1980528062909,-7.70555136271414,-4.78880215351652));
#33296=CARTESIAN_POINT('Ctrl Pts',(7.27501095229772,-7.70355337375246,-4.73109983436428));
#33297=CARTESIAN_POINT('Ctrl Pts',(7.35194075983702,-7.70159253788124,-4.67335568633486));
#33298=CARTESIAN_POINT('Ctrl Pts',(7.50571898352358,-7.69774589003658,-4.55780213135908));
#33299=CARTESIAN_POINT('Ctrl Pts',(7.58257003626834,-7.69585999385016,-4.49999077482257));
#33300=CARTESIAN_POINT('Ctrl Pts',(7.65938992538726,-7.69401141008081,-4.44213955875821));
#33301=CARTESIAN_POINT('',(7.19805280629065,-8.,-4.27880215351701));
#33302=CARTESIAN_POINT('Ctrl Pts',(7.65938992538726,-7.69401141008081,-4.44213955875821));
#33303=CARTESIAN_POINT('Ctrl Pts',(7.58256899053098,-7.74503701931143,-4.41481449926424));
#33304=CARTESIAN_POINT('Ctrl Pts',(7.50571689118228,-7.79604676496702,-4.3875416844512));
#33305=CARTESIAN_POINT('Ctrl Pts',(7.35193866587007,-7.89804240208786,-4.3330962045807));
#33306=CARTESIAN_POINT('Ctrl Pts',(7.27500990493544,-7.94903002496185,-4.30592263479409));
#33307=CARTESIAN_POINT('Ctrl Pts',(7.1980528062913,-8.,-4.27880215351649));
#33308=CARTESIAN_POINT('',(7.19805280629066,-7.70555136271329,-4.78880215351701));
#33309=CARTESIAN_POINT('Origin',(7.1980528062909,-0.294448637285862,9.0676043070345));
#33310=CARTESIAN_POINT('',(7.1980528062909,-0.294448637285862,9.0676043070345));
#33311=CARTESIAN_POINT('',(7.19805280629066,-0.294448637286709,9.06760430703401));
#33312=CARTESIAN_POINT('Ctrl Pts',(7.1980528062909,-0.294448637285858,9.0676043070345));
#33313=CARTESIAN_POINT('Ctrl Pts',(7.27501095230018,-0.245475957522012,
9.03702283826011));
#33314=CARTESIAN_POINT('Ctrl Pts',(7.35194075983832,-0.196448476344994,
9.00645263056873));
#33315=CARTESIAN_POINT('Ctrl Pts',(7.50571898351829,-0.0982994861648936,
8.94534455833057));
#33316=CARTESIAN_POINT('Ctrl Pts',(7.58257003626595,-0.0491763308684156,
8.91480564605483));
#33317=CARTESIAN_POINT('Ctrl Pts',(7.65938992538726,6.46212393927782E-15,
8.88427911751642));
#33318=CARTESIAN_POINT('Origin',(7.65938992538726,-7.69401141008081,4.44213955875821));
#33319=CARTESIAN_POINT('',(7.19805280629089,-8.,4.27880215351799));
#33320=CARTESIAN_POINT('Ctrl Pts',(7.1980528062909,-8.,4.27880215351798));
#33321=CARTESIAN_POINT('Ctrl Pts',(7.27501095230383,-7.949029331272,4.30592300389896));
#33322=CARTESIAN_POINT('Ctrl Pts',(7.35194075984076,-7.89804101422459,4.33309694423571));
#33323=CARTESIAN_POINT('Ctrl Pts',(7.50571898352634,-7.79604537619627,4.38754242697037));
#33324=CARTESIAN_POINT('Ctrl Pts',(7.58257003626946,-7.7450363247163,4.4148148712317));
#33325=CARTESIAN_POINT('Ctrl Pts',(7.65938992538726,-7.69401141008081,4.44213955875821));
#33326=CARTESIAN_POINT('',(7.19805280629065,-7.70555136271329,4.78880215351701));
#33327=CARTESIAN_POINT('Ctrl Pts',(7.65938992538726,-7.69401141008081,4.44213955875821));
#33328=CARTESIAN_POINT('Ctrl Pts',(7.58256899052981,-7.69586001901445,4.49999156234336));
#33329=CARTESIAN_POINT('Ctrl Pts',(7.50571689117983,-7.69774594138148,4.55780370532917));
#33330=CARTESIAN_POINT('Ctrl Pts',(7.35193866587556,-7.70159259125261,4.67335725808028));
#33331=CARTESIAN_POINT('Ctrl Pts',(7.2750099049467,-7.70355340094273,4.73110061965673));
#33332=CARTESIAN_POINT('Ctrl Pts',(7.1980528062913,-7.70555136271284,4.78880215351727));
#33333=CARTESIAN_POINT('',(7.19805280629067,-8.,4.27880215351701));
#33334=CARTESIAN_POINT('Ctrl Pts',(7.18908433792779,-7.73350218325399,4.77266473975376));
#33335=CARTESIAN_POINT('Ctrl Pts',(7.71466028436332,-6.10019622706492,5.71565437322854));
#33336=CARTESIAN_POINT('Ctrl Pts',(8.01233031911798,-3.87343953744612,7.00127294739976));
#33337=CARTESIAN_POINT('Ctrl Pts',(7.58326629775444,-1.49147728388766,8.37649949569126));
#33338=CARTESIAN_POINT('Ctrl Pts',(7.1890843379278,-0.266497816746021,9.08374172079725));
#33339=CARTESIAN_POINT('Ctrl Pts',(7.34585286708095,-7.72033859219626,4.66248967942191));
#33340=CARTESIAN_POINT('Ctrl Pts',(7.88018217809362,-6.0777705835851,5.61372014708552));
#33341=CARTESIAN_POINT('Ctrl Pts',(8.18799973158063,-3.82236863432465,6.91940076517984));
#33342=CARTESIAN_POINT('Ctrl Pts',(7.74659985034044,-1.41147052678086,8.30708639456859));
#33343=CARTESIAN_POINT('Ctrl Pts',(7.34585286708095,-0.177665211164012,
9.01725418637031));
#33344=CARTESIAN_POINT('Ctrl Pts',(7.5026213962341,-7.70717500113854,4.55231461909006));
#33345=CARTESIAN_POINT('Ctrl Pts',(8.04570407182393,-6.05534494010528,5.5117859209425));
#33346=CARTESIAN_POINT('Ctrl Pts',(8.36366914404327,-3.77129773120317,6.83752858295992));
#33347=CARTESIAN_POINT('Ctrl Pts',(7.90993340292645,-1.33146376967407,8.23767329344591));
#33348=CARTESIAN_POINT('Ctrl Pts',(7.5026213962341,-0.0888326055820031,
8.95076665194336));
#33349=CARTESIAN_POINT('Ctrl Pts',(7.65938992538726,-7.69401141008081,4.44213955875821));
#33350=CARTESIAN_POINT('Ctrl Pts',(8.21122596555423,-6.03291929662547,5.40985169479948));
#33351=CARTESIAN_POINT('Ctrl Pts',(8.53933855650592,-3.7202268280817,6.75565640074));
#33352=CARTESIAN_POINT('Ctrl Pts',(8.07326695551245,-1.25145701256728,8.16826019232323));
#33353=CARTESIAN_POINT('Ctrl Pts',(7.65938992538726,5.55111512312578E-15,
8.88427911751642));
#33354=CARTESIAN_POINT('Ctrl Pts',(7.19805432694369,-0.294451576736895,
9.06760260994166));
#33355=CARTESIAN_POINT('Ctrl Pts',(7.58605957246035,-1.50702556652525,8.36752269052502));
#33356=CARTESIAN_POINT('Ctrl Pts',(8.00996592780699,-3.87293458424645,7.00156448226551));
#33357=CARTESIAN_POINT('Ctrl Pts',(7.71659579227937,-6.08565785082586,5.72404810866374));
#33358=CARTESIAN_POINT('Ctrl Pts',(7.19805611451127,-7.70554822452553,4.78880396535056));
#33359=CARTESIAN_POINT('Origin',(0.,-7.85277568135665,4.53380215351701));
#33360=CARTESIAN_POINT('',(0.849339335588243,-7.70555136271329,4.78880215351701));
#33361=CARTESIAN_POINT('',(0.849339335588256,-8.,4.27880215351701));
#33362=CARTESIAN_POINT('Ctrl Pts',(0.849339335588243,-7.70555136271329,
4.78880215351701));
#33363=CARTESIAN_POINT('Ctrl Pts',(0.843815452152285,-7.85277568135665,
4.53380215351701));
#33364=CARTESIAN_POINT('Ctrl Pts',(0.849339335588256,-8.,4.27880215351701));
#33365=CARTESIAN_POINT('',(0.,-8.,4.27880215351701));
#33366=CARTESIAN_POINT('',(0.,-7.70555136271329,4.78880215351701));
#33367=CARTESIAN_POINT('Ctrl Pts',(7.18908433792779,-8.,-4.31107698104349));
#33368=CARTESIAN_POINT('Ctrl Pts',(7.58326629775444,-8.,-2.89659253083133));
#33369=CARTESIAN_POINT('Ctrl Pts',(8.01268601649393,-8.,-0.14606847802109));
#33370=CARTESIAN_POINT('Ctrl Pts',(7.71466028436332,-8.,2.42509771409418));
#33371=CARTESIAN_POINT('Ctrl Pts',(7.1890843379278,-8.,4.31107698104348));
#33372=CARTESIAN_POINT('Ctrl Pts',(7.34585286708095,-7.89800380336027,-4.3547645069484));
#33373=CARTESIAN_POINT('Ctrl Pts',(7.74659985034045,-7.89988311251892,-2.93117386439888));
#33374=CARTESIAN_POINT('Ctrl Pts',(8.18834927452041,-7.90355897903611,-0.149358354443497));
#33375=CARTESIAN_POINT('Ctrl Pts',(7.88018217809361,-7.90050954890512,2.45664365021595));
#33376=CARTESIAN_POINT('Ctrl Pts',(7.34585286708096,-7.89800380336027,4.35476450694839));
#33377=CARTESIAN_POINT('Ctrl Pts',(7.5026213962341,-7.79600760672054,-4.3984520328533));
#33378=CARTESIAN_POINT('Ctrl Pts',(7.90993340292647,-7.79976622503783,-2.96575519796644));
#33379=CARTESIAN_POINT('Ctrl Pts',(8.36401253254689,-7.80711795807223,-0.152648230865896));
#33380=CARTESIAN_POINT('Ctrl Pts',(8.04570407182389,-7.80101909781024,2.48818958633772));
#33381=CARTESIAN_POINT('Ctrl Pts',(7.50262139623411,-7.79600760672054,4.3984520328533));
#33382=CARTESIAN_POINT('Ctrl Pts',(7.65938992538726,-7.69401141008081,-4.44213955875821));
#33383=CARTESIAN_POINT('Ctrl Pts',(8.07326695551249,-7.69964933755674,-3.000336531534));
#33384=CARTESIAN_POINT('Ctrl Pts',(8.53967579057338,-7.71067693710834,-0.155938107288303));
#33385=CARTESIAN_POINT('Ctrl Pts',(8.21122596555418,-7.70152864671536,2.51973552245949));
#33386=CARTESIAN_POINT('Ctrl Pts',(7.65938992538726,-7.69401141008081,4.44213955875821));
#33387=CARTESIAN_POINT('Ctrl Pts',(7.19805613432595,-8.,4.27879853380353));
#33388=CARTESIAN_POINT('Ctrl Pts',(7.716598106765,-8.,2.40831070492898));
#33389=CARTESIAN_POINT('Ctrl Pts',(8.01031931069726,-8.,-0.146652009456896));
#33390=CARTESIAN_POINT('Ctrl Pts',(7.5860618869461,-8.,-2.87863845879359));
#33391=CARTESIAN_POINT('Ctrl Pts',(7.19805435334694,-8.,-4.27879875406444));
#33392=CARTESIAN_POINT('Origin',(0.,7.63278329429795E-16,9.06760430703401));
#33393=CARTESIAN_POINT('',(0.849339335588243,0.294448637286709,9.06760430703401));
#33394=CARTESIAN_POINT('',(0.849339335588255,-0.294448637286709,9.06760430703401));
#33395=CARTESIAN_POINT('Ctrl Pts',(0.849339335588243,0.294448637286709,
9.06760430703401));
#33396=CARTESIAN_POINT('Ctrl Pts',(0.843815452152285,-2.77555756156289E-16,
9.06760430703401));
#33397=CARTESIAN_POINT('Ctrl Pts',(0.849339335588255,-0.294448637286709,
9.06760430703402));
#33398=CARTESIAN_POINT('',(0.,-0.294448637286709,9.06760430703401));
#33399=CARTESIAN_POINT('',(0.,0.29444863728671,9.06760430703401));
#33400=CARTESIAN_POINT('Origin',(0.,-7.85277568135665,-4.53380215351701));
#33401=CARTESIAN_POINT('',(0.849339335588243,-8.,-4.27880215351701));
#33402=CARTESIAN_POINT('',(0.849339335588255,-7.70555136271329,-4.78880215351701));
#33403=CARTESIAN_POINT('Ctrl Pts',(0.849339335588243,-8.,-4.27880215351701));
#33404=CARTESIAN_POINT('Ctrl Pts',(0.843815452152285,-7.85277568135665,
-4.53380215351701));
#33405=CARTESIAN_POINT('Ctrl Pts',(0.849339335588255,-7.70555136271329,
-4.78880215351701));
#33406=CARTESIAN_POINT('',(0.,-7.70555136271329,-4.78880215351701));
#33407=CARTESIAN_POINT('',(0.,-8.,-4.27880215351701));
#33408=CARTESIAN_POINT('Ctrl Pts',(7.18908433792779,-0.266497816746021,
-9.08374172079725));
#33409=CARTESIAN_POINT('Ctrl Pts',(7.58326629775444,-1.49147728388782,-8.37649949569117));
#33410=CARTESIAN_POINT('Ctrl Pts',(8.01233031911798,-3.87343953744646,-7.00127294739956));
#33411=CARTESIAN_POINT('Ctrl Pts',(7.71466028436332,-6.10019622706513,-5.71565437322842));
#33412=CARTESIAN_POINT('Ctrl Pts',(7.1890843379278,-7.73350218325398,-4.77266473975377));
#33413=CARTESIAN_POINT('Ctrl Pts',(7.34585286708095,-0.177665211164016,
-9.01725418637031));
#33414=CARTESIAN_POINT('Ctrl Pts',(7.74659985034045,-1.41147052678103,-8.3070863945685));
#33415=CARTESIAN_POINT('Ctrl Pts',(8.18799973158063,-3.82236863432499,-6.91940076517965));
#33416=CARTESIAN_POINT('Ctrl Pts',(7.88018217809361,-6.0777705835853,-5.6137201470854));
#33417=CARTESIAN_POINT('Ctrl Pts',(7.34585286708095,-7.72033859219626,-4.66248967942192));
#33418=CARTESIAN_POINT('Ctrl Pts',(7.5026213962341,-0.0888326055820114,
-8.95076665194336));
#33419=CARTESIAN_POINT('Ctrl Pts',(7.90993340292647,-1.33146376967424,-8.23767329344583));
#33420=CARTESIAN_POINT('Ctrl Pts',(8.36366914404328,-3.77129773120352,-6.83752858295973));
#33421=CARTESIAN_POINT('Ctrl Pts',(8.0457040718239,-6.05534494010547,-5.51178592094237));
#33422=CARTESIAN_POINT('Ctrl Pts',(7.50262139623411,-7.70717500113853,-4.55231461909006));
#33423=CARTESIAN_POINT('Ctrl Pts',(7.65938992538726,-6.93889390390723E-15,
-8.88427911751642));
#33424=CARTESIAN_POINT('Ctrl Pts',(8.07326695551249,-1.25145701256745,-8.16826019232316));
#33425=CARTESIAN_POINT('Ctrl Pts',(8.53933855650593,-3.72022682808205,-6.75565640073981));
#33426=CARTESIAN_POINT('Ctrl Pts',(8.21122596555418,-6.03291929662565,-5.40985169479935));
#33427=CARTESIAN_POINT('Ctrl Pts',(7.65938992538726,-7.69401141008081,-4.44213955875821));
#33428=CARTESIAN_POINT('Ctrl Pts',(7.19805611451105,-7.70554822452627,-4.78880396535013));
#33429=CARTESIAN_POINT('Ctrl Pts',(7.71659579227932,-6.08565785082645,-5.7240481086634));
#33430=CARTESIAN_POINT('Ctrl Pts',(8.00996592780701,-3.87293458424719,-7.00156448226509));
#33431=CARTESIAN_POINT('Ctrl Pts',(7.58605957246042,-1.50702556652582,-8.36752269052469));
#33432=CARTESIAN_POINT('Ctrl Pts',(7.19805432694391,-0.294451576737634,
-9.06760260994123));
#33433=CARTESIAN_POINT('Origin',(0.,7.85277568135665,4.53380215351701));
#33434=CARTESIAN_POINT('',(0.849339335588243,8.,4.27880215351701));
#33435=CARTESIAN_POINT('',(0.849339335588254,7.70555136271329,4.78880215351701));
#33436=CARTESIAN_POINT('Ctrl Pts',(0.849339335588243,8.,4.27880215351701));
#33437=CARTESIAN_POINT('Ctrl Pts',(0.843815452152285,7.85277568135665,4.53380215351701));
#33438=CARTESIAN_POINT('Ctrl Pts',(0.849339335588254,7.70555136271329,4.78880215351701));
#33439=CARTESIAN_POINT('',(0.,7.70555136271329,4.78880215351701));
#33440=CARTESIAN_POINT('',(0.,8.,4.27880215351701));
#33441=CARTESIAN_POINT('Origin',(0.,-1.2490009027033E-15,-9.06760430703401));
#33442=CARTESIAN_POINT('',(0.849339335588244,-0.294448637286709,-9.06760430703401));
#33443=CARTESIAN_POINT('',(0.849339335588254,0.294448637286709,-9.06760430703401));
#33444=CARTESIAN_POINT('Ctrl Pts',(0.849339335588244,-0.294448637286709,
-9.06760430703401));
#33445=CARTESIAN_POINT('Ctrl Pts',(0.843815452152285,1.73472347597681E-16,
-9.06760430703401));
#33446=CARTESIAN_POINT('Ctrl Pts',(0.849339335588254,0.294448637286709,
-9.06760430703402));
#33447=CARTESIAN_POINT('',(0.,0.294448637286708,-9.06760430703401));
#33448=CARTESIAN_POINT('',(0.,-0.294448637286711,-9.06760430703401));
#33449=CARTESIAN_POINT('Origin',(0.,7.85277568135664,-4.53380215351701));
#33450=CARTESIAN_POINT('',(0.849339335588243,7.70555136271329,-4.78880215351701));
#33451=CARTESIAN_POINT('',(0.849339335588255,8.,-4.27880215351701));
#33452=CARTESIAN_POINT('Ctrl Pts',(0.849339335588243,7.70555136271329,-4.78880215351701));
#33453=CARTESIAN_POINT('Ctrl Pts',(0.843815452152285,7.85277568135665,-4.53380215351701));
#33454=CARTESIAN_POINT('Ctrl Pts',(0.849339335588255,8.,-4.27880215351701));
#33455=CARTESIAN_POINT('',(0.,8.,-4.27880215351701));
#33456=CARTESIAN_POINT('',(0.,7.70555136271329,-4.78880215351701));
#33457=CARTESIAN_POINT('Origin',(0.,8.,4.61880215351701));
#33458=CARTESIAN_POINT('Ctrl Pts',(0.849339335588254,7.70555136271329,4.78880215351701));
#33459=CARTESIAN_POINT('Ctrl Pts',(-0.317120580865619,3.99999999999977,
6.92820323027565));
#33460=CARTESIAN_POINT('Ctrl Pts',(0.849339335588243,0.294448637286709,
9.06760430703402));
#33461=CARTESIAN_POINT('Origin',(0.,8.,-4.61880215351701));
#33462=CARTESIAN_POINT('Ctrl Pts',(0.849339335588255,8.,-4.27880215351701));
#33463=CARTESIAN_POINT('Ctrl Pts',(-0.317120580865621,8.,2.63122856836162E-13));
#33464=CARTESIAN_POINT('Ctrl Pts',(0.849339335588243,8.,4.27880215351701));
#33465=CARTESIAN_POINT('Origin',(0.,-1.69692038195985E-15,-9.23760430703401));
#33466=CARTESIAN_POINT('Ctrl Pts',(0.849339335588254,0.294448637286709,
-9.06760430703402));
#33467=CARTESIAN_POINT('Ctrl Pts',(-0.317120580865621,4.00000000000023,
-6.92820323027538));
#33468=CARTESIAN_POINT('Ctrl Pts',(0.849339335588243,7.70555136271329,-4.78880215351701));
#33469=CARTESIAN_POINT('Origin',(0.711433114039842,0.,0.));
#33470=CARTESIAN_POINT('',(0.,-7.60300281800529,9.31099306497849E-16));
#33471=CARTESIAN_POINT('Origin',(0.,0.,0.));
#33472=CARTESIAN_POINT('',(0.229474401962219,-8.,-9.15987121259293E-16));
#33473=CARTESIAN_POINT('',(0.711433114039842,-8.83380215351701,-1.08182875316056E-15));
#33474=CARTESIAN_POINT('Ctrl Pts',(0.849339335588256,-8.,4.27880215351701));
#33475=CARTESIAN_POINT('Ctrl Pts',(0.229474401962242,-8.,2.00501685195949));
#33476=CARTESIAN_POINT('Ctrl Pts',(0.229474401962219,-8.,-8.52256803200703E-16));
#33477=CARTESIAN_POINT('Ctrl Pts',(0.849339335588255,-0.294448637286709,
9.06760430703402));
#33478=CARTESIAN_POINT('Ctrl Pts',(-0.31712058086562,-4.00000000000023,
6.92820323027538));
#33479=CARTESIAN_POINT('Ctrl Pts',(0.849339335588243,-7.70555136271329,
4.78880215351701));
#33480=CARTESIAN_POINT('Ctrl Pts',(0.849339335588255,-7.70555136271329,
-4.78880215351701));
#33481=CARTESIAN_POINT('Ctrl Pts',(-0.317120580865619,-3.99999999999977,
-6.92820323027564));
#33482=CARTESIAN_POINT('Ctrl Pts',(0.849339335588244,-0.294448637286708,
-9.06760430703401));
#33483=CARTESIAN_POINT('Ctrl Pts',(0.229474401962219,-8.,-8.52256803200703E-16));
#33484=CARTESIAN_POINT('Ctrl Pts',(0.229474401962195,-8.,-2.00501685195963));
#33485=CARTESIAN_POINT('Ctrl Pts',(0.849339335588243,-8.,-4.27880215351701));
#33486=CARTESIAN_POINT('Origin',(0.15,0.,0.));
#33487=CARTESIAN_POINT('',(0.,-5.37,-6.57635331142129E-16));
#33488=CARTESIAN_POINT('Origin',(0.,0.,0.));
#33489=CARTESIAN_POINT('',(0.4,-5.05,-6.18446633569413E-16));
#33490=CARTESIAN_POINT('',(0.15,-5.25,-6.42939569552361E-16));
#33491=CARTESIAN_POINT('Origin',(0.4,0.,0.));
#33492=CARTESIAN_POINT('Origin',(4.2,0.,0.));
#33493=CARTESIAN_POINT('',(8.,-5.05,-6.18446633569413E-16));
#33494=CARTESIAN_POINT('',(4.2,-5.05,-6.18446633569413E-16));
#33495=CARTESIAN_POINT('Origin',(8.,0.,0.));
#33496=CARTESIAN_POINT('Origin',(8.25,0.,0.));
#33497=CARTESIAN_POINT('',(8.25,-5.25,-6.42939569552361E-16));
#33498=CARTESIAN_POINT('Origin',(0.,-8.,-4.61880215351701));
#33499=CARTESIAN_POINT('Origin',(0.,-8.,4.61880215351701));
#33500=CARTESIAN_POINT('Origin',(0.,5.6564012731995E-16,9.23760430703401));
#33501=CARTESIAN_POINT('Origin',(0.,0.,0.));
#33502=CARTESIAN_POINT('',(0.,0.,0.));
#33503=CARTESIAN_POINT('Origin',(-79.75,0.,0.));
#33504=CARTESIAN_POINT('',(-80.,10.5,-1.28587913910472E-15));
#33505=CARTESIAN_POINT('Origin',(-80.,0.,0.));
#33506=CARTESIAN_POINT('',(-79.5,10.,1.22464679914735E-15));
#33507=CARTESIAN_POINT('',(-79.75,10.25,-1.25526296912604E-15));
#33508=CARTESIAN_POINT('',(-79.5,-10.,-1.22464679914735E-15));
#33509=CARTESIAN_POINT('Origin',(-79.5,0.,0.));
#33510=CARTESIAN_POINT('Origin',(-79.5,0.,0.));
#33511=CARTESIAN_POINT('Origin',(-80.,10.,0.));
#33512=CARTESIAN_POINT('',(-80.,-12.05,-1.47569939297256E-15));
#33513=CARTESIAN_POINT('Origin',(-80.,0.,0.));
#33514=CARTESIAN_POINT('Origin',(14.,0.,0.));
#33515=CARTESIAN_POINT('',(-61.,-10.,0.));
#33516=CARTESIAN_POINT('',(14.,-10.,-1.22464679914735E-15));
#33517=CARTESIAN_POINT('',(61.,-10.,0.));
#33518=CARTESIAN_POINT('',(14.,-10.,-1.22464679914735E-15));
#33519=CARTESIAN_POINT('',(108.,-10.,-1.22464679914735E-15));
#33520=CARTESIAN_POINT('',(14.,-10.,-1.22464679914735E-15));
#33521=CARTESIAN_POINT('Origin',(108.,0.,0.));
#33522=CARTESIAN_POINT('',(61.,10.,0.));
#33523=CARTESIAN_POINT('Origin',(61.,0.,0.));
#33524=CARTESIAN_POINT('Origin',(61.,0.,0.));
#33525=CARTESIAN_POINT('',(-61.,10.,0.));
#33526=CARTESIAN_POINT('Origin',(-61.,0.,0.));
#33527=CARTESIAN_POINT('Origin',(-61.,0.,0.));
#33528=CARTESIAN_POINT('Origin',(125.75,0.,0.));
#33529=CARTESIAN_POINT('',(126.,-11.05,-1.35323471305783E-15));
#33530=CARTESIAN_POINT('Origin',(126.,0.,0.));
#33531=CARTESIAN_POINT('',(125.5,-10.55,1.29200237310046E-15));
#33532=CARTESIAN_POINT('',(125.75,-10.8,-1.32261854307914E-15));
#33533=CARTESIAN_POINT('Origin',(125.5,0.,0.));
#33534=CARTESIAN_POINT('Origin',(126.,0.,0.));
#33535=CARTESIAN_POINT('',(126.,-15.5,4.11864858792871E-15));
#33536=CARTESIAN_POINT('Origin',(126.,0.,0.));
#33537=CARTESIAN_POINT('Origin',(117.05,0.,0.));
#33538=CARTESIAN_POINT('',(108.,-10.55,-1.29200237310046E-15));
#33539=CARTESIAN_POINT('Origin',(108.,0.,0.));
#33540=CARTESIAN_POINT('',(117.05,-10.55,-1.29200237310046E-15));
#33541=CARTESIAN_POINT('Origin',(124.5,0.,0.));
#33542=CARTESIAN_POINT('',(124.5,-17.,3.53428366433714E-16));
#33543=CARTESIAN_POINT('Origin',(124.5,0.,0.));
#33544=CARTESIAN_POINT('Origin',(124.5,-15.5,3.22243510571916E-16));
#33545=CARTESIAN_POINT('Origin',(112.75,0.,0.));
#33546=CARTESIAN_POINT('',(101.5,-17.,-2.0818995585505E-15));
#33547=CARTESIAN_POINT('',(112.75,-17.,-2.0818995585505E-15));
#33548=CARTESIAN_POINT('',(101.5,-2.0818995585505E-15,17.));
#33549=CARTESIAN_POINT('Origin',(101.5,0.,0.));
#33550=CARTESIAN_POINT('Origin',(101.5,0.,0.));
#33551=CARTESIAN_POINT('Origin',(101.5,0.,0.));
#33552=CARTESIAN_POINT('',(100.,-1.8982025386784E-15,15.5));
#33553=CARTESIAN_POINT('Origin',(101.5,-1.8982025386784E-15,15.5));
#33554=CARTESIAN_POINT('Origin',(100.,0.,0.));
#33555=CARTESIAN_POINT('Origin',(100.,17.,0.));
#33556=CARTESIAN_POINT('',(100.,-14.,-1.71450551880629E-15));
#33557=CARTESIAN_POINT('Origin',(100.,0.,0.));
#33558=CARTESIAN_POINT('Origin',(-81.5,0.,0.));
#33559=CARTESIAN_POINT('',(-80.,-1.8982025386784E-15,15.5));
#33560=CARTESIAN_POINT('Origin',(-80.,0.,0.));
#33561=CARTESIAN_POINT('',(-81.5,-2.0818995585505E-15,17.));
#33562=CARTESIAN_POINT('Origin',(-81.5,-1.8982025386784E-15,15.5));
#33563=CARTESIAN_POINT('',(-81.5,-17.,-2.0818995585505E-15));
#33564=CARTESIAN_POINT('Origin',(-81.5,0.,0.));
#33565=CARTESIAN_POINT('Origin',(-81.5,0.,0.));
#33566=CARTESIAN_POINT('Origin',(-84.75,0.,0.));
#33567=CARTESIAN_POINT('',(-88.5,-17.,0.));
#33568=CARTESIAN_POINT('',(-84.75,-17.,-2.0818995585505E-15));
#33569=CARTESIAN_POINT('Origin',(-88.5,0.,0.));
#33570=CARTESIAN_POINT('Origin',(-80.,14.,0.));
#33571=CARTESIAN_POINT('',(-80.,-14.,-1.71450551880629E-15));
#33572=CARTESIAN_POINT('Origin',(-80.,0.,0.));
#33573=CARTESIAN_POINT('Origin',(-88.5,0.,0.));
#33574=CARTESIAN_POINT('',(-90.,-15.5,-3.79640507735679E-15));
#33575=CARTESIAN_POINT('Origin',(-88.5,-15.5,0.));
#33576=CARTESIAN_POINT('Origin',(-90.,0.,0.));
#33577=CARTESIAN_POINT('Origin',(-90.,16.5,0.));
#33578=CARTESIAN_POINT('',(-90.,-12.05,-1.47569939297256E-15));
#33579=CARTESIAN_POINT('Origin',(-90.,0.,0.));
#33580=CARTESIAN_POINT('Origin',(-77.5,13.5,16.5));
#33581=CARTESIAN_POINT('',(-77.5,27.,18.));
#33582=CARTESIAN_POINT('',(-79.,27.,16.5));
#33583=CARTESIAN_POINT('Origin',(-77.5,27.,16.5));
#33584=CARTESIAN_POINT('',(-79.,-27.,16.5));
#33585=CARTESIAN_POINT('',(-79.,13.5,16.5));
#33586=CARTESIAN_POINT('',(-77.5,-27.,18.));
#33587=CARTESIAN_POINT('Origin',(-77.5,-27.,16.5));
#33588=CARTESIAN_POINT('',(-77.5,13.5,18.));
#33589=CARTESIAN_POINT('Origin',(-73.,-27.,16.5));
#33590=CARTESIAN_POINT('',(-73.,-33.,16.5));
#33591=CARTESIAN_POINT('',(-73.,-31.5,18.));
#33592=CARTESIAN_POINT('Origin',(-73.,-31.5,16.5));
#33593=CARTESIAN_POINT('Origin',(-73.,-27.,18.));
#33594=CARTESIAN_POINT('Origin',(-73.,-27.,16.5));
#33595=CARTESIAN_POINT('Origin',(-67.,-31.5,16.5));
#33596=CARTESIAN_POINT('',(-49.,-33.,16.5));
#33597=CARTESIAN_POINT('',(-49.,-31.5,18.));
#33598=CARTESIAN_POINT('Origin',(-49.,-31.5,16.5));
#33599=CARTESIAN_POINT('',(-67.,-31.5,18.));
#33600=CARTESIAN_POINT('',(-67.,-33.,16.5));
#33601=CARTESIAN_POINT('Origin',(-49.,-27.,16.5));
#33602=CARTESIAN_POINT('',(-43.,-27.,16.5));
#33603=CARTESIAN_POINT('',(-44.5,-27.,18.));
#33604=CARTESIAN_POINT('Origin',(-44.5,-27.,16.5));
#33605=CARTESIAN_POINT('Origin',(-49.,-27.,18.));
#33606=CARTESIAN_POINT('Origin',(-49.,-27.,16.5));
#33607=CARTESIAN_POINT('Origin',(-44.5,-13.5,16.5));
#33608=CARTESIAN_POINT('',(-43.,27.,16.5));
#33609=CARTESIAN_POINT('',(-44.5,27.,18.));
#33610=CARTESIAN_POINT('Origin',(-44.5,27.,16.5));
#33611=CARTESIAN_POINT('',(-44.5,-13.5,18.));
#33612=CARTESIAN_POINT('',(-43.,-13.5,16.5));
#33613=CARTESIAN_POINT('Origin',(-49.,27.,16.5));
#33614=CARTESIAN_POINT('',(-49.,33.,16.5));
#33615=CARTESIAN_POINT('',(-49.,31.5,18.));
#33616=CARTESIAN_POINT('Origin',(-49.,31.5,16.5));
#33617=CARTESIAN_POINT('Origin',(-49.,27.,18.));
#33618=CARTESIAN_POINT('Origin',(-49.,27.,16.5));
#33619=CARTESIAN_POINT('Origin',(-55.,31.5,16.5));
#33620=CARTESIAN_POINT('',(-73.,33.,16.5));
#33621=CARTESIAN_POINT('',(-73.,31.5,18.));
#33622=CARTESIAN_POINT('Origin',(-73.,31.5,16.5));
#33623=CARTESIAN_POINT('',(-55.,31.5,18.));
#33624=CARTESIAN_POINT('',(-55.,33.,16.5));
#33625=CARTESIAN_POINT('Origin',(-73.,27.,16.5));
#33626=CARTESIAN_POINT('Origin',(-73.,27.,18.));
#33627=CARTESIAN_POINT('Origin',(-73.,27.,16.5));
#33628=CARTESIAN_POINT('Origin',(-49.,-27.,-24.));
#33629=CARTESIAN_POINT('',(-49.,-33.,-22.5));
#33630=CARTESIAN_POINT('',(-49.,-33.,-24.));
#33631=CARTESIAN_POINT('',(-43.,-27.,-22.5));
#33632=CARTESIAN_POINT('Origin',(-49.,-27.,-22.5));
#33633=CARTESIAN_POINT('',(-43.,-27.,-24.));
#33634=CARTESIAN_POINT('Origin',(-73.,-33.,-24.));
#33635=CARTESIAN_POINT('',(-73.,-33.,-22.5));
#33636=CARTESIAN_POINT('',(-73.,-33.,-24.));
#33637=CARTESIAN_POINT('',(-67.,-33.,-22.5));
#33638=CARTESIAN_POINT('Origin',(-73.,-27.,-24.));
#33639=CARTESIAN_POINT('',(-79.,-27.,-22.5));
#33640=CARTESIAN_POINT('',(-79.,-27.,-24.));
#33641=CARTESIAN_POINT('Origin',(-73.,-27.,-22.5));
#33642=CARTESIAN_POINT('Origin',(-79.,27.,-24.));
#33643=CARTESIAN_POINT('',(-79.,27.,-22.5));
#33644=CARTESIAN_POINT('',(-79.,27.,-24.));
#33645=CARTESIAN_POINT('',(-79.,13.5,-22.5));
#33646=CARTESIAN_POINT('',(-79.,-14.,1.71450551880629E-15));
#33647=CARTESIAN_POINT('Origin',(-79.,0.,0.));
#33648=CARTESIAN_POINT('Origin',(-61.,0.,18.));
#33649=CARTESIAN_POINT('',(-71.,-1.22464679914735E-15,18.));
#33650=CARTESIAN_POINT('Origin',(-61.,0.,18.));
#33651=CARTESIAN_POINT('',(-65.5,-25.,18.));
#33652=CARTESIAN_POINT('Origin',(-61.,-25.,18.));
#33653=CARTESIAN_POINT('',(-65.5,25.,18.));
#33654=CARTESIAN_POINT('Origin',(-61.,25.,18.));
#33655=CARTESIAN_POINT('Origin',(-77.5,13.5,-22.5));
#33656=CARTESIAN_POINT('',(-77.5,27.,-24.));
#33657=CARTESIAN_POINT('Origin',(-77.5,27.,-22.5));
#33658=CARTESIAN_POINT('',(-77.5,-27.,-24.));
#33659=CARTESIAN_POINT('',(-77.5,13.5,-24.));
#33660=CARTESIAN_POINT('Origin',(-77.5,-27.,-22.5));
#33661=CARTESIAN_POINT('Origin',(-73.,-27.,-22.5));
#33662=CARTESIAN_POINT('',(-73.,-31.5,-24.));
#33663=CARTESIAN_POINT('Origin',(-73.,-31.5,-22.5));
#33664=CARTESIAN_POINT('Origin',(-73.,-27.,-24.));
#33665=CARTESIAN_POINT('Origin',(-67.,-31.5,-22.5));
#33666=CARTESIAN_POINT('',(-49.,-31.5,-24.));
#33667=CARTESIAN_POINT('Origin',(-49.,-31.5,-22.5));
#33668=CARTESIAN_POINT('',(-67.,-31.5,-24.));
#33669=CARTESIAN_POINT('Origin',(-49.,-27.,-22.5));
#33670=CARTESIAN_POINT('',(-44.5,-27.,-24.));
#33671=CARTESIAN_POINT('Origin',(-44.5,-27.,-22.5));
#33672=CARTESIAN_POINT('Origin',(-49.,-27.,-24.));
#33673=CARTESIAN_POINT('Origin',(-44.5,-13.5,-22.5));
#33674=CARTESIAN_POINT('',(-44.5,27.,-24.));
#33675=CARTESIAN_POINT('',(-43.,27.,-22.5));
#33676=CARTESIAN_POINT('Origin',(-44.5,27.,-22.5));
#33677=CARTESIAN_POINT('',(-43.,-13.5,-22.5));
#33678=CARTESIAN_POINT('',(-44.5,-13.5,-24.));
#33679=CARTESIAN_POINT('Origin',(-49.,27.,-22.5));
#33680=CARTESIAN_POINT('',(-49.,31.5,-24.));
#33681=CARTESIAN_POINT('',(-49.,33.,-22.5));
#33682=CARTESIAN_POINT('Origin',(-49.,31.5,-22.5));
#33683=CARTESIAN_POINT('Origin',(-49.,27.,-22.5));
#33684=CARTESIAN_POINT('Origin',(-49.,27.,-24.));
#33685=CARTESIAN_POINT('Origin',(-55.,31.5,-22.5));
#33686=CARTESIAN_POINT('',(-73.,31.5,-24.));
#33687=CARTESIAN_POINT('',(-73.,33.,-22.5));
#33688=CARTESIAN_POINT('Origin',(-73.,31.5,-22.5));
#33689=CARTESIAN_POINT('',(-55.,33.,-22.5));
#33690=CARTESIAN_POINT('',(-55.,31.5,-24.));
#33691=CARTESIAN_POINT('Origin',(-73.,27.,-22.5));
#33692=CARTESIAN_POINT('Origin',(-73.,27.,-22.5));
#33693=CARTESIAN_POINT('Origin',(-73.,27.,-24.));
#33694=CARTESIAN_POINT('Origin',(-49.,27.,-24.));
#33695=CARTESIAN_POINT('',(-43.,27.,-24.));
#33696=CARTESIAN_POINT('',(-49.,33.,-24.));
#33697=CARTESIAN_POINT('Origin',(-49.,33.,-24.));
#33698=CARTESIAN_POINT('',(-73.,33.,-24.));
#33699=CARTESIAN_POINT('Origin',(-73.,27.,-24.));
#33700=CARTESIAN_POINT('Origin',(-61.,0.,-24.));
#33701=CARTESIAN_POINT('',(-65.5,-25.,-24.));
#33702=CARTESIAN_POINT('Origin',(-61.,-25.,-24.));
#33703=CARTESIAN_POINT('',(-65.5,25.,-24.));
#33704=CARTESIAN_POINT('Origin',(-61.,25.,-24.));
#33705=CARTESIAN_POINT('Origin',(44.5,13.5,16.5));
#33706=CARTESIAN_POINT('',(44.5,27.,18.));
#33707=CARTESIAN_POINT('',(43.,27.,16.5));
#33708=CARTESIAN_POINT('Origin',(44.5,27.,16.5));
#33709=CARTESIAN_POINT('',(43.,-27.,16.5));
#33710=CARTESIAN_POINT('',(43.,13.5,16.5));
#33711=CARTESIAN_POINT('',(44.5,-27.,18.));
#33712=CARTESIAN_POINT('Origin',(44.5,-27.,16.5));
#33713=CARTESIAN_POINT('',(44.5,13.5,18.));
#33714=CARTESIAN_POINT('Origin',(49.,-27.,16.5));
#33715=CARTESIAN_POINT('',(49.,-33.,16.5));
#33716=CARTESIAN_POINT('',(49.,-31.5,18.));
#33717=CARTESIAN_POINT('Origin',(49.,-31.5,16.5));
#33718=CARTESIAN_POINT('Origin',(49.,-27.,18.));
#33719=CARTESIAN_POINT('Origin',(49.,-27.,16.5));
#33720=CARTESIAN_POINT('Origin',(55.,-31.5,16.5));
#33721=CARTESIAN_POINT('',(73.,-33.,16.5));
#33722=CARTESIAN_POINT('',(73.,-31.5,18.));
#33723=CARTESIAN_POINT('Origin',(73.,-31.5,16.5));
#33724=CARTESIAN_POINT('',(55.,-31.5,18.));
#33725=CARTESIAN_POINT('',(55.,-33.,16.5));
#33726=CARTESIAN_POINT('Origin',(73.,-27.,16.5));
#33727=CARTESIAN_POINT('',(79.,-27.,16.5));
#33728=CARTESIAN_POINT('',(77.5,-27.,18.));
#33729=CARTESIAN_POINT('Origin',(77.5,-27.,16.5));
#33730=CARTESIAN_POINT('Origin',(73.,-27.,18.));
#33731=CARTESIAN_POINT('Origin',(73.,-27.,16.5));
#33732=CARTESIAN_POINT('Origin',(77.5,-13.5,16.5));
#33733=CARTESIAN_POINT('',(79.,27.,16.5));
#33734=CARTESIAN_POINT('',(77.5,27.,18.));
#33735=CARTESIAN_POINT('Origin',(77.5,27.,16.5));
#33736=CARTESIAN_POINT('',(77.5,-13.5,18.));
#33737=CARTESIAN_POINT('',(79.,-13.5,16.5));
#33738=CARTESIAN_POINT('Origin',(73.,27.,16.5));
#33739=CARTESIAN_POINT('',(73.,33.,16.5));
#33740=CARTESIAN_POINT('',(73.,31.5,18.));
#33741=CARTESIAN_POINT('Origin',(73.,31.5,16.5));
#33742=CARTESIAN_POINT('Origin',(73.,27.,18.));
#33743=CARTESIAN_POINT('Origin',(73.,27.,16.5));
#33744=CARTESIAN_POINT('Origin',(67.,31.5,16.5));
#33745=CARTESIAN_POINT('',(49.,33.,16.5));
#33746=CARTESIAN_POINT('',(49.,31.5,18.));
#33747=CARTESIAN_POINT('Origin',(49.,31.5,16.5));
#33748=CARTESIAN_POINT('',(67.,31.5,18.));
#33749=CARTESIAN_POINT('',(67.,33.,16.5));
#33750=CARTESIAN_POINT('Origin',(49.,27.,16.5));
#33751=CARTESIAN_POINT('Origin',(49.,27.,18.));
#33752=CARTESIAN_POINT('Origin',(49.,27.,16.5));
#33753=CARTESIAN_POINT('Origin',(73.,-27.,-24.));
#33754=CARTESIAN_POINT('',(73.,-33.,-22.5));
#33755=CARTESIAN_POINT('',(73.,-33.,-24.));
#33756=CARTESIAN_POINT('',(79.,-27.,-22.5));
#33757=CARTESIAN_POINT('Origin',(73.,-27.,-22.5));
#33758=CARTESIAN_POINT('',(79.,-27.,-24.));
#33759=CARTESIAN_POINT('Origin',(49.,-33.,-24.));
#33760=CARTESIAN_POINT('',(49.,-33.,-22.5));
#33761=CARTESIAN_POINT('',(49.,-33.,-24.));
#33762=CARTESIAN_POINT('',(55.,-33.,-22.5));
#33763=CARTESIAN_POINT('Origin',(49.,-27.,-24.));
#33764=CARTESIAN_POINT('',(43.,-27.,-22.5));
#33765=CARTESIAN_POINT('',(43.,-27.,-24.));
#33766=CARTESIAN_POINT('Origin',(49.,-27.,-22.5));
#33767=CARTESIAN_POINT('Origin',(43.,27.,-24.));
#33768=CARTESIAN_POINT('',(43.,27.,-22.5));
#33769=CARTESIAN_POINT('',(43.,27.,-24.));
#33770=CARTESIAN_POINT('',(43.,13.5,-22.5));
#33771=CARTESIAN_POINT('',(43.,-14.,1.71450551880629E-15));
#33772=CARTESIAN_POINT('Origin',(43.,0.,0.));
#33773=CARTESIAN_POINT('Origin',(61.,0.,18.));
#33774=CARTESIAN_POINT('',(51.,-1.22464679914735E-15,18.));
#33775=CARTESIAN_POINT('Origin',(61.,0.,18.));
#33776=CARTESIAN_POINT('',(56.5,25.,18.));
#33777=CARTESIAN_POINT('Origin',(61.,25.,18.));
#33778=CARTESIAN_POINT('',(56.5,-25.,18.));
#33779=CARTESIAN_POINT('Origin',(61.,-25.,18.));
#33780=CARTESIAN_POINT('Origin',(44.5,13.5,-22.5));
#33781=CARTESIAN_POINT('',(44.5,27.,-24.));
#33782=CARTESIAN_POINT('Origin',(44.5,27.,-22.5));
#33783=CARTESIAN_POINT('',(44.5,-27.,-24.));
#33784=CARTESIAN_POINT('',(44.5,13.5,-24.));
#33785=CARTESIAN_POINT('Origin',(44.5,-27.,-22.5));
#33786=CARTESIAN_POINT('Origin',(49.,-27.,-22.5));
#33787=CARTESIAN_POINT('',(49.,-31.5,-24.));
#33788=CARTESIAN_POINT('Origin',(49.,-31.5,-22.5));
#33789=CARTESIAN_POINT('Origin',(49.,-27.,-24.));
#33790=CARTESIAN_POINT('Origin',(55.,-31.5,-22.5));
#33791=CARTESIAN_POINT('',(73.,-31.5,-24.));
#33792=CARTESIAN_POINT('Origin',(73.,-31.5,-22.5));
#33793=CARTESIAN_POINT('',(55.,-31.5,-24.));
#33794=CARTESIAN_POINT('Origin',(73.,-27.,-22.5));
#33795=CARTESIAN_POINT('',(77.5,-27.,-24.));
#33796=CARTESIAN_POINT('Origin',(77.5,-27.,-22.5));
#33797=CARTESIAN_POINT('Origin',(73.,-27.,-24.));
#33798=CARTESIAN_POINT('Origin',(77.5,-13.5,-22.5));
#33799=CARTESIAN_POINT('',(77.5,27.,-24.));
#33800=CARTESIAN_POINT('',(79.,27.,-22.5));
#33801=CARTESIAN_POINT('Origin',(77.5,27.,-22.5));
#33802=CARTESIAN_POINT('',(79.,-13.5,-22.5));
#33803=CARTESIAN_POINT('',(77.5,-13.5,-24.));
#33804=CARTESIAN_POINT('Origin',(73.,27.,-22.5));
#33805=CARTESIAN_POINT('',(73.,31.5,-24.));
#33806=CARTESIAN_POINT('',(73.,33.,-22.5));
#33807=CARTESIAN_POINT('Origin',(73.,31.5,-22.5));
#33808=CARTESIAN_POINT('Origin',(73.,27.,-22.5));
#33809=CARTESIAN_POINT('Origin',(73.,27.,-24.));
#33810=CARTESIAN_POINT('Origin',(67.,31.5,-22.5));
#33811=CARTESIAN_POINT('',(49.,31.5,-24.));
#33812=CARTESIAN_POINT('',(49.,33.,-22.5));
#33813=CARTESIAN_POINT('Origin',(49.,31.5,-22.5));
#33814=CARTESIAN_POINT('',(67.,33.,-22.5));
#33815=CARTESIAN_POINT('',(67.,31.5,-24.));
#33816=CARTESIAN_POINT('Origin',(49.,27.,-22.5));
#33817=CARTESIAN_POINT('Origin',(49.,27.,-22.5));
#33818=CARTESIAN_POINT('Origin',(49.,27.,-24.));
#33819=CARTESIAN_POINT('Origin',(73.,27.,-24.));
#33820=CARTESIAN_POINT('',(79.,27.,-24.));
#33821=CARTESIAN_POINT('',(73.,33.,-24.));
#33822=CARTESIAN_POINT('Origin',(73.,33.,-24.));
#33823=CARTESIAN_POINT('',(49.,33.,-24.));
#33824=CARTESIAN_POINT('Origin',(49.,27.,-24.));
#33825=CARTESIAN_POINT('Origin',(61.,0.,-24.));
#33826=CARTESIAN_POINT('',(56.5,25.,-24.));
#33827=CARTESIAN_POINT('Origin',(61.,25.,-24.));
#33828=CARTESIAN_POINT('',(56.5,-25.,-24.));
#33829=CARTESIAN_POINT('Origin',(61.,-25.,-24.));
#33830=CARTESIAN_POINT('Ctrl Pts',(61.,10.,0.));
#33831=CARTESIAN_POINT('Ctrl Pts',(59.5040034982906,10.,1.72039597696584));
#33832=CARTESIAN_POINT('Ctrl Pts',(56.5121809687138,9.31827600185967,5.16099188597912));
#33833=CARTESIAN_POINT('Ctrl Pts',(52.9151698102436,6.44751899352647,9.29755471821987));
#33834=CARTESIAN_POINT('Ctrl Pts',(50.916118401284,2.30148284591066,11.5964638385234));
#33835=CARTESIAN_POINT('Ctrl Pts',(50.9184096402541,-2.30110422892933,11.5938289137078));
#33836=CARTESIAN_POINT('Ctrl Pts',(52.9132003149412,-6.44872389556736,9.29981963781766));
#33837=CARTESIAN_POINT('Ctrl Pts',(56.5134223825492,-9.3173037934771,5.15956426006841));
#33838=CARTESIAN_POINT('Ctrl Pts',(59.5040034982906,-10.,1.72039597696584));
#33839=CARTESIAN_POINT('Ctrl Pts',(61.,-10.,0.));
#33840=CARTESIAN_POINT('Ctrl Pts',(61.,10.,0.));
#33841=CARTESIAN_POINT('Ctrl Pts',(59.4612607410989,10.,1.67765321977414));
#33842=CARTESIAN_POINT('Ctrl Pts',(56.3852895451264,9.2787466754377,5.03147281006447));
#33843=CARTESIAN_POINT('Ctrl Pts',(52.7787910927581,6.28233675146603,9.01828223151668));
#33844=CARTESIAN_POINT('Ctrl Pts',(50.9218563946624,2.16780125001729,11.1411198281225));
#33845=CARTESIAN_POINT('Ctrl Pts',(50.921935151735,-2.16957611933213,11.139875359174));
#33846=CARTESIAN_POINT('Ctrl Pts',(52.7749511431933,-6.28255214648714,9.02170832410809));
#33847=CARTESIAN_POINT('Ctrl Pts',(56.3865568068429,-9.27716494796019,5.03035580652707));
#33848=CARTESIAN_POINT('Ctrl Pts',(59.4612607410989,-10.,1.67765321977414));
#33849=CARTESIAN_POINT('Ctrl Pts',(61.,-10.,-1.16633028490224E-16));
#33850=CARTESIAN_POINT('Ctrl Pts',(61.,10.,0.));
#33851=CARTESIAN_POINT('Ctrl Pts',(59.3864609160134,10.,1.60285339468867));
#33852=CARTESIAN_POINT('Ctrl Pts',(56.1634454725933,9.24997499276094,4.8044724705041));
#33853=CARTESIAN_POINT('Ctrl Pts',(52.4020469154053,6.14806419752617,8.52856750953951));
#33854=CARTESIAN_POINT('Ctrl Pts',(50.5404578733979,2.04963586749967,10.355517733166));
#33855=CARTESIAN_POINT('Ctrl Pts',(50.540659846251,-2.05249740360806,10.3555567579218));
#33856=CARTESIAN_POINT('Ctrl Pts',(52.3971494142207,-6.14820999431346,8.53360127461872));
#33857=CARTESIAN_POINT('Ctrl Pts',(56.163818037358,-9.24763407888523,4.80405041789639));
#33858=CARTESIAN_POINT('Ctrl Pts',(59.3864609160134,-10.,1.60285339468867));
#33859=CARTESIAN_POINT('Ctrl Pts',(61.,-10.,-3.20740828348117E-16));
#33860=CARTESIAN_POINT('Ctrl Pts',(61.,10.,0.));
#33861=CARTESIAN_POINT('Ctrl Pts',(59.3116610909279,10.,1.5280535696032));
#33862=CARTESIAN_POINT('Ctrl Pts',(55.9363931602234,9.28829710822045,4.58270974350988));
#33863=CARTESIAN_POINT('Ctrl Pts',(51.9123266113155,6.32379422406357,8.1866464187036));
#33864=CARTESIAN_POINT('Ctrl Pts',(49.7441230249571,2.20237919885278,10.0805955452152));
#33865=CARTESIAN_POINT('Ctrl Pts',(49.7460827491046,-2.20331916195195,10.0795573075147));
#33866=CARTESIAN_POINT('Ctrl Pts',(51.9092854431927,-6.32444064491119,8.18991583103531));
#33867=CARTESIAN_POINT('Ctrl Pts',(55.9374860580148,-9.28688811871409,4.58156316448158));
#33868=CARTESIAN_POINT('Ctrl Pts',(59.3116610909279,-10.,1.5280535696032));
#33869=CARTESIAN_POINT('Ctrl Pts',(61.,-10.,-5.2484862820601E-16));
#33870=CARTESIAN_POINT('Ctrl Pts',(61.,10.,0.));
#33871=CARTESIAN_POINT('Ctrl Pts',(59.2796040230342,10.,1.49599650170942));
#33872=CARTESIAN_POINT('Ctrl Pts',(55.8390081140209,9.31827600185966,4.48781903128619));
#33873=CARTESIAN_POINT('Ctrl Pts',(51.7024452817801,6.44751899352647,8.08483018975641));
#33874=CARTESIAN_POINT('Ctrl Pts',(49.4035361614766,2.30148284591066,10.083881598716));
#33875=CARTESIAN_POINT('Ctrl Pts',(49.4061710862922,-2.30110422892933,10.0815903597459));
#33876=CARTESIAN_POINT('Ctrl Pts',(51.7001803621823,-6.44872389556736,8.08679968505884));
#33877=CARTESIAN_POINT('Ctrl Pts',(55.8404357399316,-9.3173037934771,4.48657761745079));
#33878=CARTESIAN_POINT('Ctrl Pts',(59.2796040230342,-10.,1.49599650170942));
#33879=CARTESIAN_POINT('Ctrl Pts',(61.,-10.,-6.12323399573678E-16));
#33880=CARTESIAN_POINT('',(51.,1.22464679914735E-15,11.5));
#33881=CARTESIAN_POINT('Origin',(61.,0.,-1.11022302462516E-15));
#33882=CARTESIAN_POINT('Origin',(61.,0.,-1.11022302462516E-15));
#33883=CARTESIAN_POINT('Ctrl Pts',(61.,-10.,0.));
#33884=CARTESIAN_POINT('Ctrl Pts',(62.4959965017094,-10.,1.72039597696584));
#33885=CARTESIAN_POINT('Ctrl Pts',(65.4878388575297,-9.31826228028074,5.16101468615917));
#33886=CARTESIAN_POINT('Ctrl Pts',(69.0848089584877,-6.44748693262444,9.2975303022608));
#33887=CARTESIAN_POINT('Ctrl Pts',(71.0839062596644,-2.30147560731927,11.596492198614));
#33888=CARTESIAN_POINT('Ctrl Pts',(71.0815657345164,2.3010998930418,11.5938005946939));
#33889=CARTESIAN_POINT('Ctrl Pts',(69.0868232329507,6.44874145130402,9.29984671789331));
#33890=CARTESIAN_POINT('Ctrl Pts',(65.4865746588077,9.31727427505449,5.15956085762893));
#33891=CARTESIAN_POINT('Ctrl Pts',(62.4959965017094,10.,1.72039597696584));
#33892=CARTESIAN_POINT('Ctrl Pts',(61.,10.,0.));
#33893=CARTESIAN_POINT('Ctrl Pts',(61.,-10.,-1.16633028490224E-16));
#33894=CARTESIAN_POINT('Ctrl Pts',(62.5387392589011,-10.,1.67765321977414));
#33895=CARTESIAN_POINT('Ctrl Pts',(65.6147402149094,-9.27874444858818,5.0314839646684));
#33896=CARTESIAN_POINT('Ctrl Pts',(69.2211149565067,-6.28225704725854,9.018198244725));
#33897=CARTESIAN_POINT('Ctrl Pts',(71.0780204967536,-2.16769213476844,11.1410773775261));
#33898=CARTESIAN_POINT('Ctrl Pts',(71.0779550071476,2.16958048977102,11.139828336814));
#33899=CARTESIAN_POINT('Ctrl Pts',(69.2251092841024,6.28254286828191,9.02175516699167));
#33900=CARTESIAN_POINT('Ctrl Pts',(65.6135473050458,9.277121682446,5.03041327352834));
#33901=CARTESIAN_POINT('Ctrl Pts',(62.5387392589011,10.,1.67765321977414));
#33902=CARTESIAN_POINT('Ctrl Pts',(61.,10.,0.));
#33903=CARTESIAN_POINT('Ctrl Pts',(61.,-10.,-3.20740828348117E-16));
#33904=CARTESIAN_POINT('Ctrl Pts',(62.6135390839866,-10.,1.60285339468867));
#33905=CARTESIAN_POINT('Ctrl Pts',(65.8365086336303,-9.24999260746104,4.80443145593069));
#33906=CARTESIAN_POINT('Ctrl Pts',(69.5977546769801,-6.14807857455455,8.52836701951912));
#33907=CARTESIAN_POINT('Ctrl Pts',(71.4595637706598,-2.04957572202921,10.3555252406934));
#33908=CARTESIAN_POINT('Ctrl Pts',(71.4594638033093,2.05269181819478,10.3556714380237));
#33909=CARTESIAN_POINT('Ctrl Pts',(69.6029136286413,6.14828611739566,8.53366950962115));
#33910=CARTESIAN_POINT('Ctrl Pts',(65.8362560480664,9.24757421412897,4.80413551166672));
#33911=CARTESIAN_POINT('Ctrl Pts',(62.6135390839866,10.,1.60285339468867));
#33912=CARTESIAN_POINT('Ctrl Pts',(61.,10.,0.));
#33913=CARTESIAN_POINT('Ctrl Pts',(61.,-10.,-5.2484862820601E-16));
#33914=CARTESIAN_POINT('Ctrl Pts',(62.6883389090721,-10.,1.5280535696032));
#33915=CARTESIAN_POINT('Ctrl Pts',(66.0636051991207,-9.28829063155977,4.58271947637952));
#33916=CARTESIAN_POINT('Ctrl Pts',(70.0875935962318,-6.32376606817711,8.18655899425094));
#33917=CARTESIAN_POINT('Ctrl Pts',(72.255906691879,-2.20233839346268,10.0805696428556));
#33918=CARTESIAN_POINT('Ctrl Pts',(72.2539378332695,2.20337142560397,10.0795384423798));
#33919=CARTESIAN_POINT('Ctrl Pts',(70.0907494790084,6.32446716030411,8.18995953920261));
#33920=CARTESIAN_POINT('Ctrl Pts',(66.0625288064666,9.28684508262977,4.58161014100602));
#33921=CARTESIAN_POINT('Ctrl Pts',(62.6883389090721,10.,1.5280535696032));
#33922=CARTESIAN_POINT('Ctrl Pts',(61.,10.,0.));
#33923=CARTESIAN_POINT('Ctrl Pts',(61.,-10.,-6.12323399573678E-16));
#33924=CARTESIAN_POINT('Ctrl Pts',(62.7203959769658,-10.,1.49599650170942));
#33925=CARTESIAN_POINT('Ctrl Pts',(66.1610146861591,-9.31826228028074,4.48783885752971));
#33926=CARTESIAN_POINT('Ctrl Pts',(70.2975303022608,-6.44748693262444,8.08480895848765));
#33927=CARTESIAN_POINT('Ctrl Pts',(72.596492198614,-2.30147560731927,10.0839062596644));
#33928=CARTESIAN_POINT('Ctrl Pts',(72.5938005946939,2.3010998930418,10.0815657345164));
#33929=CARTESIAN_POINT('Ctrl Pts',(70.2998467178933,6.44874145130402,8.0868232329507));
#33930=CARTESIAN_POINT('Ctrl Pts',(66.1595608576289,9.31727427505449,4.48657465880776));
#33931=CARTESIAN_POINT('Ctrl Pts',(62.7203959769658,10.,1.49599650170942));
#33932=CARTESIAN_POINT('Ctrl Pts',(61.,10.,0.));
#33933=CARTESIAN_POINT('Origin',(61.,0.,-1.11022302462516E-15));
#33934=CARTESIAN_POINT('Ctrl Pts',(-61.,10.,0.));
#33935=CARTESIAN_POINT('Ctrl Pts',(-62.4959965017094,10.,1.72039597696584));
#33936=CARTESIAN_POINT('Ctrl Pts',(-65.4878388575297,9.31826228028074,5.16101468615917));
#33937=CARTESIAN_POINT('Ctrl Pts',(-69.0848089584877,6.44748693262444,9.2975303022608));
#33938=CARTESIAN_POINT('Ctrl Pts',(-71.0839062596644,2.30147560731927,11.596492198614));
#33939=CARTESIAN_POINT('Ctrl Pts',(-71.0815657345164,-2.3010998930418,11.5938005946939));
#33940=CARTESIAN_POINT('Ctrl Pts',(-69.0868232329507,-6.44874145130402,
9.29984671789331));
#33941=CARTESIAN_POINT('Ctrl Pts',(-65.4865746588077,-9.31727427505449,
5.15956085762893));
#33942=CARTESIAN_POINT('Ctrl Pts',(-62.4959965017094,-10.,1.72039597696584));
#33943=CARTESIAN_POINT('Ctrl Pts',(-61.,-10.,0.));
#33944=CARTESIAN_POINT('Ctrl Pts',(-61.,10.,0.));
#33945=CARTESIAN_POINT('Ctrl Pts',(-62.5387392589011,10.,1.67765321977414));
#33946=CARTESIAN_POINT('Ctrl Pts',(-65.6147402149094,9.27874444858818,5.0314839646684));
#33947=CARTESIAN_POINT('Ctrl Pts',(-69.2211149565067,6.28225704725854,9.018198244725));
#33948=CARTESIAN_POINT('Ctrl Pts',(-71.0780204967536,2.16769213476844,11.1410773775261));
#33949=CARTESIAN_POINT('Ctrl Pts',(-71.0779550071476,-2.16958048977102,
11.139828336814));
#33950=CARTESIAN_POINT('Ctrl Pts',(-69.2251092841024,-6.28254286828192,
9.02175516699167));
#33951=CARTESIAN_POINT('Ctrl Pts',(-65.6135473050458,-9.277121682446,5.03041327352834));
#33952=CARTESIAN_POINT('Ctrl Pts',(-62.5387392589011,-10.,1.67765321977414));
#33953=CARTESIAN_POINT('Ctrl Pts',(-61.,-10.,-1.16633028490224E-16));
#33954=CARTESIAN_POINT('Ctrl Pts',(-61.,10.,0.));
#33955=CARTESIAN_POINT('Ctrl Pts',(-62.6135390839866,10.,1.60285339468867));
#33956=CARTESIAN_POINT('Ctrl Pts',(-65.8365086336303,9.24999260746104,4.80443145593068));
#33957=CARTESIAN_POINT('Ctrl Pts',(-69.5977546769801,6.14807857455454,8.52836701951912));
#33958=CARTESIAN_POINT('Ctrl Pts',(-71.4595637706598,2.04957572202922,10.3555252406934));
#33959=CARTESIAN_POINT('Ctrl Pts',(-71.4594638033093,-2.05269181819478,
10.3556714380237));
#33960=CARTESIAN_POINT('Ctrl Pts',(-69.6029136286413,-6.14828611739566,
8.53366950962116));
#33961=CARTESIAN_POINT('Ctrl Pts',(-65.8362560480664,-9.24757421412897,
4.80413551166671));
#33962=CARTESIAN_POINT('Ctrl Pts',(-62.6135390839866,-10.,1.60285339468867));
#33963=CARTESIAN_POINT('Ctrl Pts',(-61.,-10.,-3.20740828348117E-16));
#33964=CARTESIAN_POINT('Ctrl Pts',(-61.,10.,0.));
#33965=CARTESIAN_POINT('Ctrl Pts',(-62.6883389090721,10.,1.5280535696032));
#33966=CARTESIAN_POINT('Ctrl Pts',(-66.0636051991207,9.28829063155977,4.58271947637952));
#33967=CARTESIAN_POINT('Ctrl Pts',(-70.0875935962318,6.32376606817712,8.18655899425094));
#33968=CARTESIAN_POINT('Ctrl Pts',(-72.255906691879,2.20233839346268,10.0805696428556));
#33969=CARTESIAN_POINT('Ctrl Pts',(-72.2539378332695,-2.20337142560396,
10.0795384423798));
#33970=CARTESIAN_POINT('Ctrl Pts',(-70.0907494790084,-6.32446716030411,
8.18995953920261));
#33971=CARTESIAN_POINT('Ctrl Pts',(-66.0625288064666,-9.28684508262977,
4.58161014100602));
#33972=CARTESIAN_POINT('Ctrl Pts',(-62.6883389090721,-10.,1.5280535696032));
#33973=CARTESIAN_POINT('Ctrl Pts',(-61.,-10.,-5.2484862820601E-16));
#33974=CARTESIAN_POINT('Ctrl Pts',(-61.,10.,0.));
#33975=CARTESIAN_POINT('Ctrl Pts',(-62.7203959769658,10.,1.49599650170942));
#33976=CARTESIAN_POINT('Ctrl Pts',(-66.1610146861591,9.31826228028074,4.48783885752971));
#33977=CARTESIAN_POINT('Ctrl Pts',(-70.2975303022608,6.44748693262445,8.08480895848765));
#33978=CARTESIAN_POINT('Ctrl Pts',(-72.596492198614,2.30147560731927,10.0839062596644));
#33979=CARTESIAN_POINT('Ctrl Pts',(-72.5938005946939,-2.3010998930418,10.0815657345164));
#33980=CARTESIAN_POINT('Ctrl Pts',(-70.2998467178933,-6.44874145130402,
8.0868232329507));
#33981=CARTESIAN_POINT('Ctrl Pts',(-66.1595608576289,-9.31727427505449,
4.48657465880776));
#33982=CARTESIAN_POINT('Ctrl Pts',(-62.7203959769658,-10.,1.49599650170942));
#33983=CARTESIAN_POINT('Ctrl Pts',(-61.,-10.,-6.12323399573678E-16));
#33984=CARTESIAN_POINT('',(-71.,1.22464679914735E-15,11.5));
#33985=CARTESIAN_POINT('Origin',(-61.,0.,-1.11022302462516E-15));
#33986=CARTESIAN_POINT('Origin',(-61.,0.,-1.11022302462516E-15));
#33987=CARTESIAN_POINT('Ctrl Pts',(-61.,-10.,0.));
#33988=CARTESIAN_POINT('Ctrl Pts',(-59.5040034982906,-10.,1.72039597696584));
#33989=CARTESIAN_POINT('Ctrl Pts',(-56.5121809687138,-9.31827600185967,
5.16099188597912));
#33990=CARTESIAN_POINT('Ctrl Pts',(-52.9151698102436,-6.44751899352647,
9.29755471821987));
#33991=CARTESIAN_POINT('Ctrl Pts',(-50.916118401284,-2.30148284591066,11.5964638385234));
#33992=CARTESIAN_POINT('Ctrl Pts',(-50.9184096402541,2.30110422892933,11.5938289137078));
#33993=CARTESIAN_POINT('Ctrl Pts',(-52.9132003149412,6.44872389556736,9.29981963781766));
#33994=CARTESIAN_POINT('Ctrl Pts',(-56.5134223825492,9.3173037934771,5.15956426006841));
#33995=CARTESIAN_POINT('Ctrl Pts',(-59.5040034982906,10.,1.72039597696584));
#33996=CARTESIAN_POINT('Ctrl Pts',(-61.,10.,0.));
#33997=CARTESIAN_POINT('Ctrl Pts',(-61.,-10.,-1.16633028490224E-16));
#33998=CARTESIAN_POINT('Ctrl Pts',(-59.4612607410989,-10.,1.67765321977414));
#33999=CARTESIAN_POINT('Ctrl Pts',(-56.3852895451264,-9.27874667543771,
5.03147281006447));
#34000=CARTESIAN_POINT('Ctrl Pts',(-52.7787910927581,-6.28233675146603,
9.01828223151668));
#34001=CARTESIAN_POINT('Ctrl Pts',(-50.9218563946624,-2.16780125001729,
11.1411198281225));
#34002=CARTESIAN_POINT('Ctrl Pts',(-50.921935151735,2.16957611933213,11.139875359174));
#34003=CARTESIAN_POINT('Ctrl Pts',(-52.7749511431933,6.28255214648713,9.0217083241081));
#34004=CARTESIAN_POINT('Ctrl Pts',(-56.3865568068429,9.27716494796019,5.03035580652706));
#34005=CARTESIAN_POINT('Ctrl Pts',(-59.4612607410989,10.,1.67765321977414));
#34006=CARTESIAN_POINT('Ctrl Pts',(-61.,10.,0.));
#34007=CARTESIAN_POINT('Ctrl Pts',(-61.,-10.,-3.20740828348117E-16));
#34008=CARTESIAN_POINT('Ctrl Pts',(-59.3864609160134,-10.,1.60285339468867));
#34009=CARTESIAN_POINT('Ctrl Pts',(-56.1634454725933,-9.24997499276093,
4.80447247050411));
#34010=CARTESIAN_POINT('Ctrl Pts',(-52.4020469154053,-6.14806419752618,
8.5285675095395));
#34011=CARTESIAN_POINT('Ctrl Pts',(-50.5404578733979,-2.04963586749967,
10.355517733166));
#34012=CARTESIAN_POINT('Ctrl Pts',(-50.540659846251,2.05249740360806,10.3555567579218));
#34013=CARTESIAN_POINT('Ctrl Pts',(-52.3971494142207,6.14820999431346,8.53360127461872));
#34014=CARTESIAN_POINT('Ctrl Pts',(-56.163818037358,9.24763407888523,4.8040504178964));
#34015=CARTESIAN_POINT('Ctrl Pts',(-59.3864609160134,10.,1.60285339468867));
#34016=CARTESIAN_POINT('Ctrl Pts',(-61.,10.,0.));
#34017=CARTESIAN_POINT('Ctrl Pts',(-61.,-10.,-5.2484862820601E-16));
#34018=CARTESIAN_POINT('Ctrl Pts',(-59.3116610909279,-10.,1.5280535696032));
#34019=CARTESIAN_POINT('Ctrl Pts',(-55.9363931602234,-9.28829710822045,
4.58270974350988));
#34020=CARTESIAN_POINT('Ctrl Pts',(-51.9123266113155,-6.32379422406357,
8.1866464187036));
#34021=CARTESIAN_POINT('Ctrl Pts',(-49.7441230249571,-2.20237919885278,
10.0805955452152));
#34022=CARTESIAN_POINT('Ctrl Pts',(-49.7460827491046,2.20331916195195,10.0795573075147));
#34023=CARTESIAN_POINT('Ctrl Pts',(-51.9092854431927,6.3244406449112,8.18991583103531));
#34024=CARTESIAN_POINT('Ctrl Pts',(-55.9374860580148,9.28688811871409,4.58156316448158));
#34025=CARTESIAN_POINT('Ctrl Pts',(-59.3116610909279,10.,1.5280535696032));
#34026=CARTESIAN_POINT('Ctrl Pts',(-61.,10.,0.));
#34027=CARTESIAN_POINT('Ctrl Pts',(-61.,-10.,-6.12323399573678E-16));
#34028=CARTESIAN_POINT('Ctrl Pts',(-59.2796040230342,-10.,1.49599650170942));
#34029=CARTESIAN_POINT('Ctrl Pts',(-55.8390081140209,-9.31827600185966,
4.48781903128619));
#34030=CARTESIAN_POINT('Ctrl Pts',(-51.7024452817801,-6.44751899352647,
8.08483018975641));
#34031=CARTESIAN_POINT('Ctrl Pts',(-49.4035361614766,-2.30148284591066,
10.083881598716));
#34032=CARTESIAN_POINT('Ctrl Pts',(-49.4061710862922,2.30110422892933,10.0815903597459));
#34033=CARTESIAN_POINT('Ctrl Pts',(-51.7001803621823,6.44872389556736,8.08679968505883));
#34034=CARTESIAN_POINT('Ctrl Pts',(-55.8404357399316,9.3173037934771,4.48657761745079));
#34035=CARTESIAN_POINT('Ctrl Pts',(-59.2796040230342,10.,1.49599650170942));
#34036=CARTESIAN_POINT('Ctrl Pts',(-61.,10.,0.));
#34037=CARTESIAN_POINT('Origin',(-61.,0.,-1.11022302462516E-15));
#34038=CARTESIAN_POINT('Origin',(61.,-25.,18.));
#34039=CARTESIAN_POINT('',(56.5,-25.,18.));
#34040=CARTESIAN_POINT('Origin',(-61.,25.,18.));
#34041=CARTESIAN_POINT('',(-65.5,25.,18.));
#34042=CARTESIAN_POINT('Origin',(-61.,-25.,18.));
#34043=CARTESIAN_POINT('',(-65.5,-25.,18.));
#34044=CARTESIAN_POINT('Origin',(61.,25.,18.));
#34045=CARTESIAN_POINT('',(56.5,25.,18.));
#34046=CARTESIAN_POINT('Origin',(-61.,0.,18.));
#34047=CARTESIAN_POINT('',(-71.,1.22464679914735E-15,18.));
#34048=CARTESIAN_POINT('Origin',(61.,0.,18.));
#34049=CARTESIAN_POINT('',(51.,1.22464679914735E-15,18.));
#34050=CARTESIAN_POINT('Origin',(-85.05,0.,0.));
#34051=CARTESIAN_POINT('',(-85.05,-12.05,-1.47569939297256E-15));
#34052=CARTESIAN_POINT('Origin',(108.,10.55,0.));
#34053=CARTESIAN_POINT('Origin',(79.,-27.,-24.));
#34054=CARTESIAN_POINT('',(79.,-14.,-1.71450551880629E-15));
#34055=CARTESIAN_POINT('Origin',(79.,0.,0.));
#34056=CARTESIAN_POINT('Origin',(10.,0.,0.));
#34057=CARTESIAN_POINT('',(10.,-14.,-1.71450551880629E-15));
#34058=CARTESIAN_POINT('Origin',(-43.,-27.,-24.));
#34059=CARTESIAN_POINT('',(-43.,-14.,-1.71450551880629E-15));
#34060=CARTESIAN_POINT('Origin',(-43.,0.,0.));
#34061=CARTESIAN_POINT('Origin',(10.,0.,0.));
#34062=CARTESIAN_POINT('',(10.,-14.,-1.71450551880629E-15));
#34063=CARTESIAN_POINT('Origin',(10.,0.,0.));
#34064=CARTESIAN_POINT('',(10.,-14.,-1.71450551880629E-15));
#34065=CARTESIAN_POINT('',(0.,0.,0.));
#34066=CARTESIAN_POINT('Origin',(-85.75,0.,0.));
#34067=CARTESIAN_POINT('',(-89.5188431528481,-11.9252862155783,0.000296729823191094));
#34068=CARTESIAN_POINT('',(-89.7311568471519,-11.9248987907529,0.000229507259365661));
#34069=CARTESIAN_POINT('',(-85.75,-11.925,-1.46039130798322E-15));
#34070=CARTESIAN_POINT('',(-90.,5.1296446118907,10.7653319110792));
#34071=CARTESIAN_POINT('Ctrl Pts',(-89.5188431528481,-11.9252862155783,
0.000296729823191094));
#34072=CARTESIAN_POINT('Ctrl Pts',(-89.5262732725778,-11.9256675610804,
0.37140882978507));
#34073=CARTESIAN_POINT('Ctrl Pts',(-89.5337033923074,-11.9086887659417,
0.742486110439695));
#34074=CARTESIAN_POINT('Ctrl Pts',(-89.5411335120371,-11.874094865106,1.11191379148113));
#34075=CARTESIAN_POINT('Ctrl Pts',(-89.5809184802334,-11.6888599974842,
3.09003380513459));
#34076=CARTESIAN_POINT('Ctrl Pts',(-89.6207034484296,-10.9985782879942,
5.02085775997829));
#34077=CARTESIAN_POINT('Ctrl Pts',(-89.6604884166259,-9.88773523873562,
6.66807012563771));
#34078=CARTESIAN_POINT('Ctrl Pts',(-89.7002733848221,-8.77689218947705,
8.31528249129713));
#34079=CARTESIAN_POINT('Ctrl Pts',(-89.7400583530184,-7.24548780044994,
9.67888326777227));
#34080=CARTESIAN_POINT('Ctrl Pts',(-89.7798433212147,-5.48096071686973,
10.5919600041883));
#34081=CARTESIAN_POINT('Ctrl Pts',(-89.8196282894109,-3.71643363328953,
11.5050367406042));
#34082=CARTESIAN_POINT('Ctrl Pts',(-89.8594132576072,-1.71878385515623,
11.967589436961));
#34083=CARTESIAN_POINT('Ctrl Pts',(-89.8991982258034,0.267492608476263,
11.9230350042462));
#34084=CARTESIAN_POINT('Ctrl Pts',(-89.9327988172023,1.94501220659287,11.8854063380305));
#34085=CARTESIAN_POINT('Ctrl Pts',(-89.9663994086011,3.61441952603868,11.4860718254948));
#34086=CARTESIAN_POINT('Ctrl Pts',(-90.,5.13009691060871,10.7656670051304));
#34087=CARTESIAN_POINT('',(-90.,-5.1296446118933,10.765331911078));
#34088=CARTESIAN_POINT('Origin',(-90.,0.,0.));
#34089=CARTESIAN_POINT('Ctrl Pts',(-90.,-5.12964461189318,10.765331911078));
#34090=CARTESIAN_POINT('Ctrl Pts',(-89.9602150318037,-6.92369670303529,
9.91047209636926));
#34091=CARTESIAN_POINT('Ctrl Pts',(-89.9204300636075,-8.49893930959995,
8.59874522586898));
#34092=CARTESIAN_POINT('Ctrl Pts',(-89.8806450954112,-9.66327664795995,
6.98920240711812));
#34093=CARTESIAN_POINT('Ctrl Pts',(-89.840860127215,-10.8276139863199,5.37965958836726));
#34094=CARTESIAN_POINT('Ctrl Pts',(-89.8010751590187,-11.5810460564753,
3.47230082136582));
#34095=CARTESIAN_POINT('Ctrl Pts',(-89.7612901908224,-11.831183536793,1.50127032371404));
#34096=CARTESIAN_POINT('Ctrl Pts',(-89.7512457429322,-11.8943353501623,
1.00364737662614));
#34097=CARTESIAN_POINT('Ctrl Pts',(-89.741201295042,-11.9254070149145,0.501965974265288));
#34098=CARTESIAN_POINT('Ctrl Pts',(-89.7311568471519,-11.9248987907529,
0.000229507259365661));
#34099=CARTESIAN_POINT('Origin',(-85.75,0.,0.));
#34100=CARTESIAN_POINT('',(-88.0188431528482,-11.9249138545732,-0.000313305576115086));
#34101=CARTESIAN_POINT('',(-88.2311568471518,-11.9253287759226,-0.000290940587986354));
#34102=CARTESIAN_POINT('',(-85.75,-11.925,-1.46039130798322E-15));
#34103=CARTESIAN_POINT('Ctrl Pts',(-88.0188431528482,-11.9249138545732,
-0.000313305576115086));
#34104=CARTESIAN_POINT('Ctrl Pts',(-88.0488536542227,-11.9233842134251,
1.49875571795511));
#34105=CARTESIAN_POINT('Ctrl Pts',(-88.0788641555972,-11.6398512903311,
2.99838693882232));
#34106=CARTESIAN_POINT('Ctrl Pts',(-88.1088746569718,-11.0879741656425,
4.39173220896684));
#34107=CARTESIAN_POINT('Ctrl Pts',(-88.148659625168,-10.3563498058901,6.23889219364382));
#34108=CARTESIAN_POINT('Ctrl Pts',(-88.1884445933643,-9.15311464423924,
7.89925625669109));
#34109=CARTESIAN_POINT('Ctrl Pts',(-88.2282295615605,-7.62553833621686,
9.16960457008304));
#34110=CARTESIAN_POINT('Ctrl Pts',(-88.2680145297567,-6.09796202819448,
10.439952883475));
#34111=CARTESIAN_POINT('Ctrl Pts',(-88.307799497953,-4.24604457380059,11.3202854472116));
#34112=CARTESIAN_POINT('Ctrl Pts',(-88.3475844661493,-2.29645093028959,
11.7028541830264));
#34113=CARTESIAN_POINT('Ctrl Pts',(-88.3873694343455,-0.346857286778581,
12.0854229188411));
#34114=CARTESIAN_POINT('Ctrl Pts',(-88.4271544025418,1.70041254584955,11.9702278267339));
#34115=CARTESIAN_POINT('Ctrl Pts',(-88.4669393707381,3.59478350797716,11.3713681849374));
#34116=CARTESIAN_POINT('Ctrl Pts',(-88.5067243389343,5.48915447010478,10.7725085431409));
#34117=CARTESIAN_POINT('Ctrl Pts',(-88.5465093071305,7.23062656173189,9.68998435165513));
#34118=CARTESIAN_POINT('Ctrl Pts',(-88.5862942753268,8.60605275571365,8.25629086835593));
#34119=CARTESIAN_POINT('Ctrl Pts',(-88.626079243523,9.9814789496954,6.82259738505672));
#34120=CARTESIAN_POINT('Ctrl Pts',(-88.6658642117193,10.9908592460318,5.03773460994408));
#34121=CARTESIAN_POINT('Ctrl Pts',(-88.7056491799156,11.5106508088721,3.12016038042581));
#34122=CARTESIAN_POINT('Ctrl Pts',(-88.7454341481119,12.0304423717123,1.20258615090756));
#34123=CARTESIAN_POINT('Ctrl Pts',(-88.7852191163081,12.0606452010564,-0.847699533016319));
#34124=CARTESIAN_POINT('Ctrl Pts',(-88.8250040845044,11.5975626213517,-2.77975252944092));
#34125=CARTESIAN_POINT('Ctrl Pts',(-88.8647890527006,11.134480041647,-4.71180552586556));
#34126=CARTESIAN_POINT('Ctrl Pts',(-88.9045740208969,10.1781120528935,-6.52562583479092));
#34127=CARTESIAN_POINT('Ctrl Pts',(-88.9443589890932,8.84551308397863,-7.99921130042105));
#34128=CARTESIAN_POINT('Ctrl Pts',(-88.9841439572895,7.51291411506383,-9.47279676605115));
#34129=CARTESIAN_POINT('Ctrl Pts',(-89.0239289254857,5.80408416598773,-10.606147388386));
#34130=CARTESIAN_POINT('Ctrl Pts',(-89.0637138936819,3.92817500056627,-11.2605471970953));
#34131=CARTESIAN_POINT('Ctrl Pts',(-89.1034988618782,2.05226583514479,-11.9149470058045));
#34132=CARTESIAN_POINT('Ctrl Pts',(-89.1432838300745,0.00927745337794966,
-12.0903960008881));
#34133=CARTESIAN_POINT('Ctrl Pts',(-89.1830687982707,-1.95073903883306,
-11.7654197631003));
#34134=CARTESIAN_POINT('Ctrl Pts',(-89.222853766467,-3.91075553104407,-11.4404435253125));
#34135=CARTESIAN_POINT('Ctrl Pts',(-89.2626387346633,-5.78780013369925,
-10.6150420546534));
#34136=CARTESIAN_POINT('Ctrl Pts',(-89.3024237028595,-7.35213260967356,
-9.39024094984122));
#34137=CARTESIAN_POINT('Ctrl Pts',(-89.3422086710558,-8.91646508564786,
-8.16543984502907));
#34138=CARTESIAN_POINT('Ctrl Pts',(-89.381993639252,-10.1680854349413,-6.54123910606394));
#34139=CARTESIAN_POINT('Ctrl Pts',(-89.4217786074483,-10.9538015967113,
-4.71643070034976));
#34140=CARTESIAN_POINT('Ctrl Pts',(-89.4541334559149,-11.5927797963778,
-3.23241796578538));
#34141=CARTESIAN_POINT('Ctrl Pts',(-89.4864883043815,-11.9236256264652,
-1.61573049386844));
#34142=CARTESIAN_POINT('Ctrl Pts',(-89.5188431528481,-11.9252862155783,
0.000296729823191094));
#34143=CARTESIAN_POINT('Ctrl Pts',(-89.7311568471519,-11.9248987907529,
0.000229507259365661));
#34144=CARTESIAN_POINT('Ctrl Pts',(-89.7014163268458,-11.9233939941566,
-1.48535772943447));
#34145=CARTESIAN_POINT('Ctrl Pts',(-89.6716758065397,-11.6450321505873,
-2.9714277111775));
#34146=CARTESIAN_POINT('Ctrl Pts',(-89.6419352862337,-11.1027988892476,
-4.35406132175854));
#34147=CARTESIAN_POINT('Ctrl Pts',(-89.6021503180374,-10.3774338709044,
-6.20366024127725));
#34148=CARTESIAN_POINT('Ctrl Pts',(-89.5623653498411,-9.17986094373797,
-7.86815585201252));
#34149=CARTESIAN_POINT('Ctrl Pts',(-89.5225803816448,-7.65660908602565,
-9.14369467174216));
#34150=CARTESIAN_POINT('Ctrl Pts',(-89.4827954134486,-6.13335722831333,
-10.4192334914718));
#34151=CARTESIAN_POINT('Ctrl Pts',(-89.4430104452524,-4.28442644005515,
-11.3058155201958));
#34152=CARTESIAN_POINT('Ctrl Pts',(-89.4032254770561,-2.3361391875209,-11.6949890221749));
#34153=CARTESIAN_POINT('Ctrl Pts',(-89.3634405088599,-0.387851934986667,
-12.0841625241539));
#34154=CARTESIAN_POINT('Ctrl Pts',(-89.3236555406636,1.65979178182363,-11.975927499388));
#34155=CARTESIAN_POINT('Ctrl Pts',(-89.2838705724673,3.55618223645511,-11.3835018375421));
#34156=CARTESIAN_POINT('Ctrl Pts',(-89.244085604271,5.45257269108659,-10.7910761756962));
#34157=CARTESIAN_POINT('Ctrl Pts',(-89.2043006360747,7.19770988353926,-9.71445987677028));
#34158=CARTESIAN_POINT('Ctrl Pts',(-89.1645156678785,8.57799285603494,-8.28543931996323));
#34159=CARTESIAN_POINT('Ctrl Pts',(-89.1247306996822,9.95827582853063,-6.85641876315616));
#34160=CARTESIAN_POINT('Ctrl Pts',(-89.084945731486,10.9737045810693,-5.07499394846794));
#34161=CARTESIAN_POINT('Ctrl Pts',(-89.0451607632897,11.4999985475621,-3.15919506363862));
#34162=CARTESIAN_POINT('Ctrl Pts',(-89.0053757950935,12.0262925140549,-1.2433961788093));
#34163=CARTESIAN_POINT('Ctrl Pts',(-88.9655908268973,12.0634516945017,0.806776776161122));
#34164=CARTESIAN_POINT('Ctrl Pts',(-88.925805858701,11.6069267617573,2.74039011995642));
#34165=CARTESIAN_POINT('Ctrl Pts',(-88.8860208905047,11.150401829013,4.6740034637517));
#34166=CARTESIAN_POINT('Ctrl Pts',(-88.8462359223084,10.2001927830774,6.49105719637186));
#34167=CARTESIAN_POINT('Ctrl Pts',(-88.8064509541121,8.87260081037856,7.96915508324411));
#34168=CARTESIAN_POINT('Ctrl Pts',(-88.7666659859158,7.5450088376797,9.44725297011637));
#34169=CARTESIAN_POINT('Ctrl Pts',(-88.7268810177196,5.84003393821749,10.5863950112407));
#34170=CARTESIAN_POINT('Ctrl Pts',(-88.6870960495234,3.96635578564482,11.2471554480454));
#34171=CARTESIAN_POINT('Ctrl Pts',(-88.6473110813271,2.09267763307216,11.9079158848501));
#34172=CARTESIAN_POINT('Ctrl Pts',(-88.6075261131309,0.0502962273890387,
12.0902947173352));
#34173=CARTESIAN_POINT('Ctrl Pts',(-88.5677411449346,-1.91081155032196,
11.7719701033081));
#34174=CARTESIAN_POINT('Ctrl Pts',(-88.5279561767384,-3.87191932803296,
11.453645489281));
#34175=CARTESIAN_POINT('Ctrl Pts',(-88.4881712085421,-5.75175347777183,
10.6346174287416));
#34176=CARTESIAN_POINT('Ctrl Pts',(-88.4483862403458,-7.32023225262676,
9.41513047179962));
#34177=CARTESIAN_POINT('Ctrl Pts',(-88.4086012721495,-8.88871102748168,
8.19564351485764));
#34178=CARTESIAN_POINT('Ctrl Pts',(-88.3688163039533,-10.1458344274527,
6.57569766151304));
#34179=CARTESIAN_POINT('Ctrl Pts',(-88.3290313357571,-10.9377371277736,
4.75356584986406));
#34180=CARTESIAN_POINT('Ctrl Pts',(-88.296406506222,-11.5871203440395,3.2593648377581));
#34181=CARTESIAN_POINT('Ctrl Pts',(-88.2637816766869,-11.9236670000931,
1.62920435573443));
#34182=CARTESIAN_POINT('Ctrl Pts',(-88.2311568471518,-11.9253287759226,
-0.000290940587986354));
#34183=CARTESIAN_POINT('Origin',(-85.75,0.,0.));
#34184=CARTESIAN_POINT('',(-86.5188431528481,-11.9244727711418,0.000275034636322557));
#34185=CARTESIAN_POINT('',(-86.7311568471519,-11.9241833131278,0.00019535608514432));
#34186=CARTESIAN_POINT('',(-85.75,-11.925,-1.46039130798322E-15));
#34187=CARTESIAN_POINT('Ctrl Pts',(-86.5188431528481,-11.9244727711418,
0.000275034636322557));
#34188=CARTESIAN_POINT('Ctrl Pts',(-86.5316490676713,-11.925012519502,0.640017395537692));
#34189=CARTESIAN_POINT('Ctrl Pts',(-86.5444549824944,-11.8744209897277,
1.27967524169772));
#34190=CARTESIAN_POINT('Ctrl Pts',(-86.5572608973175,-11.771953842827,1.9109122468146));
#34191=CARTESIAN_POINT('Ctrl Pts',(-86.5970458655138,-11.4536124953399,
3.87201729239096));
#34192=CARTESIAN_POINT('Ctrl Pts',(-86.6368308337101,-10.6345682683525,
5.75184447388234));
#34193=CARTESIAN_POINT('Ctrl Pts',(-86.6766158019064,-9.41506786773371,
7.32031283065446));
#34194=CARTESIAN_POINT('Ctrl Pts',(-86.7164007701026,-8.1955674671149,8.88878118742658));
#34195=CARTESIAN_POINT('Ctrl Pts',(-86.7561857382989,-6.57561089286461,
10.1458907194795));
#34196=CARTESIAN_POINT('Ctrl Pts',(-86.7959707064951,-4.75347231000134,
10.9377778314759));
#34197=CARTESIAN_POINT('Ctrl Pts',(-86.8357556746914,-2.93133372713806,
11.7296649434723));
#34198=CARTESIAN_POINT('Ctrl Pts',(-86.8755406428876,-0.907013135661791,
12.0563296354123));
#34199=CARTESIAN_POINT('Ctrl Pts',(-86.9153256110839,1.07172327033036,11.8777898669959));
#34200=CARTESIAN_POINT('Ctrl Pts',(-86.9551105792802,3.0504596763225,11.6992500985794));
#34201=CARTESIAN_POINT('Ctrl Pts',(-86.9948955474764,4.98361189683049,11.0155058698065));
#34202=CARTESIAN_POINT('Ctrl Pts',(-87.0346805156727,6.63457226689149,9.9102438783345));
#34203=CARTESIAN_POINT('Ctrl Pts',(-87.0744654838689,8.28553263695249,8.80498188686248));
#34204=CARTESIAN_POINT('Ctrl Pts',(-87.1142504520652,9.6543011565665,7.27820213269135));
#34205=CARTESIAN_POINT('Ctrl Pts',(-87.1540354202615,10.573347757555,5.51677442809552));
#34206=CARTESIAN_POINT('Ctrl Pts',(-87.1938203884578,11.4923943585434,3.75534672349969));
#34207=CARTESIAN_POINT('Ctrl Pts',(-87.233605356654,11.9617190409063,1.75927106847916));
#34208=CARTESIAN_POINT('Ctrl Pts',(-87.2733903248502,11.9238789317937,-0.227143374542267));
#34209=CARTESIAN_POINT('Ctrl Pts',(-87.3131752930465,11.8860388226812,-2.21355781756369));
#34210=CARTESIAN_POINT('Ctrl Pts',(-87.3529602612428,11.3410339220931,-4.19031104858601));
#34211=CARTESIAN_POINT('Ctrl Pts',(-87.392745229439,10.3555699635724,-5.91545886827222));
#34212=CARTESIAN_POINT('Ctrl Pts',(-87.4325301976353,9.37010600505178,-7.64060668795844));
#34213=CARTESIAN_POINT('Ctrl Pts',(-87.4723151658315,7.94418298859856,-9.11414909630856));
#34214=CARTESIAN_POINT('Ctrl Pts',(-87.5121001340278,6.25232639222003,-10.1557322521756));
#34215=CARTESIAN_POINT('Ctrl Pts',(-87.551885102224,4.56046979584153,-11.1973154080427));
#34216=CARTESIAN_POINT('Ctrl Pts',(-87.5916700704203,2.60267961953774,-11.8069393114268));
#34217=CARTESIAN_POINT('Ctrl Pts',(-87.6314550386166,0.618579084479763,
-11.9099892027141));
#34218=CARTESIAN_POINT('Ctrl Pts',(-87.6712400068129,-1.36552145057824,
-12.0130390940015));
#34219=CARTESIAN_POINT('Ctrl Pts',(-87.7110249750091,-3.37593234439042,
-11.6095149731922));
#34220=CARTESIAN_POINT('Ctrl Pts',(-87.7508099432054,-5.16658987668869,
-10.748806070401));
#34221=CARTESIAN_POINT('Ctrl Pts',(-87.7905949114016,-6.95724740898696,
-9.88809716760979));
#34222=CARTESIAN_POINT('Ctrl Pts',(-87.8303798795979,-8.52815157977131,
-8.57020348283671));
#34223=CARTESIAN_POINT('Ctrl Pts',(-87.8701648477942,-9.68703198025464,
-6.95642827216015));
#34224=CARTESIAN_POINT('Ctrl Pts',(-87.9099498159904,-10.845912380738,-5.34265306148359));
#34225=CARTESIAN_POINT('Ctrl Pts',(-87.9497347841867,-11.5927690109203,
-3.43299632490356));
#34226=CARTESIAN_POINT('Ctrl Pts',(-87.9895197523829,-11.8361905470845,
-1.46119000346019));
#34227=CARTESIAN_POINT('Ctrl Pts',(-87.9992942192047,-11.8959949364508,
-0.976751876658961));
#34228=CARTESIAN_POINT('Ctrl Pts',(-88.0090686860264,-11.9254120610665,
-0.488562410485842));
#34229=CARTESIAN_POINT('Ctrl Pts',(-88.0188431528482,-11.9249138545732,
-0.000313305576115086));
#34230=CARTESIAN_POINT('Ctrl Pts',(-88.2311568471518,-11.9253287759226,
-0.000290940587986354));
#34231=CARTESIAN_POINT('Ctrl Pts',(-88.2239967084906,-11.9256934841995,
-0.357914641177949));
#34232=CARTESIAN_POINT('Ctrl Pts',(-88.2168365698294,-11.9099279125869,
-0.715506302006868));
#34233=CARTESIAN_POINT('Ctrl Pts',(-88.2096764311682,-11.8777989864306,
-1.07162165229349));
#34234=CARTESIAN_POINT('Ctrl Pts',(-88.169891462972,-11.6992761440956,-3.05035957284871));
#34235=CARTESIAN_POINT('Ctrl Pts',(-88.1301064947758,-11.0155484587548,
-4.98351764400581));
#34236=CARTESIAN_POINT('Ctrl Pts',(-88.0903215265795,-9.91030059580027,
-6.63448746494451));
#34237=CARTESIAN_POINT('Ctrl Pts',(-88.0505365583832,-8.80505273284578,
-8.28545728588321));
#34238=CARTESIAN_POINT('Ctrl Pts',(-88.010751590187,-7.27828469227764,-9.65423885660352));
#34239=CARTESIAN_POINT('Ctrl Pts',(-87.9709666219907,-5.51686485626861,
-10.5733005210593));
#34240=CARTESIAN_POINT('Ctrl Pts',(-87.9311816537944,-3.75544502025959,
-11.492362185515));
#34241=CARTESIAN_POINT('Ctrl Pts',(-87.8913966855982,-1.75937338880969,
-11.9617039437062));
#34242=CARTESIAN_POINT('Ctrl Pts',(-87.8516117174019,0.227041369848316,
-11.9238808282072));
#34243=CARTESIAN_POINT('Ctrl Pts',(-87.8118267492057,2.21345612850632,-11.8860577127083));
#34244=CARTESIAN_POINT('Ctrl Pts',(-87.7720417810094,4.19021401437242,-11.3410697235191));
#34245=CARTESIAN_POINT('Ctrl Pts',(-87.7322568128131,5.91537025754448,-10.3556205265248));
#34246=CARTESIAN_POINT('Ctrl Pts',(-87.6924718446169,7.64052650071656,-9.37017132953037));
#34247=CARTESIAN_POINT('Ctrl Pts',(-87.6526868764206,9.11408110119458,-7.94426092473072));
#34248=CARTESIAN_POINT('Ctrl Pts',(-87.6129019082243,10.1556787259928,-6.25241324546769));
#34249=CARTESIAN_POINT('Ctrl Pts',(-87.5731169400281,11.1972763507911,-4.56056556620466));
#34250=CARTESIAN_POINT('Ctrl Pts',(-87.5333319718319,11.8069169999095,-2.60278061247826));
#34251=CARTESIAN_POINT('Ctrl Pts',(-87.4935470036356,11.9099838639235,-0.618680966760705));
#34252=CARTESIAN_POINT('Ctrl Pts',(-87.4537620354393,12.0130507279375,1.36541867895684));
#34253=CARTESIAN_POINT('Ctrl Pts',(-87.413977067243,11.6095438068471,3.37583301666555));
#34254=CARTESIAN_POINT('Ctrl Pts',(-87.3741920990468,10.7488502257642,5.16649790484009));
#34255=CARTESIAN_POINT('Ctrl Pts',(-87.3344071308505,9.88815664468133,6.95716279301464));
#34256=CARTESIAN_POINT('Ctrl Pts',(-87.2946221626543,8.57027640360599,8.52807823165505));
#34257=CARTESIAN_POINT('Ctrl Pts',(-87.2548371944581,6.95651111301019,9.68697243270591));
#34258=CARTESIAN_POINT('Ctrl Pts',(-87.2150522262618,5.34274582241438,10.8458666337568));
#34259=CARTESIAN_POINT('Ctrl Pts',(-87.1752672580655,3.4330954822981,11.5927395972181));
#34260=CARTESIAN_POINT('Ctrl Pts',(-87.1354822898692,1.46129125108685,11.8361780003709));
#34261=CARTESIAN_POINT('Ctrl Pts',(-87.0956973216729,-0.510512980124398,
12.0796164035238));
#34262=CARTESIAN_POINT('Ctrl Pts',(-87.0559123534767,-2.54447110243062,
11.8196202463681));
#34263=CARTESIAN_POINT('Ctrl Pts',(-87.0161273852804,-4.3916373386571,11.0880116911415));
#34264=CARTESIAN_POINT('Ctrl Pts',(-86.9763424170842,-6.23880357488359,
10.3564031359149));
#34265=CARTESIAN_POINT('Ctrl Pts',(-86.936557448888,-7.89917792503034,9.15318218261725));
#34266=CARTESIAN_POINT('Ctrl Pts',(-86.8967724806917,-9.16953930086925,
7.6256167479702));
#34267=CARTESIAN_POINT('Ctrl Pts',(-86.8569875124955,-10.4399006767081,
6.09805131332317));
#34268=CARTESIAN_POINT('Ctrl Pts',(-86.8172025442992,-11.3202490782392,
4.24614139732673));
#34269=CARTESIAN_POINT('Ctrl Pts',(-86.7774175761029,-11.7028344910425,
2.29655103413447));
#34270=CARTESIAN_POINT('Ctrl Pts',(-86.7619973331192,-11.851120647722,1.54090993444184));
#34271=CARTESIAN_POINT('Ctrl Pts',(-86.7465770901356,-11.9246299821493,
0.770594715534088));
#34272=CARTESIAN_POINT('Ctrl Pts',(-86.7311568471519,-11.9241833131278,
0.00019535608514432));
#34273=CARTESIAN_POINT('Origin',(-85.75,0.,0.));
#34274=CARTESIAN_POINT('',(-85.0188431528481,-11.9257267375167,-0.000211608777844763));
#34275=CARTESIAN_POINT('',(-85.2311568471519,-11.9259825692636,-9.38362929313221E-5));
#34276=CARTESIAN_POINT('',(-85.75,-11.925,-1.46039130798322E-15));
#34277=CARTESIAN_POINT('Ctrl Pts',(-85.0188431528481,-11.9257267375167,
-0.000211608777844763));
#34278=CARTESIAN_POINT('Ctrl Pts',(-85.0542294493162,-11.9242705478464,
1.7670388487699));
#34279=CARTESIAN_POINT('Ctrl Pts',(-85.0896157457842,-11.5263826191068,
3.53492306196897));
#34280=CARTESIAN_POINT('Ctrl Pts',(-85.1250020422522,-10.7662288870872,
5.13018503014497));
#34281=CARTESIAN_POINT('Ctrl Pts',(-85.1647870104484,-9.91158471487207,
6.92374505205773));
#34282=CARTESIAN_POINT('Ctrl Pts',(-85.2045719786447,-8.5990147066321,8.49910013949158));
#34283=CARTESIAN_POINT('Ctrl Pts',(-85.244356946841,-6.98917052831226,9.66343511484645));
#34284=CARTESIAN_POINT('Ctrl Pts',(-85.2841419150372,-5.37932634999243,
10.8277700902013));
#34285=CARTESIAN_POINT('Ctrl Pts',(-85.3239268832335,-3.47220800159274,
11.5810849534772));
#34286=CARTESIAN_POINT('Ctrl Pts',(-85.3637118514297,-1.50123673904742,
11.83117792724));
#34287=CARTESIAN_POINT('Ctrl Pts',(-85.403496819626,0.469734523497902,12.0812709010027));
#34288=CARTESIAN_POINT('Ctrl Pts',(-85.4432817878222,2.50455870018884,11.8281419852523));
#34289=CARTESIAN_POINT('Ctrl Pts',(-85.4830667560185,4.35418401333848,11.102772828022));
#34290=CARTESIAN_POINT('Ctrl Pts',(-85.5228517242148,6.20380932648811,10.3774036707916));
#34291=CARTESIAN_POINT('Ctrl Pts',(-85.562636692411,7.86823577609642,9.17979427208133));
#34292=CARTESIAN_POINT('Ctrl Pts',(-85.6024216606073,9.14374631827695,7.65652572383014));
#34293=CARTESIAN_POINT('Ctrl Pts',(-85.6422066288036,10.4192568604575,6.13325717557897));
#34294=CARTESIAN_POINT('Ctrl Pts',(-85.6819915969998,11.3058514952102,4.28432947778694));
#34295=CARTESIAN_POINT('Ctrl Pts',(-85.7217765651961,11.6950157020167,2.33604165678988));
#34296=CARTESIAN_POINT('Ctrl Pts',(-85.7615615333924,12.0841799088233,0.38775383579276));
#34297=CARTESIAN_POINT('Ctrl Pts',(-85.8013465015887,11.9759136876837,-1.65989410840939));
#34298=CARTESIAN_POINT('Ctrl Pts',(-85.8411314697849,11.383468254672,-3.55628083642892));
#34299=CARTESIAN_POINT('Ctrl Pts',(-85.8809164379812,10.7910228216603,-5.4526675644484));
#34300=CARTESIAN_POINT('Ctrl Pts',(-85.9207014061774,9.71439817677659,-7.19779307628529));
#34301=CARTESIAN_POINT('Ctrl Pts',(-85.9604863743736,8.28536751437418,-8.57806318724856));
#34302=CARTESIAN_POINT('Ctrl Pts',(-86.0002713425699,6.85633685197174,-9.95833329821186));
#34303=CARTESIAN_POINT('Ctrl Pts',(-86.0400563107662,5.07490017205052,-10.9737480083016));
#34304=CARTESIAN_POINT('Ctrl Pts',(-86.0798412789624,3.15909595530759,-11.500025897268));
#34305=CARTESIAN_POINT('Ctrl Pts',(-86.1196262471587,1.24329173856466,-12.0263037862345));
#34306=CARTESIAN_POINT('Ctrl Pts',(-86.1594112153549,-0.806880015000012,
-12.0634448540777));
#34307=CARTESIAN_POINT('Ctrl Pts',(-86.1991961835512,-2.74048906500605,
-11.6069032294259));
#34308=CARTESIAN_POINT('Ctrl Pts',(-86.2389811517475,-4.67409811501208,
-11.1503616047741));
#34309=CARTESIAN_POINT('Ctrl Pts',(-86.2787661199437,-6.49114446145946,
-10.2001372876273));
#34310=CARTESIAN_POINT('Ctrl Pts',(-86.31855108814,-7.96923118774666,-8.8725327369879));
#34311=CARTESIAN_POINT('Ctrl Pts',(-86.3583360563363,-9.44731791403387,
-7.54492818634847));
#34312=CARTESIAN_POINT('Ctrl Pts',(-86.3981210245325,-10.5864450201609,
-5.83994340221645));
#34313=CARTESIAN_POINT('Ctrl Pts',(-86.4379059927288,-11.247189339231,-3.96625955531976));
#34314=CARTESIAN_POINT('Ctrl Pts',(-86.4648850461019,-11.6952544517187,
-2.69567373354868));
#34315=CARTESIAN_POINT('Ctrl Pts',(-86.491864099475,-11.923335648178,-1.34751179185571));
#34316=CARTESIAN_POINT('Ctrl Pts',(-86.5188431528481,-11.9244727711418,
0.000275034636322557));
#34317=CARTESIAN_POINT('Ctrl Pts',(-86.7311568471519,-11.9241833131278,
0.00019535608514432));
#34318=CARTESIAN_POINT('Ctrl Pts',(-86.7067921219393,-11.923477554601,-1.21707266730429));
#34319=CARTESIAN_POINT('Ctrl Pts',(-86.6824273967267,-11.7381367941709,
-2.43455075192281));
#34320=CARTESIAN_POINT('Ctrl Pts',(-86.6580626715141,-11.3713988928199,
-3.59468621683454));
#34321=CARTESIAN_POINT('Ctrl Pts',(-86.6182777033178,-10.7725554577184,
-5.48906229422317));
#34322=CARTESIAN_POINT('Ctrl Pts',(-86.5784927351216,-9.69004616343957,
-7.23054363861233));
#34323=CARTESIAN_POINT('Ctrl Pts',(-86.5387077669254,-8.25636445447486,
-8.60598209224268));
#34324=CARTESIAN_POINT('Ctrl Pts',(-86.4989227987291,-6.82268274551014,
-9.98142054587304));
#34325=CARTESIAN_POINT('Ctrl Pts',(-86.4591378305328,-5.0378286218595,-10.9908161087446));
#34326=CARTESIAN_POINT('Ctrl Pts',(-86.4193528623365,-3.12025884135912,
-11.5106240725707));
#34327=CARTESIAN_POINT('Ctrl Pts',(-86.3795678941403,-1.20268906085873,
-12.0304320363968));
#34328=CARTESIAN_POINT('Ctrl Pts',(-86.3397829259441,0.847596376491398,
-12.0606524011774));
#34329=CARTESIAN_POINT('Ctrl Pts',(-86.2999979577478,2.77965331601329,-11.5975863531985));
#34330=CARTESIAN_POINT('Ctrl Pts',(-86.2602129895515,4.71171025553519,-11.1345203052197));
#34331=CARTESIAN_POINT('Ctrl Pts',(-86.2204280213552,6.52553869722884,-10.1781678444814));
#34332=CARTESIAN_POINT('Ctrl Pts',(-86.180643053159,7.99913557911104,-8.84558148253248));
#34333=CARTESIAN_POINT('Ctrl Pts',(-86.1408580849627,9.47273246099324,-7.51299512058353));
#34334=CARTESIAN_POINT('Ctrl Pts',(-86.1010731167665,10.606097783064,-5.80417485742391));
#34335=CARTESIAN_POINT('Ctrl Pts',(-86.0612881485702,11.2605135904926,-3.92827130624306));
#34336=CARTESIAN_POINT('Ctrl Pts',(-86.021503180374,11.9149293979212,-2.05236775506224));
#34337=CARTESIAN_POINT('Ctrl Pts',(-85.9817182121776,12.0903956907077,-0.00938091586017931));
#34338=CARTESIAN_POINT('Ctrl Pts',(-85.9419332439814,11.7654363174268,1.95063836671386));
#34339=CARTESIAN_POINT('Ctrl Pts',(-85.9021482757851,11.4404769441458,3.91065764928794));
#34340=CARTESIAN_POINT('Ctrl Pts',(-85.8623633075889,10.6150919047974,5.78770937523399));
#34341=CARTESIAN_POINT('Ctrl Pts',(-85.8225783393926,9.3903039873357,7.35205228507991));
#34342=CARTESIAN_POINT('Ctrl Pts',(-85.7827933711964,8.165516069874,8.91639519492582));
#34343=CARTESIAN_POINT('Ctrl Pts',(-85.7430084030001,6.54132527429904,10.1680292886716));
#34344=CARTESIAN_POINT('Ctrl Pts',(-85.7032234348038,4.71652401205079,10.9537611358323));
#34345=CARTESIAN_POINT('Ctrl Pts',(-85.6634384666076,2.89172274980254,11.739492982993));
#34346=CARTESIAN_POINT('Ctrl Pts',(-85.6236534984113,0.866311020881004,
12.0593225835686));
#34347=CARTESIAN_POINT('Ctrl Pts',(-85.5838685302151,-1.1118114311319,11.8741044764953));
#34348=CARTESIAN_POINT('Ctrl Pts',(-85.5440835620188,-3.0899338831448,11.688886369422));
#34349=CARTESIAN_POINT('Ctrl Pts',(-85.5042985938226,-5.02076705824908,
10.9986205546999));
#34350=CARTESIAN_POINT('Ctrl Pts',(-85.4645136256263,-6.66798713044286,
9.88779193780744));
#34351=CARTESIAN_POINT('Ctrl Pts',(-85.4247286574301,-8.31520720263664,
8.77696332091496));
#34352=CARTESIAN_POINT('Ctrl Pts',(-85.3849436892338,-9.67881417191992,
7.24557190185211));
#34353=CARTESIAN_POINT('Ctrl Pts',(-85.3451587210375,-10.5919097167293,
5.48105193642395));
#34354=CARTESIAN_POINT('Ctrl Pts',(-85.3071580964089,-11.4640532076362,
3.79567014787885));
#34355=CARTESIAN_POINT('Ctrl Pts',(-85.2691574717804,-11.9251896698631,
1.8976023630708));
#34356=CARTESIAN_POINT('Ctrl Pts',(-85.2311568471519,-11.9259825692636,
-9.38362929313221E-5));
#34357=CARTESIAN_POINT('Origin',(-85.75,0.,0.));
#34358=CARTESIAN_POINT('',(-83.5188431528481,-11.9240088006309,7.96196756353007E-5));
#34359=CARTESIAN_POINT('',(-83.7311568471519,-11.9239866250219,-4.23754525262851E-5));
#34360=CARTESIAN_POINT('',(-85.75,-11.925,-1.46039130798322E-15));
#34361=CARTESIAN_POINT('Ctrl Pts',(-83.5188431528481,-11.9240088006309,
7.96196756353007E-5));
#34362=CARTESIAN_POINT('Ctrl Pts',(-83.5370248627648,-11.9242195872713,
0.908480640254555));
#34363=CARTESIAN_POINT('Ctrl Pts',(-83.5552065726814,-11.8217585988444,
1.81683486812291));
#34364=CARTESIAN_POINT('Ctrl Pts',(-83.573388282598,-11.6161109140083,2.70119420587685));
#34365=CARTESIAN_POINT('Ctrl Pts',(-83.6131732507943,-11.166115471426,4.63633717581385));
#34366=CARTESIAN_POINT('Ctrl Pts',(-83.6529582189906,-10.2220456992873,
6.45658879193667));
#34367=CARTESIAN_POINT('Ctrl Pts',(-83.6927431871868,-8.89945077497426,
7.93915982913878));
#34368=CARTESIAN_POINT('Ctrl Pts',(-83.7325281553831,-7.57685585066127,
9.42173086634086));
#34369=CARTESIAN_POINT('Ctrl Pts',(-83.7723131235793,-5.87573577417402,
10.5666213246222));
#34370=CARTESIAN_POINT('Ctrl Pts',(-83.8120980917756,-4.00429869523271,
11.2337026332634));
#34371=CARTESIAN_POINT('Ctrl Pts',(-83.8518830599718,-2.13286161629138,
11.9007839419046));
#34372=CARTESIAN_POINT('Ctrl Pts',(-83.8916680281681,-0.0911075348959658,
12.0900561009056));
#34373=CARTESIAN_POINT('Ctrl Pts',(-83.9314529963644,1.87106358683858,11.7783531933421));
#34374=CARTESIAN_POINT('Ctrl Pts',(-83.9712379645607,3.83323470857312,11.4666502857785));
#34375=CARTESIAN_POINT('Ctrl Pts',(-84.0110229327569,5.7158228706468,10.6539723116505));
#34376=CARTESIAN_POINT('Ctrl Pts',(-84.0508079009531,7.28840918318163,9.4397867809977));
#34377=CARTESIAN_POINT('Ctrl Pts',(-84.0905928691494,8.86099549571648,8.22560125034485));
#34378=CARTESIAN_POINT('Ctrl Pts',(-84.1303778373456,10.1235799587125,6.60990816316717));
#34379=CARTESIAN_POINT('Ctrl Pts',(-84.1701628055419,10.9216288739539,4.79045985606893));
#34380=CARTESIAN_POINT('Ctrl Pts',(-84.2099477737382,11.7196777891953,2.97101154897075));
#34381=CARTESIAN_POINT('Ctrl Pts',(-84.2497327419345,12.0531911566822,0.94780802195201));
#34382=CARTESIAN_POINT('Ctrl Pts',(-84.2895177101307,11.8813486943064,-1.03152125369576));
#34383=CARTESIAN_POINT('Ctrl Pts',(-84.329302678327,11.7095062319307,-3.01085052934356));
#34384=CARTESIAN_POINT('Ctrl Pts',(-84.3690876465232,11.0323079396923,-4.94630555362038));
#34385=CARTESIAN_POINT('Ctrl Pts',(-84.4088726147195,9.93263932701359,-6.60099681049727));
#34386=CARTESIAN_POINT('Ctrl Pts',(-84.4486575829157,8.83297071433485,-8.25568806737415));
#34387=CARTESIAN_POINT('Ctrl Pts',(-84.488442551112,7.31083178121576,-9.62961555685108));
#34388=CARTESIAN_POINT('Ctrl Pts',(-84.5282275193082,5.55252432785638,-10.5546177799685));
#34389=CARTESIAN_POINT('Ctrl Pts',(-84.5680124875045,3.794216874497,-11.4796200030859));
#34390=CARTESIAN_POINT('Ctrl Pts',(-84.6077974557008,1.79974090089733,-11.9556969598438));
#34391=CARTESIAN_POINT('Ctrl Pts',(-84.6475824238971,-0.186790223121584,
-11.9245793345182));
#34392=CARTESIAN_POINT('Ctrl Pts',(-84.6873673920933,-2.1733213471405,-11.8934617091927));
#34393=CARTESIAN_POINT('Ctrl Pts',(-84.7271523602896,-4.15190762157867,
-11.3551495017836));
#34394=CARTESIAN_POINT('Ctrl Pts',(-84.7669373284859,-5.88038049221546,
-10.3755292953879));
#34395=CARTESIAN_POINT('Ctrl Pts',(-84.8067222966821,-7.60885336285225,
-9.3959090889922));
#34396=CARTESIAN_POINT('Ctrl Pts',(-84.8465072648784,-9.08721282968765,
-7.97498088360977));
#34397=CARTESIAN_POINT('Ctrl Pts',(-84.8862922330746,-10.1345154689654,
-6.28665881863918));
#34398=CARTESIAN_POINT('Ctrl Pts',(-84.9260772012709,-11.1818181082431,
-4.59833675366858));
#34399=CARTESIAN_POINT('Ctrl Pts',(-84.9658621694672,-11.7980639199631,
-2.64262082910982));
#34400=CARTESIAN_POINT('Ctrl Pts',(-85.0056471376634,-11.9078276577279,
-0.658880388634596));
#34401=CARTESIAN_POINT('Ctrl Pts',(-85.0100458093917,-11.9199632625049,
-0.439555769631561));
#34402=CARTESIAN_POINT('Ctrl Pts',(-85.0144444811199,-11.9259077482744,
-0.219888585467614));
#34403=CARTESIAN_POINT('Ctrl Pts',(-85.0188431528481,-11.9257267375167,
-0.000211608777844763));
#34404=CARTESIAN_POINT('Ctrl Pts',(-85.2311568471519,-11.9259825692636,
-9.38362929313221E-5));
#34405=CARTESIAN_POINT('Ctrl Pts',(-85.2293725035842,-11.9260198003607,
-0.0892013717583456));
#34406=CARTESIAN_POINT('Ctrl Pts',(-85.2275881600165,-11.9250420512741,
-0.17830808794031));
#34407=CARTESIAN_POINT('Ctrl Pts',(-85.2258038164487,-11.9230442142274,
-0.267391927138796));
#34408=CARTESIAN_POINT('Ctrl Pts',(-85.1860188482525,-11.8784990465807,
-2.25366731347994));
#34409=CARTESIAN_POINT('Ctrl Pts',(-85.1462338800562,-11.3268245909518,
-4.22856957436877));
#34410=CARTESIAN_POINT('Ctrl Pts',(-85.1064489118599,-10.3355428993453,
-5.95038105947133));
#34411=CARTESIAN_POINT('Ctrl Pts',(-85.0666639436637,-9.34426120773877,
-7.6721925445739));
#34412=CARTESIAN_POINT('Ctrl Pts',(-85.0268789754674,-7.9133722801547,-9.14091325389021));
#34413=CARTESIAN_POINT('Ctrl Pts',(-84.9870940072712,-6.21800939600349,
-10.1767794968906));
#34414=CARTESIAN_POINT('Ctrl Pts',(-84.947309039075,-4.52264651185229,-11.212645739891));
#34415=CARTESIAN_POINT('Ctrl Pts',(-84.9075240708787,-2.56280967113394,
-11.8156575165756));
#34416=CARTESIAN_POINT('Ctrl Pts',(-84.8677391026824,-0.578372595985458,
-11.9120093568354));
#34417=CARTESIAN_POINT('Ctrl Pts',(-84.8279541344861,1.40606447916304,-12.0083611970952));
#34418=CARTESIAN_POINT('Ctrl Pts',(-84.7881691662899,3.41510178874168,-11.5980531009304));
#34419=CARTESIAN_POINT('Ctrl Pts',(-84.7483841980936,5.20284373197974,-10.7313046214205));
#34420=CARTESIAN_POINT('Ctrl Pts',(-84.7085992298973,6.99058567521779,-9.86455614191062));
#34421=CARTESIAN_POINT('Ctrl Pts',(-84.6688142617011,8.55703225211528,-8.54136727905574));
#34422=CARTESIAN_POINT('Ctrl Pts',(-84.6290292935048,9.71045863991032,-6.92368939075921));
#34423=CARTESIAN_POINT('Ctrl Pts',(-84.5892443253086,10.8638850277054,-5.30601150246268));
#34424=CARTESIAN_POINT('Ctrl Pts',(-84.5494593571123,11.6042912263979,-3.39384458872447));
#34425=CARTESIAN_POINT('Ctrl Pts',(-84.509674388916,11.8410554112094,-1.4212278233248));
#34426=CARTESIAN_POINT('Ctrl Pts',(-84.4698894207198,12.0778195960208,0.551388942074894));
#34427=CARTESIAN_POINT('Ctrl Pts',(-84.4301044525235,11.8109417669511,2.58445555913603));
#34428=CARTESIAN_POINT('Ctrl Pts',(-84.3903194843273,11.0730863667161,4.42913536622702));
#34429=CARTESIAN_POINT('Ctrl Pts',(-84.350534516131,10.3352309664812,6.27381517331799));
#34430=CARTESIAN_POINT('Ctrl Pts',(-84.3107495479347,9.12639799508108,7.93010817043879));
#34431=CARTESIAN_POINT('Ctrl Pts',(-84.2709645797385,7.59454225072356,9.19529280551203));
#34432=CARTESIAN_POINT('Ctrl Pts',(-84.2311796115422,6.06268650636603,10.4604774405853));
#34433=CARTESIAN_POINT('Ctrl Pts',(-84.191394643346,4.20780798905109,11.334553713611));
#34434=CARTESIAN_POINT('Ctrl Pts',(-84.1516096751497,2.25693407413093,11.7105392857095));
#34435=CARTESIAN_POINT('Ctrl Pts',(-84.1118247069535,0.30606015921078,12.086524857808));
#34436=CARTESIAN_POINT('Ctrl Pts',(-84.0720397387572,-1.74080915331459,
11.9644197289793));
#34437=CARTESIAN_POINT('Ctrl Pts',(-84.032254770561,-3.63314782448661,11.3591689248174));
#34438=CARTESIAN_POINT('Ctrl Pts',(-83.9924698023647,-5.52548649565861,
10.7539181206555));
#34439=CARTESIAN_POINT('Ctrl Pts',(-83.9526848341684,-7.26329452547726,
9.66552164116037));
#34440=CARTESIAN_POINT('Ctrl Pts',(-83.9128998659722,-8.63387335055236,
8.22719349133102));
#34441=CARTESIAN_POINT('Ctrl Pts',(-83.8731148977759,-10.0044521756275,
6.78886534150164));
#34442=CARTESIAN_POINT('Ctrl Pts',(-83.8333299295796,-11.0078017959591,
5.00060552133803));
#34443=CARTESIAN_POINT('Ctrl Pts',(-83.7935449613834,-11.5211174948606,
3.0812876280193));
#34444=CARTESIAN_POINT('Ctrl Pts',(-83.7727489233062,-11.7894332257493,
2.07803917009065));
#34445=CARTESIAN_POINT('Ctrl Pts',(-83.751952885229,-11.9238585928665,1.03898214397406));
#34446=CARTESIAN_POINT('Ctrl Pts',(-83.7311568471519,-11.9239866250219,
-4.23754525262852E-5));
#34447=CARTESIAN_POINT('Origin',(-85.75,0.,0.));
#34448=CARTESIAN_POINT('',(-82.0188431528482,-11.9260172048445,5.30405712340781E-5));
#34449=CARTESIAN_POINT('',(-82.2311568471519,-11.9258224962353,0.000178908662697473));
#34450=CARTESIAN_POINT('',(-85.75,-11.925,-1.46039130798322E-15));
#34451=CARTESIAN_POINT('Ctrl Pts',(-82.0188431528482,-11.9260172048445,
5.30405712340781E-5));
#34452=CARTESIAN_POINT('Ctrl Pts',(-82.0198202762134,-11.9260288816802,
0.0488487122931931));
#34453=CARTESIAN_POINT('Ctrl Pts',(-82.0207973995787,-11.925735492526,0.0976442386766466));
#34454=CARTESIAN_POINT('Ctrl Pts',(-82.0217745229439,-11.9251361629207,
0.146436006056953));
#34455=CARTESIAN_POINT('Ctrl Pts',(-82.0615594911402,-11.900733605235,2.13306224232621));
#34456=CARTESIAN_POINT('Ctrl Pts',(-82.1013444593364,-11.3691346776982,
4.1134567013229));
#34457=CARTESIAN_POINT('Ctrl Pts',(-82.1411294275327,-10.3953731816262,
5.84523425748872));
#34458=CARTESIAN_POINT('Ctrl Pts',(-82.1809143957289,-9.42161168555416,
7.57701181365452));
#34459=CARTESIAN_POINT('Ctrl Pts',(-82.2206993639251,-8.00568762094685,
9.06017246698947));
#34460=CARTESIAN_POINT('Ctrl Pts',(-82.2604843321214,-6.32091762223773,
10.1131828701275));
#34461=CARTESIAN_POINT('Ctrl Pts',(-82.3002693003177,-4.63614762352858,
11.1661932732656));
#34462=CARTESIAN_POINT('Ctrl Pts',(-82.340054268514,-2.68253169071761,11.7890534262067));
#34463=CARTESIAN_POINT('Ctrl Pts',(-82.3798392367102,-0.699174929923869,
11.9055296212553));
#34464=CARTESIAN_POINT('Ctrl Pts',(-82.4196242049065,1.28418183086987,12.0220058163039));
#34465=CARTESIAN_POINT('Ctrl Pts',(-82.4594091731028,3.29727941964638,11.6320980534599));
#34466=CARTESIAN_POINT('Ctrl Pts',(-82.499194141299,5.09372180800857,10.7835284630743));
#34467=CARTESIAN_POINT('Ctrl Pts',(-82.5389791094953,6.89016419637075,9.9349588726887));
#34468=CARTESIAN_POINT('Ctrl Pts',(-82.5787640776915,8.46995138431862,8.62772745476145));
#34469=CARTESIAN_POINT('Ctrl Pts',(-82.6185490458878,9.63972739936108,7.02183271463421));
#34470=CARTESIAN_POINT('Ctrl Pts',(-82.658334014084,10.8095034144035,5.41593797450697));
#34471=CARTESIAN_POINT('Ctrl Pts',(-82.6981189822803,11.5692682565406,3.51137991217972));
#34472=CARTESIAN_POINT('Ctrl Pts',(-82.7379039504766,11.8260299004481,1.54126629538404));
#34473=CARTESIAN_POINT('Ctrl Pts',(-82.7776889186728,12.0827915443555,-0.428847321411644));
#34474=CARTESIAN_POINT('Ctrl Pts',(-82.8174738868691,11.8365499900335,-2.46451649267577));
#34475=CARTESIAN_POINT('Ctrl Pts',(-82.8572588550654,11.1174442959487,-4.31658595878279));
#34476=CARTESIAN_POINT('Ctrl Pts',(-82.8970438232616,10.398338601864,-6.1686554248898));
#34477=CARTESIAN_POINT('Ctrl Pts',(-82.9368287914578,9.20636876801659,-7.83712518583971));
#34478=CARTESIAN_POINT('Ctrl Pts',(-82.9766137596541,7.68742544683738,-9.11778334612848));
#34479=CARTESIAN_POINT('Ctrl Pts',(-83.0163987278503,6.16848212565817,-10.3984415064173));
#34480=CARTESIAN_POINT('Ctrl Pts',(-83.0561836960466,4.32256531714715,-11.2912880660449));
#34481=CARTESIAN_POINT('Ctrl Pts',(-83.0959686642429,2.37560562037672,-11.6870432880836));
#34482=CARTESIAN_POINT('Ctrl Pts',(-83.1357536324391,0.4286459236063,-12.0827985101224));
#34483=CARTESIAN_POINT('Ctrl Pts',(-83.1755386006354,-1.61935666142352,
-11.9814623945722));
#34484=CARTESIAN_POINT('Ctrl Pts',(-83.2153235688317,-3.51773743235987,
-11.395437955618));
#34485=CARTESIAN_POINT('Ctrl Pts',(-83.255108537028,-5.41611820329623,-10.8094135166638));
#34486=CARTESIAN_POINT('Ctrl Pts',(-83.2948935052242,-7.1648771601391,-9.73870075430558));
#34487=CARTESIAN_POINT('Ctrl Pts',(-83.3346784734205,-8.54997538283724,
-8.31434927639566));
#34488=CARTESIAN_POINT('Ctrl Pts',(-83.3744634416168,-9.93507360553538,
-6.88999779848573));
#34489=CARTESIAN_POINT('Ctrl Pts',(-83.414248409813,-10.9565110940888,-5.1120076050241));
#34490=CARTESIAN_POINT('Ctrl Pts',(-83.4540333780092,-11.4892692818526,
-3.19799534641771));
#34491=CARTESIAN_POINT('Ctrl Pts',(-83.4756366362888,-11.7785572529796,
-2.15868570140124));
#34492=CARTESIAN_POINT('Ctrl Pts',(-83.4972398945685,-11.9237583468368,
-1.07927001020106));
#34493=CARTESIAN_POINT('Ctrl Pts',(-83.5188431528481,-11.9240088006309,
7.96196756353007E-5));
#34494=CARTESIAN_POINT('Ctrl Pts',(-83.7311568471519,-11.9239866250219,
-4.23754525262852E-5));
#34495=CARTESIAN_POINT('Ctrl Pts',(-83.7121679170328,-11.9241035316002,
-0.948779049150204));
#34496=CARTESIAN_POINT('Ctrl Pts',(-83.6931789869137,-11.8122490199285,
-1.89748862014936));
#34497=CARTESIAN_POINT('Ctrl Pts',(-83.6741900567946,-11.588113260095,-2.8188850364372));
#34498=CARTESIAN_POINT('Ctrl Pts',(-83.6344050885983,-11.1185115489563,
-4.74936384110115));
#34499=CARTESIAN_POINT('Ctrl Pts',(-83.5946201204021,-10.1560263492076,
-6.55994548395522));
#34500=CARTESIAN_POINT('Ctrl Pts',(-83.5548351522058,-8.81846078752594,
-8.02902429411543));
#34501=CARTESIAN_POINT('Ctrl Pts',(-83.5150501840096,-7.48089522584431,
-9.49810310427565));
#34502=CARTESIAN_POINT('Ctrl Pts',(-83.4752652158133,-5.76824930222981,
-10.625679081742));
#34503=CARTESIAN_POINT('Ctrl Pts',(-83.435480247617,-3.89014187032842,-11.2737428570226));
#34504=CARTESIAN_POINT('Ctrl Pts',(-83.3956952794208,-2.01203443842704,
-11.9218066323032));
#34505=CARTESIAN_POINT('Ctrl Pts',(-83.3559103112245,0.0315345017612198,
-12.090358205398));
#34506=CARTESIAN_POINT('Ctrl Pts',(-83.3161253430283,1.99044285894123,-11.7587677501927));
#34507=CARTESIAN_POINT('Ctrl Pts',(-83.276340374832,3.94935121612124,-11.4271772949875));
#34508=CARTESIAN_POINT('Ctrl Pts',(-83.2365554066357,5.82359899029299,-10.5954448114821));
#34509=CARTESIAN_POINT('Ctrl Pts',(-83.1967704384394,7.38378811207008,-9.36536998144095));
#34510=CARTESIAN_POINT('Ctrl Pts',(-83.1569854702432,8.9439772338472,-8.13529515139976));
#34511=CARTESIAN_POINT('Ctrl Pts',(-83.117200502047,10.1901077032297,-6.50687797482273));
#34512=CARTESIAN_POINT('Ctrl Pts',(-83.0774155338507,10.9696597020526,-4.67942814989959));
#34513=CARTESIAN_POINT('Ctrl Pts',(-83.0376305656544,11.7492117008756,-2.85197832497647));
#34514=CARTESIAN_POINT('Ctrl Pts',(-82.9978455974581,12.0621852291391,-0.825495851707222));
#34515=CARTESIAN_POINT('Ctrl Pts',(-82.9580606292619,11.8702739778685,1.15198847272976));
#34516=CARTESIAN_POINT('Ctrl Pts',(-82.9182756610656,11.6783627265978,3.12947279716674));
#34517=CARTESIAN_POINT('Ctrl Pts',(-82.8784906928694,10.981566695793,5.05795897277145));
#34518=CARTESIAN_POINT('Ctrl Pts',(-82.8387057246731,9.86517004487055,6.70141043418577));
#34519=CARTESIAN_POINT('Ctrl Pts',(-82.7989207564769,8.74877339394805,8.34486189560009));
#34520=CARTESIAN_POINT('Ctrl Pts',(-82.7591357882806,7.21277612290786,9.70327864282402));
#34521=CARTESIAN_POINT('Ctrl Pts',(-82.7193508200843,5.44517624072831,10.6103976096621));
#34522=CARTESIAN_POINT('Ctrl Pts',(-82.679565851888,3.67757635854875,11.5175165765002));
#34523=CARTESIAN_POINT('Ctrl Pts',(-82.6397808836917,1.67837386522983,11.9733377629524));
#34524=CARTESIAN_POINT('Ctrl Pts',(-82.5999959154955,-0.307739412094615,
11.9220710541212));
#34525=CARTESIAN_POINT('Ctrl Pts',(-82.5602109472993,-2.29385268941909,
11.87080434529));
#34526=CARTESIAN_POINT('Ctrl Pts',(-82.5204259791031,-4.26687675074909,
11.3124497411754));
#34527=CARTESIAN_POINT('Ctrl Pts',(-82.4806410109068,-5.98532373643242,
10.3153469066002));
#34528=CARTESIAN_POINT('Ctrl Pts',(-82.4408560427106,-7.70377072211571,
9.31824407202492));
#34529=CARTESIAN_POINT('Ctrl Pts',(-82.4010710745143,-9.16764063215234,
7.88239300698909));
#34530=CARTESIAN_POINT('Ctrl Pts',(-82.361286106318,-10.1977636774582,6.18353433504965));
#34531=CARTESIAN_POINT('Ctrl Pts',(-82.3215011381217,-11.227886722764,4.48467566311021));
#34532=CARTESIAN_POINT('Ctrl Pts',(-82.2817161699255,-11.8242629033391,
2.52280938426718));
#34533=CARTESIAN_POINT('Ctrl Pts',(-82.2419312017292,-11.9138985183695,
0.538057603617393));
#34534=CARTESIAN_POINT('Ctrl Pts',(-82.2383397502035,-11.9219900660308,
0.358890945100783));
#34535=CARTESIAN_POINT('Ctrl Pts',(-82.2347482986777,-11.9259522069787,
0.179537793630527));
#34536=CARTESIAN_POINT('Ctrl Pts',(-82.2311568471519,-11.9258224962353,
0.000178908662697473));
#34537=CARTESIAN_POINT('Origin',(-92.7728704041008,0.,0.));
#34538=CARTESIAN_POINT('',(-81.5228704041008,-11.0668932874501,4.91862629439992E-5));
#34539=CARTESIAN_POINT('',(-81.425,-11.06595,-4.66420812603649E-14));
#34540=CARTESIAN_POINT('',(-92.7728704041008,-11.06595,-4.66420812603649E-14));
#34541=CARTESIAN_POINT('',(-81.425,-10.149321152349,-4.41097929944913));
#34542=CARTESIAN_POINT('Ctrl Pts',(-81.5228704041008,-11.0668939277106,
4.92196483355134E-5));
#34543=CARTESIAN_POINT('Ctrl Pts',(-81.4902469360672,-11.0665321546601,
-1.51174383270627));
#34544=CARTESIAN_POINT('Ctrl Pts',(-81.4576234680336,-10.7506077524621,
-3.0236872243398));
#34545=CARTESIAN_POINT('Ctrl Pts',(-81.425,-10.149321152349,-4.41097929944913));
#34546=CARTESIAN_POINT('Origin',(-81.425,0.,0.));
#34547=CARTESIAN_POINT('Origin',(-92.7728704041008,0.,0.));
#34548=CARTESIAN_POINT('',(-83.0228704041008,-11.0650302043893,7.38840550997362E-5));
#34549=CARTESIAN_POINT('',(-82.7271295958992,-11.0667132454688,0.000166020487631646));
#34550=CARTESIAN_POINT('',(-92.7728704041008,-11.06595,-4.66420812603649E-14));
#34551=CARTESIAN_POINT('Ctrl Pts',(-83.0228704041008,-11.0650302043893,
7.38840550998376E-5));
#34552=CARTESIAN_POINT('Ctrl Pts',(-83.0012671458212,-11.0647977927194,
-1.00152184229597));
#34553=CARTESIAN_POINT('Ctrl Pts',(-82.9398789193453,-10.6819148380356,
-3.84784936091178));
#34554=CARTESIAN_POINT('Ctrl Pts',(-82.8387057246731,-8.27151795293221,
-8.04356576264067));
#34555=CARTESIAN_POINT('Ctrl Pts',(-82.7193508200843,-3.40317098979375,
-11.0243088802804));
#34556=CARTESIAN_POINT('Ctrl Pts',(-82.5999959154955,2.29823635758004,-11.306417153959));
#34557=CARTESIAN_POINT('Ctrl Pts',(-82.4806410109068,7.43705978076056,-8.82083340892465));
#34558=CARTESIAN_POINT('Ctrl Pts',(-82.361286106318,10.7553688582105,-4.17600247780928));
#34559=CARTESIAN_POINT('Ctrl Pts',(-82.2419312017292,11.4408774690408,1.49107004187632));
#34560=CARTESIAN_POINT('Ctrl Pts',(-82.1225762971404,9.32577815964549,6.79314407704868));
#34561=CARTESIAN_POINT('Ctrl Pts',(-82.0032213925517,4.92782947223121,10.4323283560957));
#34562=CARTESIAN_POINT('Ctrl Pts',(-81.8838664879629,-0.676406317082347,
11.5177874273519));
#34563=CARTESIAN_POINT('Ctrl Pts',(-81.7645115833741,-6.1150519099602,9.78381527403391));
#34564=CARTESIAN_POINT('Ctrl Pts',(-81.6451566787853,-10.0568242125366,
5.65486392012898));
#34565=CARTESIAN_POINT('Ctrl Pts',(-81.5646096190276,-11.0555472977052,
1.93426637659237));
#34566=CARTESIAN_POINT('Ctrl Pts',(-81.5238475274661,-11.0669047633735,
0.0453297616602893));
#34567=CARTESIAN_POINT('Ctrl Pts',(-81.5228704041008,-11.0668939277106,
4.92196483355134E-5));
#34568=CARTESIAN_POINT('',(-81.425,-7.47762833958605,8.15722525234652));
#34569=CARTESIAN_POINT('Origin',(-81.425,0.,0.));
#34570=CARTESIAN_POINT('Ctrl Pts',(-82.7271295958992,-11.0667132454688,
0.000166020487631455));
#34571=CARTESIAN_POINT('Ctrl Pts',(-82.6909360792287,-11.0655002280488,
-1.67714648383287));
#34572=CARTESIAN_POINT('Ctrl Pts',(-82.614957594362,-10.2534263510633,-5.19934407837023));
#34573=CARTESIAN_POINT('Ctrl Pts',(-82.499194141299,-6.66636917491129,-9.416820017226));
#34574=CARTESIAN_POINT('Ctrl Pts',(-82.3798392367102,-1.33616352515641,
-11.4600008190507));
#34575=CARTESIAN_POINT('Ctrl Pts',(-82.2604843321214,4.32110767959995,-10.6978936382306));
#34576=CARTESIAN_POINT('Ctrl Pts',(-82.1411294275327,8.92064463412699,-7.31705529020618));
#34577=CARTESIAN_POINT('Ctrl Pts',(-82.0217745229439,11.3364445890174,-2.14507737917849));
#34578=CARTESIAN_POINT('Ctrl Pts',(-81.9024196183551,10.9773205983354,3.5519900017792));
#34579=CARTESIAN_POINT('Ctrl Pts',(-81.7830647137664,7.93081818705442,8.37957343457652));
#34580=CARTESIAN_POINT('Ctrl Pts',(-81.6637098091775,2.94344912458979,11.155910191377));
#34581=CARTESIAN_POINT('Ctrl Pts',(-81.5443549045888,-2.76549453716151,
11.2014042094999));
#34582=CARTESIAN_POINT('Ctrl Pts',(-81.4647849681962,-6.11821953149998,
9.40337863342461));
#34583=CARTESIAN_POINT('Ctrl Pts',(-81.425,-7.47762833958605,8.15722525234652));
#34584=CARTESIAN_POINT('Origin',(-92.7728704041008,0.,0.));
#34585=CARTESIAN_POINT('',(-84.5228704041007,-11.0666243849915,-0.000196364959975874));
#34586=CARTESIAN_POINT('',(-84.2271295958992,-11.0650096262609,-3.93228210321395E-5));
#34587=CARTESIAN_POINT('',(-92.7728704041008,-11.06595,-4.66420812603649E-14));
#34588=CARTESIAN_POINT('Ctrl Pts',(-84.5228704041008,-11.0666243849915,
-0.000196364959975971));
#34589=CARTESIAN_POINT('Ctrl Pts',(-84.5184717323725,-11.066792356144,-0.204048309631058));
#34590=CARTESIAN_POINT('Ctrl Pts',(-84.474288092448,-11.0113828159013,-2.25160265711946));
#34591=CARTESIAN_POINT('Ctrl Pts',(-84.3903194843273,-9.80445239033203,
-6.08191356265241));
#34592=CARTESIAN_POINT('Ctrl Pts',(-84.2709645797384,-5.68886699611132,
-10.0376168266402));
#34593=CARTESIAN_POINT('Ctrl Pts',(-84.1516096751498,-0.180706798974452,
-11.5362170710623));
#34594=CARTESIAN_POINT('Ctrl Pts',(-84.0322547705609,5.37168852179416,-10.2108727189529));
#34595=CARTESIAN_POINT('Ctrl Pts',(-83.9128998659722,9.60915099398264,-6.38601412721019));
#34596=CARTESIAN_POINT('Ctrl Pts',(-83.7935449613833,11.4943943756167,-0.99792644773947));
#34597=CARTESIAN_POINT('Ctrl Pts',(-83.6741900567946,10.5659309167634,4.63444312957206));
#34598=CARTESIAN_POINT('Ctrl Pts',(-83.5548351522057,7.0510387058728,9.13234977562325));
#34599=CARTESIAN_POINT('Ctrl Pts',(-83.4354802476171,1.81012638584784,11.3947532543155));
#34600=CARTESIAN_POINT('Ctrl Pts',(-83.3161253430282,-3.87388583478548,
10.8678409906937));
#34601=CARTESIAN_POINT('Ctrl Pts',(-83.1967704384395,-8.6096115480947,7.68059556507888));
#34602=CARTESIAN_POINT('Ctrl Pts',(-83.0990187921303,-10.7620932754816,
3.53041677683679));
#34603=CARTESIAN_POINT('Ctrl Pts',(-83.0410521140174,-11.0652258064372,
0.843035751868332));
#34604=CARTESIAN_POINT('Ctrl Pts',(-83.0228704041008,-11.0650302043893,
7.38840550998376E-5));
#34605=CARTESIAN_POINT('Ctrl Pts',(-84.2271295958992,-11.0650096262609,
-3.93228210321395E-5));
#34606=CARTESIAN_POINT('Ctrl Pts',(-84.2081406657801,-11.065118111154,-0.880431154628511));
#34607=CARTESIAN_POINT('Ctrl Pts',(-84.1493667674648,-10.743849849773,-3.60531251949298));
#34608=CARTESIAN_POINT('Ctrl Pts',(-84.0508079009531,-8.53125926061665,
-7.76753330473083));
#34609=CARTESIAN_POINT('Ctrl Pts',(-83.9314529963644,-3.76344689371811,
-10.9065771758865));
#34610=CARTESIAN_POINT('Ctrl Pts',(-83.8120980917756,1.92561768833889,-11.3758056740724));
#34611=CARTESIAN_POINT('Ctrl Pts',(-83.6927431871867,7.1433113126398,-9.06035659838774));
#34612=CARTESIAN_POINT('Ctrl Pts',(-83.573388282598,10.6123974680266,-4.52702752791171));
#34613=CARTESIAN_POINT('Ctrl Pts',(-83.4540333780092,11.4836803397467,1.11447026455969));
#34614=CARTESIAN_POINT('Ctrl Pts',(-83.3346784734204,9.54387907255568,6.48315745825352));
#34615=CARTESIAN_POINT('Ctrl Pts',(-83.2153235688317,5.26783655646332,10.2648358994969));
#34616=CARTESIAN_POINT('Ctrl Pts',(-83.0959686642429,-0.297716860125996,
11.5337904801815));
#34617=CARTESIAN_POINT('Ctrl Pts',(-82.9766137596541,-5.79039248565415,
9.9793944722816));
#34618=CARTESIAN_POINT('Ctrl Pts',(-82.8572588550654,-9.86564059407429,
5.98214765639898));
#34619=CARTESIAN_POINT('Ctrl Pts',(-82.774097467147,-11.0224273794537,2.1767290968266));
#34620=CARTESIAN_POINT('Ctrl Pts',(-82.730721047425,-11.0668336121439,0.166604297477993));
#34621=CARTESIAN_POINT('Ctrl Pts',(-82.7271295958992,-11.0667132454688,
0.000166020487631455));
#34622=CARTESIAN_POINT('Origin',(-92.7728704041008,0.,0.));
#34623=CARTESIAN_POINT('',(-86.0228704041009,-11.065460751515,0.000255221764428716));
#34624=CARTESIAN_POINT('',(-85.7271295958992,-11.0668617871986,-8.70765389315853E-5));
#34625=CARTESIAN_POINT('',(-92.7728704041008,-11.06595,-4.66420812603649E-14));
#34626=CARTESIAN_POINT('Ctrl Pts',(-86.0228704041009,-11.065460751515,0.00025522176442902));
#34627=CARTESIAN_POINT('Ctrl Pts',(-85.9958913507277,-11.064405544315,-1.25044009334015));
#34628=CARTESIAN_POINT('Ctrl Pts',(-85.9291273291583,-10.5406416224597,
-4.34634890493393));
#34629=CARTESIAN_POINT('Ctrl Pts',(-85.8225783393926,-7.7096875531033,-8.58357018328625));
#34630=CARTESIAN_POINT('Ctrl Pts',(-85.7032234348039,-2.65123622795373,
-11.2288871096588));
#34631=CARTESIAN_POINT('Ctrl Pts',(-85.583868530215,3.05620983905482,-11.1254905814324));
#34632=CARTESIAN_POINT('Ctrl Pts',(-85.4645136256263,8.01552788387837,-8.29869098115147));
#34633=CARTESIAN_POINT('Ctrl Pts',(-85.3451587210375,11.0127290131994,-3.44045911757623));
#34634=CARTESIAN_POINT('Ctrl Pts',(-85.2258038164487,11.3141299162988,2.25996094988123));
#34635=CARTESIAN_POINT('Ctrl Pts',(-85.10644891186,8.84595082235115,7.40716634796478));
#34636=CARTESIAN_POINT('Ctrl Pts',(-84.9870940072712,4.21237601227739,10.7411753355518));
#34637=CARTESIAN_POINT('Ctrl Pts',(-84.8677391026824,-1.45234413817624,
11.4458575808972));
#34638=CARTESIAN_POINT('Ctrl Pts',(-84.7483841980936,-6.7615457199306,9.34871428246502));
#34639=CARTESIAN_POINT('Ctrl Pts',(-84.6334279652331,-10.2809268459538,
5.1247300936646));
#34640=CARTESIAN_POINT('Ctrl Pts',(-84.5582567005688,-11.0652730959279,
1.63974537094761));
#34641=CARTESIAN_POINT('Ctrl Pts',(-84.5228704041008,-11.0666243849915,
-0.000196364959975971));
#34642=CARTESIAN_POINT('Ctrl Pts',(-85.7271295958992,-11.0668617871986,
-8.70765389308394E-5));
#34643=CARTESIAN_POINT('Ctrl Pts',(-85.7253452523315,-11.0668963362517,
-0.0827755069023009));
#34644=CARTESIAN_POINT('Ctrl Pts',(-85.6837759405676,-11.045758910777,-2.00912511781817));
#34645=CARTESIAN_POINT('Ctrl Pts',(-85.6024216606073,-9.99893271614051,
-5.75658776984223));
#34646=CARTESIAN_POINT('Ctrl Pts',(-85.4830667560185,-6.01549992917226,
-9.84533995430987));
#34647=CARTESIAN_POINT('Ctrl Pts',(-85.3637118514298,-0.559536032933944,
-11.5240564751155));
#34648=CARTESIAN_POINT('Ctrl Pts',(-85.2443569468409,5.03339639874698,-10.3818051853656));
#34649=CARTESIAN_POINT('Ctrl Pts',(-85.1250020422522,9.39420633525482,-6.69819718614323));
#34650=CARTESIAN_POINT('Ctrl Pts',(-85.0056471376634,11.4554133728453,-1.37494097002217));
#34651=CARTESIAN_POINT('Ctrl Pts',(-84.8862922330746,10.7124557092996,4.28488633339115));
#34652=CARTESIAN_POINT('Ctrl Pts',(-84.7669373284858,7.34720156593731,8.89581853250784));
#34653=CARTESIAN_POINT('Ctrl Pts',(-84.647582423897,2.18342975997975,11.3291479245805));
#34654=CARTESIAN_POINT('Ctrl Pts',(-84.5282275193083,-3.5148226850366,10.9892210691436));
#34655=CARTESIAN_POINT('Ctrl Pts',(-84.4088726147195,-8.35268350706726,
7.95924848492489));
#34656=CARTESIAN_POINT('Ctrl Pts',(-84.3085066402497,-10.7015054577232,
3.77296701935926));
#34657=CARTESIAN_POINT('Ctrl Pts',(-84.2479256339763,-11.0648908172521,
0.964136222734465));
#34658=CARTESIAN_POINT('Ctrl Pts',(-84.2271295958992,-11.0650096262609,
-3.93228210321395E-5));
#34659=CARTESIAN_POINT('Origin',(-92.7728704041008,0.,0.));
#34660=CARTESIAN_POINT('',(-87.5228704041008,-11.0658700602947,-0.000290735752023665));
#34661=CARTESIAN_POINT('',(-87.2271295958992,-11.065192145401,0.000181283075004757));
#34662=CARTESIAN_POINT('',(-92.7728704041008,-11.06595,-4.66420812603649E-14));
#34663=CARTESIAN_POINT('Ctrl Pts',(-87.5228704041008,-11.0658700602947,
-0.000290735752023694));
#34664=CARTESIAN_POINT('Ctrl Pts',(-87.513095937279,-11.0663323771202,-0.453367480613647));
#34665=CARTESIAN_POINT('Ctrl Pts',(-87.4635365022611,-10.9279235443852,
-2.75031985271847));
#34666=CARTESIAN_POINT('Ctrl Pts',(-87.3741920990468,-9.37154264007224,
-6.72986982053519));
#34667=CARTESIAN_POINT('Ctrl Pts',(-87.2548371944581,-4.99832326681662,
-10.398736643432));
#34668=CARTESIAN_POINT('Ctrl Pts',(-87.1354822898692,0.598433067870375,
-11.5221021137892));
#34669=CARTESIAN_POINT('Ctrl Pts',(-87.0161273852805,6.04869928207646,-9.82497818079478));
#34670=CARTESIAN_POINT('Ctrl Pts',(-86.8967724806917,10.0183075346351,-5.72280293206974));
#34671=CARTESIAN_POINT('Ctrl Pts',(-86.7774175761028,11.5355394792043,-0.219745720288259));
#34672=CARTESIAN_POINT('Ctrl Pts',(-86.6580626715142,10.2289926946021,5.33710293246003));
#34673=CARTESIAN_POINT('Ctrl Pts',(-86.5387077669253,6.41849609092341,9.58748492508142));
#34674=CARTESIAN_POINT('Ctrl Pts',(-86.4193528623365,1.03681915645036,11.4909514529782));
#34675=CARTESIAN_POINT('Ctrl Pts',(-86.2999979577478,-4.59866020185083,
10.5815539315257));
#34676=CARTESIAN_POINT('Ctrl Pts',(-86.1806430531589,-9.10843591325322,
7.08190330857717));
#34677=CARTESIAN_POINT('Ctrl Pts',(-86.0882672019434,-10.8731611950013,
3.03159876678569));
#34678=CARTESIAN_POINT('Ctrl Pts',(-86.035676318924,-11.0659616176254,0.593911991459538));
#34679=CARTESIAN_POINT('Ctrl Pts',(-86.0228704041009,-11.065460751515,0.00025522176442902));
#34680=CARTESIAN_POINT('Ctrl Pts',(-87.2271295958992,-11.065192145401,0.000181283075005034));
#34681=CARTESIAN_POINT('Ctrl Pts',(-87.2027648706866,-11.0645372281205,
-1.12939750798797));
#34682=CARTESIAN_POINT('Ctrl Pts',(-87.1386151772778,-10.6117081325261,
-4.10396985076007));
#34683=CARTESIAN_POINT('Ctrl Pts',(-87.0346805156727,-7.98746940186916,
-8.32570061724489));
#34684=CARTESIAN_POINT('Ctrl Pts',(-86.9153256110839,-3.01863758058317,
-11.1357435930835));
#34685=CARTESIAN_POINT('Ctrl Pts',(-86.7959707064951,2.68912496921423,-11.2198736674593));
#34686=CARTESIAN_POINT('Ctrl Pts',(-86.6766158019064,7.73861801182051,-8.55749668308028));
#34687=CARTESIAN_POINT('Ctrl Pts',(-86.5572608973175,10.8937787629573,-3.80033452179447));
#34688=CARTESIAN_POINT('Ctrl Pts',(-86.4379059927288,11.3822570579663,1.88710955701514));
#34689=CARTESIAN_POINT('Ctrl Pts',(-86.31855108814,9.08447854823605,7.11260906562713));
#34690=CARTESIAN_POINT('Ctrl Pts',(-86.1991961835512,4.56291524401145,10.5970166881896));
#34691=CARTESIAN_POINT('Ctrl Pts',(-86.0798412789624,-1.07560171741225,
11.4873860890675));
#34692=CARTESIAN_POINT('Ctrl Pts',(-85.9604863743737,-6.45082269201481,
9.56576420418091));
#34693=CARTESIAN_POINT('Ctrl Pts',(-85.8429158133526,-10.1901984085959,
5.36627856497651));
#34694=CARTESIAN_POINT('Ctrl Pts',(-85.7651302205278,-11.0661260064756,
1.7609033852933));
#34695=CARTESIAN_POINT('Ctrl Pts',(-85.7271295958992,-11.0668617871986,
-8.70765389308394E-5));
#34696=CARTESIAN_POINT('Origin',(-92.7728704041008,0.,0.));
#34697=CARTESIAN_POINT('',(-89.0228704041008,-11.0662155972561,0.000275354078309783));
#34698=CARTESIAN_POINT('',(-88.7271295958992,-11.0662550916496,-0.000269981886922288));
#34699=CARTESIAN_POINT('',(-92.7728704041008,-11.06595,-4.66420812603649E-14));
#34700=CARTESIAN_POINT('Ctrl Pts',(-89.0228704041008,-11.0662155972561,
0.000275354078309552));
#34701=CARTESIAN_POINT('Ctrl Pts',(-88.9905155556342,-11.0646746332228,
-1.49933692734806));
#34702=CARTESIAN_POINT('Ctrl Pts',(-88.9183757389713,-10.3801459586505,
-4.84430558557994));
#34703=CARTESIAN_POINT('Ctrl Pts',(-88.8064509541122,-7.11268667591289,
-9.08441704154723));
#34704=CARTESIAN_POINT('Ctrl Pts',(-88.6870960495234,-1.88720699773628,
-11.3822412941864));
#34705=CARTESIAN_POINT('Ctrl Pts',(-88.5677411449346,3.80024137539898,-10.8938111540241));
#34706=CARTESIAN_POINT('Ctrl Pts',(-88.4483862403457,8.55743050117986,-7.73869132528777));
#34707=CARTESIAN_POINT('Ctrl Pts',(-88.3290313357571,11.2198507137954,-2.6892209233878));
#34708=CARTESIAN_POINT('Ctrl Pts',(-88.2096764311682,11.1357694560897,3.01854231284303));
#34709=CARTESIAN_POINT('Ctrl Pts',(-88.0903215265796,8.32576898055664,7.9873982188198));
#34710=CARTESIAN_POINT('Ctrl Pts',(-87.9709666219907,3.47770782525073,11.0010230180077));
#34711=CARTESIAN_POINT('Ctrl Pts',(-87.8516117174019,-2.22165962238982,
11.3217131134804));
#34712=CARTESIAN_POINT('Ctrl Pts',(-87.7322568128132,-7.37718816438983,
8.87096691632776));
#34713=CARTESIAN_POINT('Ctrl Pts',(-87.6226763750461,-10.4525402687832,
4.62723777833816));
#34714=CARTESIAN_POINT('Ctrl Pts',(-87.5528809054753,-11.0644506110316,
1.39078874944263));
#34715=CARTESIAN_POINT('Ctrl Pts',(-87.5228704041008,-11.0658700602947,
-0.000290735752023694));
#34716=CARTESIAN_POINT('Ctrl Pts',(-88.7271295958992,-11.0662550916496,
-0.000269981886922149));
#34717=CARTESIAN_POINT('Ctrl Pts',(-88.719969457238,-11.0665935271679,-0.332131280800377));
#34718=CARTESIAN_POINT('Ctrl Pts',(-88.6730243503806,-10.9706735787383,
-2.50776908882701));
#34719=CARTESIAN_POINT('Ctrl Pts',(-88.5862942753268,-9.58753979769892,
-6.41841405704041));
#34720=CARTESIAN_POINT('Ctrl Pts',(-88.4669393707381,-5.33719041442222,
-10.2289469935215));
#34721=CARTESIAN_POINT('Ctrl Pts',(-88.3475844661493,0.219647037160976,
-11.5355413152965));
#34722=CARTESIAN_POINT('Ctrl Pts',(-88.2282295615605,5.72271720750059,-10.0183564501475));
#34723=CARTESIAN_POINT('Ctrl Pts',(-88.1088746569716,9.82492639772949,-6.0487833070047));
#34724=CARTESIAN_POINT('Ctrl Pts',(-87.989519752383,11.5220969489527,-0.598531631862895));
#34725=CARTESIAN_POINT('Ctrl Pts',(-87.8701648477941,10.3987793606657,4.99823429024215));
#34726=CARTESIAN_POINT('Ctrl Pts',(-87.7508099432054,6.72994996350157,9.37148503193342));
#34727=CARTESIAN_POINT('Ctrl Pts',(-87.6314550386166,1.41369960344878,11.4506948105535));
#34728=CARTESIAN_POINT('Ctrl Pts',(-87.5121001340278,-4.24860954964163,
10.7268949425594));
#34729=CARTESIAN_POINT('Ctrl Pts',(-87.3927452294391,-8.87090377354262,
7.37726402227169));
#34730=CARTESIAN_POINT('Ctrl Pts',(-87.2977550500628,-10.8213976376337,
3.27418514836392));
#34731=CARTESIAN_POINT('Ctrl Pts',(-87.2425498388829,-11.0656066373975,
0.715082816969709));
#34732=CARTESIAN_POINT('Ctrl Pts',(-87.2271295958992,-11.065192145401,0.000181283075005034));
#34733=CARTESIAN_POINT('Origin',(-90.25,0.,0.));
#34734=CARTESIAN_POINT('',(-90.,15.5,-1.8982025386784E-15));
#34735=CARTESIAN_POINT('Origin',(-90.,0.,0.));
#34736=CARTESIAN_POINT('',(-90.5,16.,1.95943487863577E-15));
#34737=CARTESIAN_POINT('',(-90.25,15.75,1.92881870865708E-15));
#34738=CARTESIAN_POINT('',(-90.5,-16.,-1.95943487863577E-15));
#34739=CARTESIAN_POINT('Origin',(-90.5,0.,0.));
#34740=CARTESIAN_POINT('Origin',(-90.5,0.,0.));
#34741=CARTESIAN_POINT('Origin',(-91.5,0.,0.));
#34742=CARTESIAN_POINT('',(-92.5,-16.,-1.95943487863577E-15));
#34743=CARTESIAN_POINT('',(-91.5,-16.,-1.95943487863577E-15));
#34744=CARTESIAN_POINT('',(-92.5,16.,-1.95943487863577E-15));
#34745=CARTESIAN_POINT('Origin',(-92.5,0.,0.));
#34746=CARTESIAN_POINT('Origin',(-92.5,0.,0.));
#34747=CARTESIAN_POINT('Origin',(-90.,12.,0.));
#34748=CARTESIAN_POINT('',(-90.,6.42428395783992,-9.0102067141404));
#34749=CARTESIAN_POINT('Ctrl Pts',(-90.,5.13009691060825,10.7656670051306));
#34750=CARTESIAN_POINT('Ctrl Pts',(-90.,5.38142570207304,10.63534500805));
#34751=CARTESIAN_POINT('Ctrl Pts',(-90.,5.62776587470053,10.496194090036));
#34752=CARTESIAN_POINT('Ctrl Pts',(-90.,5.86860373811413,10.3483657837986));
#34753=CARTESIAN_POINT('Ctrl Pts',(-90.,5.89059422220645,10.334867839702));
#34754=CARTESIAN_POINT('Ctrl Pts',(-90.,5.91253881540746,10.321297518862));
#34755=CARTESIAN_POINT('Ctrl Pts',(-90.,5.93443711591287,10.3076549177303));
#34756=CARTESIAN_POINT('Ctrl Pts',(-90.,6.17470730136342,10.1579670319908));
#34757=CARTESIAN_POINT('Ctrl Pts',(-90.,6.4094071003827,9.99958102185828));
#34758=CARTESIAN_POINT('Ctrl Pts',(-90.,6.63816875447367,9.83291388620034));
#34759=CARTESIAN_POINT('Ctrl Pts',(-90.,6.86708098763998,9.66613704429256));
#34760=CARTESIAN_POINT('Ctrl Pts',(-90.,7.09004769008821,9.49106769853988));
#34761=CARTESIAN_POINT('Ctrl Pts',(-90.,7.30666447004526,9.30808587696727));
#34762=CARTESIAN_POINT('Ctrl Pts',(-90.,7.37724818810362,9.24846197661085));
#34763=CARTESIAN_POINT('Ctrl Pts',(-90.,7.44715738756786,9.18799769541298));
#34764=CARTESIAN_POINT('Ctrl Pts',(-90.,7.51637713519723,9.12670544422352));
#34765=CARTESIAN_POINT('Ctrl Pts',(-90.,7.5638011805984,9.08471270945205));
#34766=CARTESIAN_POINT('Ctrl Pts',(-90.,7.61090159178926,9.04233132367685));
#34767=CARTESIAN_POINT('Ctrl Pts',(-90.,7.65767343085564,8.99956519068863));
#34768=CARTESIAN_POINT('Ctrl Pts',(-90.,7.68556498060487,8.97406237212017));
#34769=CARTESIAN_POINT('Ctrl Pts',(-90.,7.71333301047639,8.94842881556734));
#34770=CARTESIAN_POINT('Ctrl Pts',(-90.,7.74097359853661,8.922668405457));
#34771=CARTESIAN_POINT('Ctrl Pts',(-90.,7.94709453709131,8.73056829897841));
#34772=CARTESIAN_POINT('Ctrl Pts',(-90.,8.14618697943012,8.53136626644155));
#34773=CARTESIAN_POINT('Ctrl Pts',(-90.,8.33789206599765,8.32547463222084));
#34774=CARTESIAN_POINT('Ctrl Pts',(-90.,8.52924341455732,8.1199629133056));
#34775=CARTESIAN_POINT('Ctrl Pts',(-90.,8.71323504729152,7.90778577042483));
#34776=CARTESIAN_POINT('Ctrl Pts',(-90.,8.88947131067135,7.68931924303648));
#34777=CARTESIAN_POINT('Ctrl Pts',(-90.,9.06438024748662,7.47249810020014));
#34778=CARTESIAN_POINT('Ctrl Pts',(-90.,9.2316505465745,7.24948146658954));
#34779=CARTESIAN_POINT('Ctrl Pts',(-90.,9.39085163563897,7.02061071827486));
#34780=CARTESIAN_POINT('Ctrl Pts',(-90.,9.4429730085429,6.94567996440997));
#34781=CARTESIAN_POINT('Ctrl Pts',(-90.,9.4942290980679,6.87012154957565));
#34782=CARTESIAN_POINT('Ctrl Pts',(-90.,9.54460366504352,6.79394696955633));
#34783=CARTESIAN_POINT('Ctrl Pts',(-90.,9.56885339937438,6.75727740713355));
#34784=CARTESIAN_POINT('Ctrl Pts',(-90.,9.59289884560302,6.72046505461935));
#34785=CARTESIAN_POINT('Ctrl Pts',(-90.,9.61673814334246,6.6835111777183));
#34786=CARTESIAN_POINT('Ctrl Pts',(-90.,9.63482522819697,6.65547394631501));
#34787=CARTESIAN_POINT('Ctrl Pts',(-90.,9.65279406781826,6.62735450526691));
#34788=CARTESIAN_POINT('Ctrl Pts',(-90.,9.67063513222111,6.59916738127204));
#34789=CARTESIAN_POINT('Ctrl Pts',(-90.,9.77582411073673,6.43297915878919));
#34790=CARTESIAN_POINT('Ctrl Pts',(-90.,9.87664553414384,6.26432609926212));
#34791=CARTESIAN_POINT('Ctrl Pts',(-90.,9.97297960718523,6.09334570164801));
#34792=CARTESIAN_POINT('Ctrl Pts',(-90.,10.1090715536707,5.85180027138097));
#34793=CARTESIAN_POINT('Ctrl Pts',(-90.,10.2362100229841,5.60561105936211));
#34794=CARTESIAN_POINT('Ctrl Pts',(-90.,10.3543191903964,5.35532203303746));
#34795=CARTESIAN_POINT('Ctrl Pts',(-90.,10.4732217365238,5.10335173174952));
#34796=CARTESIAN_POINT('Ctrl Pts',(-90.,10.5829734569656,4.84722574878759));
#34797=CARTESIAN_POINT('Ctrl Pts',(-90.,10.6834490166989,4.58747640854734));
#34798=CARTESIAN_POINT('Ctrl Pts',(-90.,10.7839018241246,4.32778588755518));
#34799=CARTESIAN_POINT('Ctrl Pts',(-90.,10.8750828153631,4.06447302517473));
#34800=CARTESIAN_POINT('Ctrl Pts',(-90.,10.9568165288933,3.79805645882746));
#34801=CARTESIAN_POINT('Ctrl Pts',(-90.,11.0372022543992,3.53603375060076));
#34802=CARTESIAN_POINT('Ctrl Pts',(-90.,11.1084497580427,3.27100827338904));
#34803=CARTESIAN_POINT('Ctrl Pts',(-90.,11.1703426294259,3.00346961322391));
#34804=CARTESIAN_POINT('Ctrl Pts',(-90.,11.1935524561946,2.90314261566199));
#34805=CARTESIAN_POINT('Ctrl Pts',(-90.,11.2154462823607,2.80246220808664));
#34806=CARTESIAN_POINT('Ctrl Pts',(-90.,11.2360108513013,2.70145432537238));
#34807=CARTESIAN_POINT('Ctrl Pts',(-90.,11.2500737341414,2.63238105548534));
#34808=CARTESIAN_POINT('Ctrl Pts',(-90.,11.2635149851746,2.56315464787577));
#34809=CARTESIAN_POINT('Ctrl Pts',(-90.,11.2763300877809,2.49378343749949));
#34810=CARTESIAN_POINT('Ctrl Pts',(-90.,11.281580840756,2.46535985787929));
#34811=CARTESIAN_POINT('Ctrl Pts',(-90.,11.2867263799758,2.43691228547538));
#34812=CARTESIAN_POINT('Ctrl Pts',(-90.,11.2917640894315,2.40845488838702));
#34813=CARTESIAN_POINT('Ctrl Pts',(-90.,11.3399768555613,2.13610694086531));
#34814=CARTESIAN_POINT('Ctrl Pts',(-90.,11.3783768067611,1.86254282314492));
#34815=CARTESIAN_POINT('Ctrl Pts',(-90.,11.4068617806356,1.58827966874211));
#34816=CARTESIAN_POINT('Ctrl Pts',(-90.,11.4352887946213,1.31457457214283));
#34817=CARTESIAN_POINT('Ctrl Pts',(-90.,11.4538412446679,1.04017266307592));
#34818=CARTESIAN_POINT('Ctrl Pts',(-90.,11.4623666776379,0.765579031056406));
#34819=CARTESIAN_POINT('Ctrl Pts',(-90.,11.4645277885494,0.695972326451475));
#34820=CARTESIAN_POINT('Ctrl Pts',(-90.,11.4660443321508,0.626353283748583));
#34821=CARTESIAN_POINT('Ctrl Pts',(-90.,11.4669132910905,0.556730111859395));
#34822=CARTESIAN_POINT('Ctrl Pts',(-90.,11.4703524607466,0.281175204517033));
#34823=CARTESIAN_POINT('Ctrl Pts',(-90.,11.4636517873567,0.0055550935556139));
#34824=CARTESIAN_POINT('Ctrl Pts',(-90.,11.4469479467724,-0.269598067443254));
#34825=CARTESIAN_POINT('Ctrl Pts',(-90.,11.4302653802983,-0.544400791748682));
#34826=CARTESIAN_POINT('Ctrl Pts',(-90.,11.4036049324252,-0.818738377219698));
#34827=CARTESIAN_POINT('Ctrl Pts',(-90.,11.3670523229692,-1.09206872465835));
#34828=CARTESIAN_POINT('Ctrl Pts',(-90.,11.3447418592934,-1.25890022803875));
#34829=CARTESIAN_POINT('Ctrl Pts',(-90.,11.3187451354215,-1.42535621584432));
#34830=CARTESIAN_POINT('Ctrl Pts',(-90.,11.2890728104253,-1.59130971323021));
#34831=CARTESIAN_POINT('Ctrl Pts',(-90.,11.2760911682395,-1.66391436833653));
#34832=CARTESIAN_POINT('Ctrl Pts',(-90.,11.2624059083653,-1.73642280066201));
#34833=CARTESIAN_POINT('Ctrl Pts',(-90.,11.24801753262,-1.8088241590467));
#34834=CARTESIAN_POINT('Ctrl Pts',(-90.,11.2386133705796,-1.85614528258763));
#34835=CARTESIAN_POINT('Ctrl Pts',(-90.,11.2289088427027,-1.90342066283882));
#34836=CARTESIAN_POINT('Ctrl Pts',(-90.,11.2189040351068,-1.95064723561348));
#34837=CARTESIAN_POINT('Ctrl Pts',(-90.,11.2135629399335,-1.97585927667222));
#34838=CARTESIAN_POINT('Ctrl Pts',(-90.,11.2081367261043,-2.00105513468646));
#34839=CARTESIAN_POINT('Ctrl Pts',(-90.,11.2026273691943,-2.02622584437508));
#34840=CARTESIAN_POINT('Ctrl Pts',(-90.,11.1440984837332,-2.29362794019419));
#34841=CARTESIAN_POINT('Ctrl Pts',(-90.,11.0761321356989,-2.55846899415871));
#34842=CARTESIAN_POINT('Ctrl Pts',(-90.,10.9989076859169,-2.82024219140262));
#34843=CARTESIAN_POINT('Ctrl Pts',(-90.,10.9216242802013,-3.0822152357584));
#34844=CARTESIAN_POINT('Ctrl Pts',(-90.,10.8350684457149,-3.34111635466465));
#34845=CARTESIAN_POINT('Ctrl Pts',(-90.,10.7393689679669,-3.59642631329222));
#34846=CARTESIAN_POINT('Ctrl Pts',(-90.,10.6445416932764,-3.84940938224622));
#34847=CARTESIAN_POINT('Ctrl Pts',(-90.,10.5407364399718,-4.0988670139967));
#34848=CARTESIAN_POINT('Ctrl Pts',(-90.,10.4280318007549,-4.34427424590613));
#34849=CARTESIAN_POINT('Ctrl Pts',(-90.,10.3389543367021,-4.53823479651512));
#34850=CARTESIAN_POINT('Ctrl Pts',(-90.,10.2443167396394,-4.72966489136653));
#34851=CARTESIAN_POINT('Ctrl Pts',(-90.,10.1441383060101,-4.91829300030524));
#34852=CARTESIAN_POINT('Ctrl Pts',(-90.,10.0350500930934,-5.12369752266081));
#34853=CARTESIAN_POINT('Ctrl Pts',(-90.,9.91939159180428,-5.32577984787966));
#34854=CARTESIAN_POINT('Ctrl Pts',(-90.,9.79736644993105,-5.52427284227006));
#34855=CARTESIAN_POINT('Ctrl Pts',(-90.,9.74398045036152,-5.61111352731585));
#34856=CARTESIAN_POINT('Ctrl Pts',(-90.,9.68937558727447,-5.69726693803969));
#34857=CARTESIAN_POINT('Ctrl Pts',(-90.,9.63356781953306,-5.78270944804998));
#34858=CARTESIAN_POINT('Ctrl Pts',(-90.,9.5976005282019,-5.83777589800808));
#34859=CARTESIAN_POINT('Ctrl Pts',(-90.,9.56113358369664,-5.89254705121343));
#34860=CARTESIAN_POINT('Ctrl Pts',(-90.,9.5241711249039,-5.94701640003021));
#34861=CARTESIAN_POINT('Ctrl Pts',(-90.,9.50389726234252,-5.9768927699414));
#34862=CARTESIAN_POINT('Ctrl Pts',(-90.,9.4834724625547,-6.00668093496707));
#34863=CARTESIAN_POINT('Ctrl Pts',(-90.,9.46291188231344,-6.03635915674249));
#34864=CARTESIAN_POINT('Ctrl Pts',(-90.,9.30976555255365,-6.25741861544314));
#34865=CARTESIAN_POINT('Ctrl Pts',(-90.,9.14893478031223,-6.47261211276324));
#34866=CARTESIAN_POINT('Ctrl Pts',(-90.,8.98082954059386,-6.68160127162625));
#34867=CARTESIAN_POINT('Ctrl Pts',(-90.,8.81151510059202,-6.89209371349556));
#34868=CARTESIAN_POINT('Ctrl Pts',(-90.,8.63482075206015,-7.09629271941038));
#34869=CARTESIAN_POINT('Ctrl Pts',(-90.,8.45112207888021,-7.2938225125168));
#34870=CARTESIAN_POINT('Ctrl Pts',(-90.,8.26780812280964,-7.49093862222691));
#34871=CARTESIAN_POINT('Ctrl Pts',(-90.,8.07751868545223,-7.6814138584871));
#34872=CARTESIAN_POINT('Ctrl Pts',(-90.,7.88059071023121,-7.86483819093346));
#34873=CARTESIAN_POINT('Ctrl Pts',(-90.,7.68518613482991,-8.04684358534082));
#34874=CARTESIAN_POINT('Ctrl Pts',(-90.,7.48324486788944,-8.22190712647571));
#34875=CARTESIAN_POINT('Ctrl Pts',(-90.,7.27506729716046,-8.38958611218002));
#34876=CARTESIAN_POINT('Ctrl Pts',(-90.,7.07054495646357,-8.55432095139367));
#34877=CARTESIAN_POINT('Ctrl Pts',(-90.,6.86000293117097,-8.71192855691827));
#34878=CARTESIAN_POINT('Ctrl Pts',(-90.,6.6437050061379,-8.86194356787701));
#34879=CARTESIAN_POINT('Ctrl Pts',(-90.,6.57120824497411,-8.91222422784541));
#34880=CARTESIAN_POINT('Ctrl Pts',(-90.,6.49806472103886,-8.96165153702105));
#34881=CARTESIAN_POINT('Ctrl Pts',(-90.,6.42428395783973,-9.01020671414053));
#34882=CARTESIAN_POINT('',(-90.,-6.42475130859185,-9.01043996637154));
#34883=CARTESIAN_POINT('Origin',(-90.,0.,0.));
#34884=CARTESIAN_POINT('Ctrl Pts',(-90.,-6.42475130859154,-9.01043996637175));
#34885=CARTESIAN_POINT('Ctrl Pts',(-90.,-6.65061596671456,-8.86211493166386));
#34886=CARTESIAN_POINT('Ctrl Pts',(-89.9999999999999,-6.87072984044529,
-8.70566715326926));
#34887=CARTESIAN_POINT('Ctrl Pts',(-89.9999999999999,-7.08460872649498,
-8.54135125534634));
#34888=CARTESIAN_POINT('Ctrl Pts',(-89.9999999999999,-7.09832383863764,
-8.53081439961243));
#34889=CARTESIAN_POINT('Ctrl Pts',(-89.9999999999999,-7.11201330530386,
-8.52024517293795));
#34890=CARTESIAN_POINT('Ctrl Pts',(-89.9999999999999,-7.12567699593402,
-8.50964363574394));
#34891=CARTESIAN_POINT('Ctrl Pts',(-89.9999999999999,-7.33729564816288,
-8.34545058766665));
#34892=CARTESIAN_POINT('Ctrl Pts',(-90.,-7.54273377508571,-8.17351106236173));
#34893=CARTESIAN_POINT('Ctrl Pts',(-90.,-7.74171723733581,-7.9942942910195));
#34894=CARTESIAN_POINT('Ctrl Pts',(-90.,-7.94191952622316,-7.81397976927991));
#34895=CARTESIAN_POINT('Ctrl Pts',(-89.9999999999999,-8.13558827492983,
-7.62629814154647));
#34896=CARTESIAN_POINT('Ctrl Pts',(-89.9999999999999,-8.32241215048194,
-7.43168519135534));
#34897=CARTESIAN_POINT('Ctrl Pts',(-89.9999999999999,-8.38001350953885,
-7.37168231223749));
#34898=CARTESIAN_POINT('Ctrl Pts',(-89.9999999999999,-8.43696393552139,
-7.31102026254922));
#34899=CARTESIAN_POINT('Ctrl Pts',(-89.9999999999999,-8.49325359145673,
-7.24971111436292));
#34900=CARTESIAN_POINT('Ctrl Pts',(-89.9999999999999,-8.52511339921065,
-7.21501028625668));
#34901=CARTESIAN_POINT('Ctrl Pts',(-89.9999999999999,-8.5567615207414,-7.18010215242168));
#34902=CARTESIAN_POINT('Ctrl Pts',(-89.9999999999999,-8.58819612090012,
-7.14498885930322));
#34903=CARTESIAN_POINT('Ctrl Pts',(-89.9999999999999,-8.61211097529082,
-7.11827532428557));
#34904=CARTESIAN_POINT('Ctrl Pts',(-90.,-8.63590251481974,-7.09144266968923));
#34905=CARTESIAN_POINT('Ctrl Pts',(-90.,-8.65955976364048,-7.06450359547617));
#34906=CARTESIAN_POINT('Ctrl Pts',(-90.,-8.83805698972194,-6.8612445412781));
#34907=CARTESIAN_POINT('Ctrl Pts',(-90.,-9.00905478459883,-6.6517718956029));
#34908=CARTESIAN_POINT('Ctrl Pts',(-90.,-9.17227989292783,-6.4365623541276));
#34909=CARTESIAN_POINT('Ctrl Pts',(-90.,-9.33663083357885,-6.2198684217992));
#34910=CARTESIAN_POINT('Ctrl Pts',(-90.,-9.49310194101511,-5.99735772885397));
#34911=CARTESIAN_POINT('Ctrl Pts',(-90.,-9.64137918380223,-5.76947781861025));
#34912=CARTESIAN_POINT('Ctrl Pts',(-90.,-9.78920952329607,-5.54228473178221));
#34913=CARTESIAN_POINT('Ctrl Pts',(-90.,-9.9288957109934,-5.30975423589191));
#34914=CARTESIAN_POINT('Ctrl Pts',(-90.,-10.0600855719573,-5.07229842674199));
#34915=CARTESIAN_POINT('Ctrl Pts',(-90.,-10.1025381524142,-4.99545855688614));
#34916=CARTESIAN_POINT('Ctrl Pts',(-90.,-10.1441006967004,-4.9181027202424));
#34917=CARTESIAN_POINT('Ctrl Pts',(-90.,-10.184760241468,-4.8402443089206));
#34918=CARTESIAN_POINT('Ctrl Pts',(-90.,-10.2071957271072,-4.79728290148023));
#34919=CARTESIAN_POINT('Ctrl Pts',(-90.,-10.2293562663178,-4.7541684701326));
#34920=CARTESIAN_POINT('Ctrl Pts',(-90.,-10.2512396111472,-4.71090323342713));
#34921=CARTESIAN_POINT('Ctrl Pts',(-90.,-10.2652344513955,-4.68323424220498));
#34922=CARTESIAN_POINT('Ctrl Pts',(-90.,-10.2791136353224,-4.65550804712252));
#34923=CARTESIAN_POINT('Ctrl Pts',(-90.,-10.2928733408437,-4.62773215676248));
#34924=CARTESIAN_POINT('Ctrl Pts',(-90.,-10.3745756942675,-4.46280452750792));
#34925=CARTESIAN_POINT('Ctrl Pts',(-90.,-10.4521032429591,-4.29605217209308));
#34926=CARTESIAN_POINT('Ctrl Pts',(-90.,-10.5253730189402,-4.12761863166149));
#34927=CARTESIAN_POINT('Ctrl Pts',(-90.,-10.633017677609,-3.8801636514142));
#34928=CARTESIAN_POINT('Ctrl Pts',(-90.,-10.7314745633192,-3.62908127751788));
#34929=CARTESIAN_POINT('Ctrl Pts',(-90.,-10.820768106391,-3.37492377019595));
#34930=CARTESIAN_POINT('Ctrl Pts',(-90.,-10.911052892199,-3.11794487429105));
#34931=CARTESIAN_POINT('Ctrl Pts',(-90.,-10.9919699583455,-2.85782164311628));
#34932=CARTESIAN_POINT('Ctrl Pts',(-90.,-11.0634983479278,-2.59509741224024));
#34933=CARTESIAN_POINT('Ctrl Pts',(-90.,-11.135398801024,-2.33100658970638));
#34934=CARTESIAN_POINT('Ctrl Pts',(-90.,-11.1978128183106,-2.06428703600773));
#34935=CARTESIAN_POINT('Ctrl Pts',(-90.,-11.2506700006432,-1.7954717017297));
#34936=CARTESIAN_POINT('Ctrl Pts',(-90.,-11.3030143363181,-1.52926454744956));
#34937=CARTESIAN_POINT('Ctrl Pts',(-90.,-11.34598643978,-1.26100146289971));
#34938=CARTESIAN_POINT('Ctrl Pts',(-90.,-11.3794684511118,-0.991190731214159));
#34939=CARTESIAN_POINT('Ctrl Pts',(-90.,-11.3920242053612,-0.890011706832077));
#34940=CARTESIAN_POINT('Ctrl Pts',(-90.,-11.4032449091829,-0.788614997625171));
#34941=CARTESIAN_POINT('Ctrl Pts',(-90.,-11.4131225018002,-0.687027337826157));
#34942=CARTESIAN_POINT('Ctrl Pts',(-90.,-11.4195212522844,-0.621218378851216));
#34943=CARTESIAN_POINT('Ctrl Pts',(-90.,-11.4253563443557,-0.555329287367791));
#34944=CARTESIAN_POINT('Ctrl Pts',(-90.,-11.4306253562291,-0.489367343649453));
#34945=CARTESIAN_POINT('Ctrl Pts',(-90.,-11.4328878359414,-0.461043710484138));
#34946=CARTESIAN_POINT('Ctrl Pts',(-90.,-11.4350458220249,-0.432707732928388));
#34947=CARTESIAN_POINT('Ctrl Pts',(-90.,-11.4370983178205,-0.404372587164961));
#34948=CARTESIAN_POINT('Ctrl Pts',(-90.,-11.4570807825108,-0.128510365709557));
#34949=CARTESIAN_POINT('Ctrl Pts',(-90.,-11.4670944941131,0.147589620248241));
#34950=CARTESIAN_POINT('Ctrl Pts',(-90.,-11.4671365005577,0.423375648430594));
#34951=CARTESIAN_POINT('Ctrl Pts',(-90.,-11.4671787076057,0.700478703366769));
#34952=CARTESIAN_POINT('Ctrl Pts',(-90.,-11.4571538896401,0.977265418803752));
#34953=CARTESIAN_POINT('Ctrl Pts',(-90.,-11.4370088281763,1.25319083488204));
#34954=CARTESIAN_POINT('Ctrl Pts',(-90.,-11.432234510889,1.31858430545373));
#34955=CARTESIAN_POINT('Ctrl Pts',(-90.,-11.4268915378888,1.38392943996235));
#34956=CARTESIAN_POINT('Ctrl Pts',(-90.,-11.4209787755945,1.44921904475968));
#34957=CARTESIAN_POINT('Ctrl Pts',(-90.,-11.3961509419423,1.72337169396549));
#34958=CARTESIAN_POINT('Ctrl Pts',(-90.,-11.3612808807937,1.99654535611728));
#34959=CARTESIAN_POINT('Ctrl Pts',(-90.,-11.3166035627522,2.26824946846252));
#34960=CARTESIAN_POINT('Ctrl Pts',(-90.,-11.271735562689,2.54111320926694));
#34961=CARTESIAN_POINT('Ctrl Pts',(-90.,-11.2169762691305,2.81249543474008));
#34962=CARTESIAN_POINT('Ctrl Pts',(-90.,-11.1525113673841,3.0818928412696));
#34963=CARTESIAN_POINT('Ctrl Pts',(-90.,-11.1122274203988,3.25023856969861));
#34964=CARTESIAN_POINT('Ctrl Pts',(-90.,-11.0681524360867,3.41780907298995));
#34965=CARTESIAN_POINT('Ctrl Pts',(-90.,-11.0203218032741,3.58447865336719));
#34966=CARTESIAN_POINT('Ctrl Pts',(-90.,-10.9993959014186,3.65739659478223));
#34967=CARTESIAN_POINT('Ctrl Pts',(-90.,-10.9777510486049,3.73014205804691));
#34968=CARTESIAN_POINT('Ctrl Pts',(-90.,-10.9553897639952,3.80270433013029));
#34969=CARTESIAN_POINT('Ctrl Pts',(-90.,-10.9412121665118,3.84871057279642));
#34970=CARTESIAN_POINT('Ctrl Pts',(-90.,-10.9267465675327,3.89464317259038));
#34971=CARTESIAN_POINT('Ctrl Pts',(-90.,-10.9119935538308,3.94049937157543));
#34972=CARTESIAN_POINT('Ctrl Pts',(-90.,-10.9032483052371,3.96768187596365));
#34973=CARTESIAN_POINT('Ctrl Pts',(-90.,-10.89440279516,3.99483517031346));
#34974=CARTESIAN_POINT('Ctrl Pts',(-90.,-10.8854606880556,4.02194834272));
#34975=CARTESIAN_POINT('Ctrl Pts',(-90.,-10.798021459592,4.2870709641265));
#34976=CARTESIAN_POINT('Ctrl Pts',(-90.,-10.7012600918437,4.54863915252615));
#34977=CARTESIAN_POINT('Ctrl Pts',(-90.,-10.5954597983809,4.80616392461528));
#34978=CARTESIAN_POINT('Ctrl Pts',(-90.,-10.4890736553727,5.06511469247184));
#34979=CARTESIAN_POINT('Ctrl Pts',(-90.,-10.373548046733,5.31997775056167));
#34980=CARTESIAN_POINT('Ctrl Pts',(-90.,-10.2491181879724,5.57025027534674));
#34981=CARTESIAN_POINT('Ctrl Pts',(-90.,-10.1249181352476,5.82006057878593));
#34982=CARTESIAN_POINT('Ctrl Pts',(-90.,-9.99184647791854,6.06529789265079));
#34983=CARTESIAN_POINT('Ctrl Pts',(-90.,-9.85008764641507,6.30544744759558));
#34984=CARTESIAN_POINT('Ctrl Pts',(-90.,-9.7374400125352,6.49628056081274));
#34985=CARTESIAN_POINT('Ctrl Pts',(-90.,-9.61930580768373,6.6839008000223));
#34986=CARTESIAN_POINT('Ctrl Pts',(-90.,-9.49575654832475,6.86803937657834));
#34987=CARTESIAN_POINT('Ctrl Pts',(-90.,-9.35867483321646,7.07234680847123));
#34988=CARTESIAN_POINT('Ctrl Pts',(-90.,-9.21492707314738,7.27236859511388));
#34989=CARTESIAN_POINT('Ctrl Pts',(-90.,-9.06478201620882,7.46786749211994));
#34990=CARTESIAN_POINT('Ctrl Pts',(-90.,-8.9990935537982,7.5533982595601));
#34991=CARTESIAN_POINT('Ctrl Pts',(-90.,-8.93218029389725,7.63806306074812));
#34992=CARTESIAN_POINT('Ctrl Pts',(-90.,-8.86406334867798,7.72184075141948));
#34993=CARTESIAN_POINT('Ctrl Pts',(-90.,-8.82362294761177,7.77157879237602));
#34994=CARTESIAN_POINT('Ctrl Pts',(-90.,-8.78275826967116,7.82100413914672));
#34995=CARTESIAN_POINT('Ctrl Pts',(-90.,-8.74147360307109,7.8701122254124));
#34996=CARTESIAN_POINT('Ctrl Pts',(-90.,-8.7177941394386,7.89827893326192));
#34997=CARTESIAN_POINT('Ctrl Pts',(-90.,-8.69397447251461,7.92634356643258));
#34998=CARTESIAN_POINT('Ctrl Pts',(-90.,-8.67003176357098,7.95428637439746));
#34999=CARTESIAN_POINT('Ctrl Pts',(-90.,-8.48862974410169,8.16599515832848));
#35000=CARTESIAN_POINT('Ctrl Pts',(-90.,-8.2999844948834,8.37093434225391));
#35001=CARTESIAN_POINT('Ctrl Pts',(-90.,-8.10458119986093,8.56883289310171));
#35002=CARTESIAN_POINT('Ctrl Pts',(-90.,-7.90691879422699,8.76901940289187));
#35003=CARTESIAN_POINT('Ctrl Pts',(-90.,-7.70234081506854,8.96200199713272));
#35004=CARTESIAN_POINT('Ctrl Pts',(-90.,-7.49130282760398,9.14747446805371));
#35005=CARTESIAN_POINT('Ctrl Pts',(-90.,-7.27896365425757,9.3340904968883));
#35006=CARTESIAN_POINT('Ctrl Pts',(-90.,-7.06008414942282,9.51310396944825));
#35007=CARTESIAN_POINT('Ctrl Pts',(-90.,-6.83508736441859,9.68417023041306));
#35008=CARTESIAN_POINT('Ctrl Pts',(-90.,-6.61081877650966,9.85468283922532));
#35009=CARTESIAN_POINT('Ctrl Pts',(-90.,-6.38047196958125,10.0173000112399));
#35010=CARTESIAN_POINT('Ctrl Pts',(-90.,-6.14443205975055,10.1716414832551));
#35011=CARTESIAN_POINT('Ctrl Pts',(-90.,-5.91150572303173,10.323947056097));
#35012=CARTESIAN_POINT('Ctrl Pts',(-90.,-5.67303499954604,10.468194147758));
#35013=CARTESIAN_POINT('Ctrl Pts',(-90.,-5.42936414325409,10.6039739276061));
#35014=CARTESIAN_POINT('Ctrl Pts',(-90.,-5.33030982339919,10.6591695876353));
#35015=CARTESIAN_POINT('Ctrl Pts',(-90.,-5.23039592609036,10.7129654986999));
#35016=CARTESIAN_POINT('Ctrl Pts',(-90.,-5.12964461189318,10.765331911078));
#35017=CARTESIAN_POINT('Origin',(-92.9267766952966,0.,-4.79034268955998E-16));
#35018=CARTESIAN_POINT('',(-93.3535533905933,15.6464466094067,1.91613707582399E-15));
#35019=CARTESIAN_POINT('',(-92.9267766952966,15.8232233047034,1.93778597722988E-15));
#35020=CARTESIAN_POINT('',(-93.3535533905933,-15.6464466094067,-1.91613707582399E-15));
#35021=CARTESIAN_POINT('Origin',(-93.3535533905933,0.,-9.58068537911996E-16));
#35022=CARTESIAN_POINT('Origin',(-93.3535533905933,0.,-9.58068537911996E-16));
#35023=CARTESIAN_POINT('Origin',(-93.5,0.,0.));
#35024=CARTESIAN_POINT('',(-93.6464466094067,-15.3535533905933,-1.88026800153281E-15));
#35025=CARTESIAN_POINT('',(-93.5,-15.5,-1.8982025386784E-15));
#35026=CARTESIAN_POINT('',(-93.6464466094067,15.3535533905933,-1.88026800153281E-15));
#35027=CARTESIAN_POINT('Origin',(-93.6464466094067,0.,-9.40134000766403E-16));
#35028=CARTESIAN_POINT('Origin',(-93.6464466094067,0.,-9.40134000766403E-16));
#35029=CARTESIAN_POINT('Origin',(-93.8232233047034,0.,-4.70067000383201E-16));
#35030=CARTESIAN_POINT('',(-94.,14.5,1.77573785876366E-15));
#35031=CARTESIAN_POINT('',(-93.8232233047034,14.9267766952966,1.82800293014823E-15));
#35032=CARTESIAN_POINT('Origin',(-94.,0.,0.));
#35033=CARTESIAN_POINT('Origin',(-94.,15.,0.));
#35034=CARTESIAN_POINT('',(-94.,5.5,-3.17542648054294));
#35035=CARTESIAN_POINT('',(-94.,-3.88578058618805E-15,-6.35085296108589));
#35036=CARTESIAN_POINT('',(-94.,7.125,-2.2372322931098));
#35037=CARTESIAN_POINT('',(-94.,5.5,3.17542648054294));
#35038=CARTESIAN_POINT('',(-94.,5.5,-1.44337567297406));
#35039=CARTESIAN_POINT('',(-94.,-6.66133814775094E-15,6.35085296108589));
#35040=CARTESIAN_POINT('',(-94.,9.625,0.793856620135735));
#35041=CARTESIAN_POINT('',(-94.,-5.50000000000001,3.17542648054294));
#35042=CARTESIAN_POINT('',(-94.,4.125,8.73242282149309));
#35043=CARTESIAN_POINT('',(-94.,-5.5,-3.17542648054295));
#35044=CARTESIAN_POINT('',(-94.,-5.5,1.44337567297406));
#35045=CARTESIAN_POINT('',(-94.,1.625,-7.28904714851903));
#35046=CARTESIAN_POINT('Origin',(-93.75,4.25,8.51591647054698));
#35047=CARTESIAN_POINT('',(-93.5,3.53525079574969E-16,5.77350269189626));
#35048=CARTESIAN_POINT('',(-94.,-4.44089209850063E-15,6.35085296108589));
#35049=CARTESIAN_POINT('',(-93.5,-5.,2.88675134594813));
#35050=CARTESIAN_POINT('',(-93.5,4.375,8.29941011960087));
#35051=CARTESIAN_POINT('',(-94.,-5.5,3.17542648054295));
#35052=CARTESIAN_POINT('Origin',(-93.75,9.5,0.577350269189625));
#35053=CARTESIAN_POINT('',(-93.5,5.,2.88675134594813));
#35054=CARTESIAN_POINT('',(-94.,5.5,3.17542648054294));
#35055=CARTESIAN_POINT('',(-93.5,9.375,0.360843918243515));
#35056=CARTESIAN_POINT('Origin',(-93.75,7.,-2.02072594216369));
#35057=CARTESIAN_POINT('',(-93.5,-1.06057523872491E-15,-5.77350269189626));
#35058=CARTESIAN_POINT('',(-94.,-3.88578058618805E-15,-6.35085296108589));
#35059=CARTESIAN_POINT('',(-93.5,5.,-2.88675134594813));
#35060=CARTESIAN_POINT('',(-93.5,6.875,-1.80421959121758));
#35061=CARTESIAN_POINT('',(-93.5,5.,-2.88675134594813));
#35062=CARTESIAN_POINT('Origin',(-93.75,1.75,-7.07254079757292));
#35063=CARTESIAN_POINT('',(-93.5,-5.,-2.88675134594813));
#35064=CARTESIAN_POINT('',(-93.5,1.875,-6.85603444662681));
#35065=CARTESIAN_POINT('',(-94.,-5.5,-3.17542648054295));
#35066=CARTESIAN_POINT('Origin',(-93.75,5.25,-1.44337567297406));
#35067=CARTESIAN_POINT('',(-93.5,5.,-1.44337567297406));
#35068=CARTESIAN_POINT('Origin',(-93.75,-5.25,1.44337567297406));
#35069=CARTESIAN_POINT('',(-93.5,-5.,1.44337567297406));
#35070=CARTESIAN_POINT('Origin',(-94.,5.,2.88675134594813));
#35071=CARTESIAN_POINT('',(-89.,5.,2.88675134594813));
#35072=CARTESIAN_POINT('',(-94.,5.,2.88675134594813));
#35073=CARTESIAN_POINT('',(-89.,5.55111512312578E-16,5.77350269189626));
#35074=CARTESIAN_POINT('',(-89.,5.,2.88675134594813));
#35075=CARTESIAN_POINT('',(-94.,3.53525079574969E-16,5.77350269189626));
#35076=CARTESIAN_POINT('Origin',(-94.,5.,-2.88675134594813));
#35077=CARTESIAN_POINT('',(-89.,5.,-2.88675134594813));
#35078=CARTESIAN_POINT('',(-94.,5.,-2.88675134594813));
#35079=CARTESIAN_POINT('',(-89.,5.,-2.88675134594813));
#35080=CARTESIAN_POINT('Origin',(-94.,-1.06057523872491E-15,-5.77350269189626));
#35081=CARTESIAN_POINT('',(-89.,-1.11022302462516E-15,-5.77350269189626));
#35082=CARTESIAN_POINT('',(-94.,-1.06057523872491E-15,-5.77350269189626));
#35083=CARTESIAN_POINT('',(-89.,-1.06057523872491E-15,-5.77350269189626));
#35084=CARTESIAN_POINT('Origin',(-81.425,1.39622887047493E-15,0.));
#35085=CARTESIAN_POINT('',(-81.425,9.46357049537274,-7.25578792958495));
#35086=CARTESIAN_POINT('Ctrl Pts',(-81.425,-10.1493211523489,-4.41097929944942));
#35087=CARTESIAN_POINT('Ctrl Pts',(-81.425,-10.0511972777313,-4.66274678383263));
#35088=CARTESIAN_POINT('Ctrl Pts',(-81.425,-9.94393250654178,-4.91057796500162));
#35089=CARTESIAN_POINT('Ctrl Pts',(-81.425,-9.82767522759895,-5.15394628116773));
#35090=CARTESIAN_POINT('Ctrl Pts',(-81.425,-9.82022016054204,-5.16955241897728));
#35091=CARTESIAN_POINT('Ctrl Pts',(-81.425,-9.81272809794668,-5.18514020202351));
#35092=CARTESIAN_POINT('Ctrl Pts',(-81.425,-9.80519907176881,-5.20070949003747));
#35093=CARTESIAN_POINT('Ctrl Pts',(-81.425,-9.68859202725284,-5.44184142631154));
#35094=CARTESIAN_POINT('Ctrl Pts',(-81.425,-9.56312278215398,-5.67853847881199));
#35095=CARTESIAN_POINT('Ctrl Pts',(-81.425,-9.42919331651251,-5.91043494040433));
#35096=CARTESIAN_POINT('Ctrl Pts',(-81.425,-9.29444350025844,-6.1437518243318));
#35097=CARTESIAN_POINT('Ctrl Pts',(-81.425,-9.15112916840663,-6.37220964860501));
#35098=CARTESIAN_POINT('Ctrl Pts',(-81.425,-8.99961185123732,-6.59541327943604));
#35099=CARTESIAN_POINT('Ctrl Pts',(-81.425,-8.95289617696045,-6.66423120936062));
#35100=CARTESIAN_POINT('Ctrl Pts',(-81.425,-8.90540040001368,-6.73254947992113));
#35101=CARTESIAN_POINT('Ctrl Pts',(-81.425,-8.85713428342694,-6.8003559591904));
#35102=CARTESIAN_POINT('Ctrl Pts',(-81.425,-8.82981577402108,-6.83873426829606));
#35103=CARTESIAN_POINT('Ctrl Pts',(-81.425,-8.80225047688398,-6.87694861825185));
#35104=CARTESIAN_POINT('Ctrl Pts',(-81.425,-8.774440110005,-6.91499676774056));
#35105=CARTESIAN_POINT('Ctrl Pts',(-81.425,-8.75328251436771,-6.94394307273295));
#35106=CARTESIAN_POINT('Ctrl Pts',(-81.425,-8.73198276368499,-6.97279352399088));
#35107=CARTESIAN_POINT('Ctrl Pts',(-81.425,-8.71055099837558,-7.00153474506046));
#35108=CARTESIAN_POINT('Ctrl Pts',(-81.425,-8.5488453047104,-7.21839131393111));
#35109=CARTESIAN_POINT('Ctrl Pts',(-81.425,-8.37950258163264,-7.4292042102773));
#35110=CARTESIAN_POINT('Ctrl Pts',(-81.425,-8.2029322943441,-7.63360703972012));
#35111=CARTESIAN_POINT('Ctrl Pts',(-81.425,-8.02514413249846,-7.83941971568467));
#35112=CARTESIAN_POINT('Ctrl Pts',(-81.425,-7.84002801022476,-8.03873412469252));
#35113=CARTESIAN_POINT('Ctrl Pts',(-81.425,-7.64795639954535,-8.23115004848213));
#35114=CARTESIAN_POINT('Ctrl Pts',(-81.425,-7.45646368826431,-8.42298603512162));
#35115=CARTESIAN_POINT('Ctrl Pts',(-81.425,-7.2580569377017,-8.60796554982375));
#35116=CARTESIAN_POINT('Ctrl Pts',(-81.425,-7.05306601649295,-8.78565843431322));
#35117=CARTESIAN_POINT('Ctrl Pts',(-81.425,-6.98673167123628,-8.84315923034786));
#35118=CARTESIAN_POINT('Ctrl Pts',(-81.425,-6.91970758521381,-8.89989671529736));
#35119=CARTESIAN_POINT('Ctrl Pts',(-81.425,-6.85200416263363,-8.95585542472905));
#35120=CARTESIAN_POINT('Ctrl Pts',(-81.425,-6.81464616008689,-8.98673282397701));
#35121=CARTESIAN_POINT('Ctrl Pts',(-81.425,-6.77708131288144,-9.01737310047241));
#35122=CARTESIAN_POINT('Ctrl Pts',(-81.425,-6.73931132370747,-9.04777359412434));
#35123=CARTESIAN_POINT('Ctrl Pts',(-81.425,-6.71515665375601,-9.06721532303619));
#35124=CARTESIAN_POINT('Ctrl Pts',(-81.425,-6.69092198364463,-9.08655581632656));
#35125=CARTESIAN_POINT('Ctrl Pts',(-81.425,-6.66661386320815,-9.1057897743195));
#35126=CARTESIAN_POINT('Ctrl Pts',(-81.425,-6.52227718275629,-9.21999710910322));
#35127=CARTESIAN_POINT('Ctrl Pts',(-81.425,-6.37528765951429,-9.33050025169547));
#35128=CARTESIAN_POINT('Ctrl Pts',(-81.425,-6.22576844769021,-9.43718820340569));
#35129=CARTESIAN_POINT('Ctrl Pts',(-81.425,-6.00610153703119,-9.59392935038481));
#35130=CARTESIAN_POINT('Ctrl Pts',(-81.425,-5.78097625235967,-9.74243767872015));
#35131=CARTESIAN_POINT('Ctrl Pts',(-81.425,-5.55093786621179,-9.88262226273903));
#35132=CARTESIAN_POINT('Ctrl Pts',(-81.425,-5.31834583144998,-10.0243630312481));
#35133=CARTESIAN_POINT('Ctrl Pts',(-81.425,-5.0807305129784,-10.1575945320724));
#35134=CARTESIAN_POINT('Ctrl Pts',(-81.425,-4.83861901722481,-10.2821832996586));
#35135=CARTESIAN_POINT('Ctrl Pts',(-81.425,-4.59524814941176,-10.4074201307014));
#35136=CARTESIAN_POINT('Ctrl Pts',(-81.425,-4.34733365355969,-10.5239243712292));
#35137=CARTESIAN_POINT('Ctrl Pts',(-81.425,-4.09538219844386,-10.6315163530296));
#35138=CARTESIAN_POINT('Ctrl Pts',(-81.425,-3.84587529675822,-10.7380644260021));
#35139=CARTESIAN_POINT('Ctrl Pts',(-81.425,-3.59240879618425,-10.8358725233087));
#35140=CARTESIAN_POINT('Ctrl Pts',(-81.425,-3.33545536944063,-10.9247196817515));
#35141=CARTESIAN_POINT('Ctrl Pts',(-81.425,-3.23909783441178,-10.9580373661676));
#35142=CARTESIAN_POINT('Ctrl Pts',(-81.425,-3.14224979922048,-10.9900944331567));
#35143=CARTESIAN_POINT('Ctrl Pts',(-81.425,-3.0449357380293,-11.0208774396873));
#35144=CARTESIAN_POINT('Ctrl Pts',(-81.425,-2.98189523387823,-11.0408188153449));
#35145=CARTESIAN_POINT('Ctrl Pts',(-81.425,-2.91865915728009,-11.0602255101925));
#35146=CARTESIAN_POINT('Ctrl Pts',(-81.425,-2.85523412591873,-11.0790936417007));
#35147=CARTESIAN_POINT('Ctrl Pts',(-81.425,-2.82799982747709,-11.0871954953932));
#35148=CARTESIAN_POINT('Ctrl Pts',(-81.425,-2.80073172898171,-11.0951977054104));
#35149=CARTESIAN_POINT('Ctrl Pts',(-81.425,-2.77344251147326,-11.1030965573882));
#35150=CARTESIAN_POINT('Ctrl Pts',(-81.425,-2.50776312916618,-11.1799973374758));
#35151=CARTESIAN_POINT('Ctrl Pts',(-81.425,-2.23977856115638,-11.2471966373664));
#35152=CARTESIAN_POINT('Ctrl Pts',(-81.425,-1.97002786073214,-11.3045768591928));
#35153=CARTESIAN_POINT('Ctrl Pts',(-81.425,-1.69898895910337,-11.3622311017012));
#35154=CARTESIAN_POINT('Ctrl Pts',(-81.425,-1.42616643671568,-11.4099725343039));
#35155=CARTESIAN_POINT('Ctrl Pts',(-81.425,-1.1520822812381,-11.4476357971411));
#35156=CARTESIAN_POINT('Ctrl Pts',(-81.425,-1.08712517140243,-11.4565618756903));
#35157=CARTESIAN_POINT('Ctrl Pts',(-81.425,-1.02209711150722,-11.464921674965));
#35158=CARTESIAN_POINT('Ctrl Pts',(-81.425,-0.957004902337799,-11.4727125904994));
#35159=CARTESIAN_POINT('Ctrl Pts',(-81.425,-0.683681187122471,-11.5054268278247));
#35160=CARTESIAN_POINT('Ctrl Pts',(-81.425,-0.409227175555571,-11.528114738695));
#35161=CARTESIAN_POINT('Ctrl Pts',(-81.425,-0.134171561186469,-11.5409041668509));
#35162=CARTESIAN_POINT('Ctrl Pts',(-81.425,0.14205800605394,-11.5537481810073));
#35163=CARTESIAN_POINT('Ctrl Pts',(-81.425,0.418894944292535,-11.5566090229993));
#35164=CARTESIAN_POINT('Ctrl Pts',(-81.425,0.695808344418892,-11.5495636793336));
#35165=CARTESIAN_POINT('Ctrl Pts',(-81.425,0.868850798209164,-11.5451610626486));
#35166=CARTESIAN_POINT('Ctrl Pts',(-81.425,1.04192316773346,-11.5368890730119));
#35167=CARTESIAN_POINT('Ctrl Pts',(-81.425,1.21489514481341,-11.5247561922664));
#35168=CARTESIAN_POINT('Ctrl Pts',(-81.425,1.29057038478588,-11.5194480569403));
#35169=CARTESIAN_POINT('Ctrl Pts',(-81.425,1.36622639396203,-11.5134008212102));
#35170=CARTESIAN_POINT('Ctrl Pts',(-81.425,1.44185216969932,-11.5066147218566));
#35171=CARTESIAN_POINT('Ctrl Pts',(-81.425,1.48980074839904,-11.5023121700381));
#35172=CARTESIAN_POINT('Ctrl Pts',(-81.425,1.53773717238975,-11.4977125990324));
#35173=CARTESIAN_POINT('Ctrl Pts',(-81.425,1.58565862201697,-11.492816009391));
#35174=CARTESIAN_POINT('Ctrl Pts',(-81.425,1.61406535643,-11.4899134235436));
#35175=CARTESIAN_POINT('Ctrl Pts',(-81.425,1.64246436467114,-11.4869066940838));
#35176=CARTESIAN_POINT('Ctrl Pts',(-81.425,1.67084421139455,-11.4837971366815));
#35177=CARTESIAN_POINT('Ctrl Pts',(-81.425,1.94835285038083,-11.4533907341748));
#35178=CARTESIAN_POINT('Ctrl Pts',(-81.425,2.22432291238045,-11.4131268975024));
#35179=CARTESIAN_POINT('Ctrl Pts',(-81.425,2.49821721852931,-11.363180987543));
#35180=CARTESIAN_POINT('Ctrl Pts',(-81.425,2.77362818031292,-11.3129585083229));
#35181=CARTESIAN_POINT('Ctrl Pts',(-81.425,3.04694096391893,-11.2529464026702));
#35182=CARTESIAN_POINT('Ctrl Pts',(-81.425,3.31761483196776,-11.1832702047752));
#35183=CARTESIAN_POINT('Ctrl Pts',(-81.425,3.58778884299265,-11.1137226788394));
#35184=CARTESIAN_POINT('Ctrl Pts',(-81.425,3.8553343105734,-11.0345466372617));
#35185=CARTESIAN_POINT('Ctrl Pts',(-81.425,4.11970937111498,-10.945815455283));
#35186=CARTESIAN_POINT('Ctrl Pts',(-81.425,4.32979306970644,-10.8753058737351));
#35187=CARTESIAN_POINT('Ctrl Pts',(-81.425,4.53787483073322,-10.7987616258001));
#35188=CARTESIAN_POINT('Ctrl Pts',(-81.425,4.74367687130894,-10.71619678164));
#35189=CARTESIAN_POINT('Ctrl Pts',(-81.425,4.97202059158535,-10.6245885370044));
#35190=CARTESIAN_POINT('Ctrl Pts',(-81.425,5.1975582746143,-10.52556888611));
#35191=CARTESIAN_POINT('Ctrl Pts',(-81.425,5.42000198252274,-10.4193513770082));
#35192=CARTESIAN_POINT('Ctrl Pts',(-81.425,5.51732110473269,-10.3728812167762));
#35193=CARTESIAN_POINT('Ctrl Pts',(-81.425,5.61404783494252,-10.3250329800772));
#35194=CARTESIAN_POINT('Ctrl Pts',(-81.425,5.71015710130799,-10.2758229214779));
#35195=CARTESIAN_POINT('Ctrl Pts',(-81.425,5.76721628348422,-10.2466073650107));
#35196=CARTESIAN_POINT('Ctrl Pts',(-81.425,5.82405781705297,-10.2169117906126));
#35197=CARTESIAN_POINT('Ctrl Pts',(-81.425,5.88067634387593,-10.1867394433756));
#35198=CARTESIAN_POINT('Ctrl Pts',(-81.425,5.91315078310045,-10.1694336229738));
#35199=CARTESIAN_POINT('Ctrl Pts',(-81.425,5.94555452822165,-10.1519694406033));
#35200=CARTESIAN_POINT('Ctrl Pts',(-81.425,5.97786469226987,-10.1343595761495));
#35201=CARTESIAN_POINT('Ctrl Pts',(-81.425,6.22266283943227,-10.0009383349686));
#35202=CARTESIAN_POINT('Ctrl Pts',(-81.425,6.46234527253621,-9.85902466517761));
#35203=CARTESIAN_POINT('Ctrl Pts',(-81.425,6.69654600256747,-9.70903679572445));
#35204=CARTESIAN_POINT('Ctrl Pts',(-81.425,6.93345436614612,-9.55731489159525));
#35205=CARTESIAN_POINT('Ctrl Pts',(-81.425,7.16475406529005,-9.39733075575456));
#35206=CARTESIAN_POINT('Ctrl Pts',(-81.425,7.39005086306915,-9.22946633224029));
#35207=CARTESIAN_POINT('Ctrl Pts',(-81.425,7.61673670522224,-9.0605669577841));
#35208=CARTESIAN_POINT('Ctrl Pts',(-81.425,7.83734593604377,-8.88368951375276));
#35209=CARTESIAN_POINT('Ctrl Pts',(-81.425,8.05145347150729,-8.69917614679468));
#35210=CARTESIAN_POINT('Ctrl Pts',(-81.425,8.26486801649614,-8.51525998443976));
#35211=CARTESIAN_POINT('Ctrl Pts',(-81.425,8.47182339046597,-8.32375687389967));
#35212=CARTESIAN_POINT('Ctrl Pts',(-81.425,8.67186756704869,-8.12496445217349));
#35213=CARTESIAN_POINT('Ctrl Pts',(-81.425,8.86927294001326,-7.92879432203648));
#35214=CARTESIAN_POINT('Ctrl Pts',(-81.425,9.05994867105627,-7.72552551270578));
#35215=CARTESIAN_POINT('Ctrl Pts',(-81.425,9.24342328678313,-7.51540975236948));
#35216=CARTESIAN_POINT('Ctrl Pts',(-81.425,9.31800737273546,-7.42999580087118));
#35217=CARTESIAN_POINT('Ctrl Pts',(-81.425,9.39140101136385,-7.34345002965296));
#35218=CARTESIAN_POINT('Ctrl Pts',(-81.425,9.46357049537284,-7.25578792958482));
#35219=CARTESIAN_POINT('',(-81.425,-11.925,-1.46039130798322E-15));
#35220=CARTESIAN_POINT('Origin',(-81.425,0.,0.));
#35221=CARTESIAN_POINT('',(-81.425,11.5970184578307,2.77968392481168));
#35222=CARTESIAN_POINT('Origin',(-81.425,0.,0.));
#35223=CARTESIAN_POINT('Ctrl Pts',(-81.425,11.5970184578306,2.77968392481176));
#35224=CARTESIAN_POINT('Ctrl Pts',(-81.425,11.5217985042993,3.05261604105638));
#35225=CARTESIAN_POINT('Ctrl Pts',(-81.425,11.4369053700675,3.3225041885107));
#35226=CARTESIAN_POINT('Ctrl Pts',(-81.425,11.3423804739584,3.58881439697669));
#35227=CARTESIAN_POINT('Ctrl Pts',(-81.425,11.3337495693404,3.61313072106369));
#35228=CARTESIAN_POINT('Ctrl Pts',(-81.425,11.3250383282922,3.63741720505413));
#35229=CARTESIAN_POINT('Ctrl Pts',(-81.425,11.3162467616178,3.66167343587083));
#35230=CARTESIAN_POINT('Ctrl Pts',(-81.425,11.2197848936528,3.92781500324165));
#35231=CARTESIAN_POINT('Ctrl Pts',(-81.425,11.113656826452,4.19031635327416));
#35232=CARTESIAN_POINT('Ctrl Pts',(-81.425,10.9981939856909,4.44873106452655));
#35233=CARTESIAN_POINT('Ctrl Pts',(-81.425,10.882655142131,4.70731587588362));
#35234=CARTESIAN_POINT('Ctrl Pts',(-81.425,10.7577688595731,4.9618091896813));
#35235=CARTESIAN_POINT('Ctrl Pts',(-81.425,10.6238227842739,5.21173643838379));
#35236=CARTESIAN_POINT('Ctrl Pts',(-81.425,10.5801769878256,5.29317423937485));
#35237=CARTESIAN_POINT('Ctrl Pts',(-81.425,10.5355689345581,5.37412698664962));
#35238=CARTESIAN_POINT('Ctrl Pts',(-81.425,10.490007659337,5.45457749292015));
#35239=CARTESIAN_POINT('Ctrl Pts',(-81.425,10.4587925795726,5.50969598901436));
#35240=CARTESIAN_POINT('Ctrl Pts',(-81.425,10.4271300544444,5.56457872818468));
#35241=CARTESIAN_POINT('Ctrl Pts',(-81.425,10.3950228757915,5.61922006877392));
#35242=CARTESIAN_POINT('Ctrl Pts',(-81.425,10.3758763329037,5.65180445690571));
#35243=CARTESIAN_POINT('Ctrl Pts',(-81.425,10.3565762277333,5.68429520631596));
#35244=CARTESIAN_POINT('Ctrl Pts',(-81.425,10.3371255444104,5.71668767315294));
#35245=CARTESIAN_POINT('Ctrl Pts',(-81.425,10.1920782333509,5.95824423624583));
#35246=CARTESIAN_POINT('Ctrl Pts',(-81.425,10.0386228839365,6.19440246598055));
#35247=CARTESIAN_POINT('Ctrl Pts',(-81.425,9.87708819968873,6.42472561727724));
#35248=CARTESIAN_POINT('Ctrl Pts',(-81.425,9.71585158140852,6.65462377320365));
#35249=CARTESIAN_POINT('Ctrl Pts',(-81.425,9.54656502423558,6.87870885973711));
#35250=CARTESIAN_POINT('Ctrl Pts',(-81.425,9.36951408979584,7.09651568591001));
#35251=CARTESIAN_POINT('Ctrl Pts',(-81.425,9.19379661890504,7.3126820945142));
#35252=CARTESIAN_POINT('Ctrl Pts',(-81.425,9.01043088264205,7.52266490201881));
#35253=CARTESIAN_POINT('Ctrl Pts',(-81.425,8.81966127669493,7.72597196868344));
#35254=CARTESIAN_POINT('Ctrl Pts',(-81.425,8.75720458209991,7.79253334416378));
#35255=CARTESIAN_POINT('Ctrl Pts',(-81.425,8.69395404007734,7.85837884269289));
#35256=CARTESIAN_POINT('Ctrl Pts',(-81.425,8.62991751890671,7.92349018984214));
#35257=CARTESIAN_POINT('Ctrl Pts',(-81.425,8.59909107785625,7.95483403969408));
#35258=CARTESIAN_POINT('Ctrl Pts',(-81.425,8.56808249318198,7.98600775332298));
#35259=CARTESIAN_POINT('Ctrl Pts',(-81.425,8.5368926161356,8.01700924783947));
#35260=CARTESIAN_POINT('Ctrl Pts',(-81.425,8.51322858239342,8.04053035410114));
#35261=CARTESIAN_POINT('Ctrl Pts',(-81.425,8.48945955094811,8.06395289139918));
#35262=CARTESIAN_POINT('Ctrl Pts',(-81.425,8.46559774965978,8.08726451773069));
#35263=CARTESIAN_POINT('Ctrl Pts',(-81.425,8.32491115744231,8.22470733807765));
#35264=CARTESIAN_POINT('Ctrl Pts',(-81.425,8.18090552595728,8.35839051249524));
#35265=CARTESIAN_POINT('Ctrl Pts',(-81.425,8.03369044282327,8.48816827575853));
#35266=CARTESIAN_POINT('Ctrl Pts',(-81.425,7.82571847091705,8.67150640090755));
#35267=CARTESIAN_POINT('Ctrl Pts',(-81.425,7.61134266473933,8.84705219851411));
#35268=CARTESIAN_POINT('Ctrl Pts',(-81.425,7.39107933880561,9.01461840461428));
#35269=CARTESIAN_POINT('Ctrl Pts',(-81.425,7.16933642874079,9.18331021025947));
#35270=CARTESIAN_POINT('Ctrl Pts',(-81.425,6.94162608609123,9.34391517153392));
#35271=CARTESIAN_POINT('Ctrl Pts',(-81.425,6.70844294298095,9.49620001683205));
#35272=CARTESIAN_POINT('Ctrl Pts',(-81.425,6.47531259544572,9.64845038293982));
#35273=CARTESIAN_POINT('Ctrl Pts',(-81.425,6.23671134404916,9.79238467087765));
#35274=CARTESIAN_POINT('Ctrl Pts',(-81.425,5.99311001119096,9.92772342358337));
#35275=CARTESIAN_POINT('Ctrl Pts',(-81.425,5.7535262708949,10.0608301032546));
#35276=CARTESIAN_POINT('Ctrl Pts',(-81.425,5.50910543535088,10.1856225652663));
#35277=CARTESIAN_POINT('Ctrl Pts',(-81.425,5.26028139661988,10.3017873386497));
#35278=CARTESIAN_POINT('Ctrl Pts',(-81.425,5.16697238209576,10.3453491286685));
#35279=CARTESIAN_POINT('Ctrl Pts',(-81.425,5.07304406823687,10.3876971542603));
#35280=CARTESIAN_POINT('Ctrl Pts',(-81.425,4.97851906691336,10.4288130563816));
#35281=CARTESIAN_POINT('Ctrl Pts',(-81.425,4.91387906031031,10.456929767806));
#35282=CARTESIAN_POINT('Ctrl Pts',(-81.425,4.84896001780061,10.4844702710005));
#35283=CARTESIAN_POINT('Ctrl Pts',(-81.425,4.78376915312182,10.5114284151287));
#35284=CARTESIAN_POINT('Ctrl Pts',(-81.425,4.75705838983725,10.5224740211342));
#35285=CARTESIAN_POINT('Ctrl Pts',(-81.425,4.73030228286874,10.5334217009663));
#35286=CARTESIAN_POINT('Ctrl Pts',(-81.425,4.70351414680798,10.5442659500702));
#35287=CARTESIAN_POINT('Ctrl Pts',(-81.425,4.44714165051129,10.6480494759911));
#35288=CARTESIAN_POINT('Ctrl Pts',(-81.425,4.18753935832216,10.7424874791396));
#35289=CARTESIAN_POINT('Ctrl Pts',(-81.425,3.92519186134608,10.8273725124873));
#35290=CARTESIAN_POINT('Ctrl Pts',(-81.425,3.66337816313301,10.9120848301571));
#35291=CARTESIAN_POINT('Ctrl Pts',(-81.425,3.39882983789161,10.9872832448377));
#35292=CARTESIAN_POINT('Ctrl Pts',(-81.425,3.13200923994814,11.0527136217828));
#35293=CARTESIAN_POINT('Ctrl Pts',(-81.425,3.06437294932055,11.0692995526482));
#35294=CARTESIAN_POINT('Ctrl Pts',(-81.425,2.99659057691665,11.0852575675369));
#35295=CARTESIAN_POINT('Ctrl Pts',(-81.425,2.92866952489536,11.1005830083263));
#35296=CARTESIAN_POINT('Ctrl Pts',(-81.425,2.65985117950432,11.1612381294237));
#35297=CARTESIAN_POINT('Ctrl Pts',(-81.425,2.38886085810285,11.211988549086));
#35298=CARTESIAN_POINT('Ctrl Pts',(-81.425,2.11624750393544,11.2528573135585));
#35299=CARTESIAN_POINT('Ctrl Pts',(-81.425,1.84398138595298,11.293674022203));
#35300=CARTESIAN_POINT('Ctrl Pts',(-81.425,1.57009572128014,11.3246341879216));
#35301=CARTESIAN_POINT('Ctrl Pts',(-81.425,1.29513858687471,11.3457089466435));
#35302=CARTESIAN_POINT('Ctrl Pts',(-81.425,1.12731412368966,11.358572261054));
#35303=CARTESIAN_POINT('Ctrl Pts',(-81.425,0.959090553024955,11.3677517951114));
#35304=CARTESIAN_POINT('Ctrl Pts',(-81.425,0.790594291629415,11.3732315749573));
#35305=CARTESIAN_POINT('Ctrl Pts',(-81.425,0.716877177268866,11.3756289786399));
#35306=CARTESIAN_POINT('Ctrl Pts',(-81.425,0.643107892631068,11.3773181344974));
#35307=CARTESIAN_POINT('Ctrl Pts',(-81.425,0.569297156125015,11.3782972772602));
#35308=CARTESIAN_POINT('Ctrl Pts',(-81.425,0.521054888586819,11.3789372392679));
#35309=CARTESIAN_POINT('Ctrl Pts',(-81.425,0.472794915191581,11.3792738887815));
#35310=CARTESIAN_POINT('Ctrl Pts',(-81.425,0.424520251078811,11.3793066729465));
#35311=CARTESIAN_POINT('Ctrl Pts',(-81.425,0.39874870013549,11.3793241748554));
#35312=CARTESIAN_POINT('Ctrl Pts',(-81.425,0.372975281400623,11.3792550536749));
#35313=CARTESIAN_POINT('Ctrl Pts',(-81.425,0.347209175026665,11.3790993778194));
#35314=CARTESIAN_POINT('Ctrl Pts',(-81.425,0.0734815860316532,11.3774455471641));
#35315=CARTESIAN_POINT('Ctrl Pts',(-81.425,-0.199703083913748,11.3660280134118));
#35316=CARTESIAN_POINT('Ctrl Pts',(-81.425,-0.471811801903946,11.3449168432811));
#35317=CARTESIAN_POINT('Ctrl Pts',(-81.425,-0.744128229367082,11.3237895583046));
#35318=CARTESIAN_POINT('Ctrl Pts',(-81.425,-1.01536770403303,11.2929537790733));
#35319=CARTESIAN_POINT('Ctrl Pts',(-81.425,-1.28499555980274,11.252427519917));
#35320=CARTESIAN_POINT('Ctrl Pts',(-81.425,-1.55216598200515,11.2122706238938));
#35321=CARTESIAN_POINT('Ctrl Pts',(-81.425,-1.81775462924585,11.162598960697));
#35322=CARTESIAN_POINT('Ctrl Pts',(-81.425,-2.08123166878887,11.103380257873));
#35323=CARTESIAN_POINT('Ctrl Pts',(-81.425,-2.28947413933727,11.0565759936376));
#35324=CARTESIAN_POINT('Ctrl Pts',(-81.425,-2.4963974611547,11.0038069733648));
#35325=CARTESIAN_POINT('Ctrl Pts',(-81.425,-2.70173202408833,10.9450356164872));
#35326=CARTESIAN_POINT('Ctrl Pts',(-81.425,-2.92532867485418,10.8810372405146));
#35327=CARTESIAN_POINT('Ctrl Pts',(-81.425,-3.14704176006627,10.809921422957));
#35328=CARTESIAN_POINT('Ctrl Pts',(-81.425,-3.36656764435611,10.7318318227437));
#35329=CARTESIAN_POINT('Ctrl Pts',(-81.425,-3.46261021873292,10.6976676226504));
#35330=CARTESIAN_POINT('Ctrl Pts',(-81.425,-3.55823395247638,10.6621683008846));
#35331=CARTESIAN_POINT('Ctrl Pts',(-81.425,-3.65341241758583,10.6253445554974));
#35332=CARTESIAN_POINT('Ctrl Pts',(-81.425,-3.71475354916237,10.60161218906));
#35333=CARTESIAN_POINT('Ctrl Pts',(-81.425,-3.77590972035012,10.577329692097));
#35334=CARTESIAN_POINT('Ctrl Pts',(-81.425,-3.83687370523298,10.5524997600722));
#35335=CARTESIAN_POINT('Ctrl Pts',(-81.425,-3.87031237457408,10.53888057346));
#35336=CARTESIAN_POINT('Ctrl Pts',(-81.425,-3.90369614804835,10.5250954090512));
#35337=CARTESIAN_POINT('Ctrl Pts',(-81.425,-3.93700061106458,10.511154572755));
#35338=CARTESIAN_POINT('Ctrl Pts',(-81.425,-4.18507021673326,10.4073157040421));
#35339=CARTESIAN_POINT('Ctrl Pts',(-81.425,-4.42899972961956,10.2947407144357));
#35340=CARTESIAN_POINT('Ctrl Pts',(-81.425,-4.66837293118891,10.1737602696767));
#35341=CARTESIAN_POINT('Ctrl Pts',(-81.425,-4.90946801249104,10.0519095780624));
#35342=CARTESIAN_POINT('Ctrl Pts',(-81.425,-5.14594155284255,9.92153176711564));
#35343=CARTESIAN_POINT('Ctrl Pts',(-81.425,-5.37734790134712,9.78291608734042));
#35344=CARTESIAN_POINT('Ctrl Pts',(-81.425,-5.60826968673858,9.64459066773201));
#35345=CARTESIAN_POINT('Ctrl Pts',(-81.425,-5.83414600053385,9.4980614796471));
#35346=CARTESIAN_POINT('Ctrl Pts',(-81.425,-6.05450572023333,9.34357285602055));
#35347=CARTESIAN_POINT('Ctrl Pts',(-81.425,-6.27316081046619,9.19027930498009));
#35348=CARTESIAN_POINT('Ctrl Pts',(-81.425,-6.48638479737507,9.02914860957272));
#35349=CARTESIAN_POINT('Ctrl Pts',(-81.425,-6.69368220069637,8.8603825530767));
#35350=CARTESIAN_POINT('Ctrl Pts',(-81.425,-6.89733986369601,8.69457970118872));
#35351=CARTESIAN_POINT('Ctrl Pts',(-81.425,-7.09527760205493,8.52140687138442));
#35352=CARTESIAN_POINT('Ctrl Pts',(-81.425,-7.28698538174064,8.34102533285908));
#35353=CARTESIAN_POINT('Ctrl Pts',(-81.425,-7.35124004705837,8.28056688194778));
#35354=CARTESIAN_POINT('Ctrl Pts',(-81.425,-7.41479448322397,8.21929838490928));
#35355=CARTESIAN_POINT('Ctrl Pts',(-81.425,-7.47762833958605,8.15722525234652));
#35356=CARTESIAN_POINT('Ctrl Pts',(-90.4959727487473,-4.76011662834209,
9.98982177454039));
#35357=CARTESIAN_POINT('Ctrl Pts',(-90.4561877805511,-6.42492926884305,
9.19654412535156));
#35358=CARTESIAN_POINT('Ctrl Pts',(-90.3766178441586,-9.3484606603926,6.76207805195742));
#35359=CARTESIAN_POINT('Ctrl Pts',(-90.2572629395698,-11.4459302495084,
1.452207172033));
#35360=CARTESIAN_POINT('Ctrl Pts',(-90.137908034981,-10.7411695159004,-4.21217348791161));
#35361=CARTESIAN_POINT('Ctrl Pts',(-90.0185531303922,-7.40726206096264,
-8.84594083473326));
#35362=CARTESIAN_POINT('Ctrl Pts',(-89.8991982258035,-2.26004805937129,
-11.314084834924));
#35363=CARTESIAN_POINT('Ctrl Pts',(-89.7798433212146,3.44036023950592,-11.0127707789974));
#35364=CARTESIAN_POINT('Ctrl Pts',(-89.6604884166259,8.29862462059312,-8.01559288387814));
#35365=CARTESIAN_POINT('Ctrl Pts',(-89.5411335120371,11.1254633134624,-3.0563078705199));
#35366=CARTESIAN_POINT('Ctrl Pts',(-89.4217786074483,11.2289102651267,2.65114154106624));
#35367=CARTESIAN_POINT('Ctrl Pts',(-89.3024237028595,8.5836358520776,7.70961342848463));
#35368=CARTESIAN_POINT('Ctrl Pts',(-89.1830687982707,3.83717874800117,10.8808559114985));
#35369=CARTESIAN_POINT('Ctrl Pts',(-89.063713893682,-1.84857987243133,11.3885779344766));
#35370=CARTESIAN_POINT('Ctrl Pts',(-88.9443589890932,-7.08182533389115,
9.10849653409288));
#35371=CARTESIAN_POINT('Ctrl Pts',(-88.8250040845044,-10.5815145635538,
4.5987506684781));
#35372=CARTESIAN_POINT('Ctrl Pts',(-88.7056491799156,-11.4909602705537,
-1.03672083502261));
#35373=CARTESIAN_POINT('Ctrl Pts',(-88.5862942753268,-9.58753979769892,
-6.41841405704041));
#35374=CARTESIAN_POINT('Ctrl Pts',(-88.4669393707381,-5.33719041442222,
-10.2289469935215));
#35375=CARTESIAN_POINT('Ctrl Pts',(-88.3475844661493,0.219647037160976,
-11.5355413152965));
#35376=CARTESIAN_POINT('Ctrl Pts',(-88.2282295615605,5.72271720750059,-10.0183564501475));
#35377=CARTESIAN_POINT('Ctrl Pts',(-88.1088746569716,9.82492639772949,-6.0487833070047));
#35378=CARTESIAN_POINT('Ctrl Pts',(-87.989519752383,11.5220969489527,-0.598531631862895));
#35379=CARTESIAN_POINT('Ctrl Pts',(-87.8701648477941,10.3987793606657,4.99823429024215));
#35380=CARTESIAN_POINT('Ctrl Pts',(-87.7508099432054,6.72994996350157,9.37148503193342));
#35381=CARTESIAN_POINT('Ctrl Pts',(-87.6314550386166,1.41369960344878,11.4506948105535));
#35382=CARTESIAN_POINT('Ctrl Pts',(-87.5121001340278,-4.24860954964163,
10.7268949425594));
#35383=CARTESIAN_POINT('Ctrl Pts',(-87.3927452294391,-8.87090377354262,
7.37726402227169));
#35384=CARTESIAN_POINT('Ctrl Pts',(-87.2733903248503,-11.3216940613219,
2.2217564663167));
#35385=CARTESIAN_POINT('Ctrl Pts',(-87.1540354202614,-11.0010527289193,
-3.47761370329691));
#35386=CARTESIAN_POINT('Ctrl Pts',(-87.0346805156727,-7.98746940186916,
-8.32570061724489));
#35387=CARTESIAN_POINT('Ctrl Pts',(-86.9153256110839,-3.01863758058317,
-11.1357435930835));
#35388=CARTESIAN_POINT('Ctrl Pts',(-86.7959707064951,2.68912496921423,-11.2198736674593));
#35389=CARTESIAN_POINT('Ctrl Pts',(-86.6766158019064,7.73861801182051,-8.55749668308028));
#35390=CARTESIAN_POINT('Ctrl Pts',(-86.5572608973175,10.8937787629573,-3.80033452179447));
#35391=CARTESIAN_POINT('Ctrl Pts',(-86.4379059927288,11.3822570579663,1.88710955701514));
#35392=CARTESIAN_POINT('Ctrl Pts',(-86.31855108814,9.08447854823605,7.11260906562713));
#35393=CARTESIAN_POINT('Ctrl Pts',(-86.1991961835512,4.56291524401145,10.5970166881896));
#35394=CARTESIAN_POINT('Ctrl Pts',(-86.0798412789624,-1.07560171741225,
11.4873860890675));
#35395=CARTESIAN_POINT('Ctrl Pts',(-85.9604863743737,-6.45082269201481,
9.56576420418091));
#35396=CARTESIAN_POINT('Ctrl Pts',(-85.8411314697848,-10.2469501238992,
5.30254385857626));
#35397=CARTESIAN_POINT('Ctrl Pts',(-85.7217765651961,-11.5347319468995,
-0.258683449368636));
#35398=CARTESIAN_POINT('Ctrl Pts',(-85.6024216606073,-9.99893271614051,
-5.75658776984223));
#35399=CARTESIAN_POINT('Ctrl Pts',(-85.4830667560185,-6.01549992917226,
-9.84533995430987));
#35400=CARTESIAN_POINT('Ctrl Pts',(-85.3637118514298,-0.559536032933944,
-11.5240564751155));
#35401=CARTESIAN_POINT('Ctrl Pts',(-85.2443569468409,5.03339639874698,-10.3818051853656));
#35402=CARTESIAN_POINT('Ctrl Pts',(-85.1250020422522,9.39420633525482,-6.69819718614323));
#35403=CARTESIAN_POINT('Ctrl Pts',(-85.0056471376634,11.4554133728453,-1.37494097002217));
#35404=CARTESIAN_POINT('Ctrl Pts',(-84.8862922330746,10.7124557092996,4.28488633339115));
#35405=CARTESIAN_POINT('Ctrl Pts',(-84.7669373284858,7.34720156593731,8.89581853250784));
#35406=CARTESIAN_POINT('Ctrl Pts',(-84.647582423897,2.18342975997975,11.3291479245805));
#35407=CARTESIAN_POINT('Ctrl Pts',(-84.5282275193083,-3.5148226850366,10.9892210691436));
#35408=CARTESIAN_POINT('Ctrl Pts',(-84.4088726147195,-8.35268350706726,
7.95924848492489));
#35409=CARTESIAN_POINT('Ctrl Pts',(-84.2895177101306,-11.1458952633209,
2.98093559009735));
#35410=CARTESIAN_POINT('Ctrl Pts',(-84.1701628055419,-11.2107090961286,
-2.72707898253186));
#35411=CARTESIAN_POINT('Ctrl Pts',(-84.0508079009531,-8.53125926061665,
-7.76753330473083));
#35412=CARTESIAN_POINT('Ctrl Pts',(-83.9314529963644,-3.76344689371811,
-10.9065771758865));
#35413=CARTESIAN_POINT('Ctrl Pts',(-83.8120980917756,1.92561768833889,-11.3758056740724));
#35414=CARTESIAN_POINT('Ctrl Pts',(-83.6927431871867,7.1433113126398,-9.06035659838774));
#35415=CARTESIAN_POINT('Ctrl Pts',(-83.573388282598,10.6123974680266,-4.52702752791171));
#35416=CARTESIAN_POINT('Ctrl Pts',(-83.4540333780092,11.4836803397467,1.11447026455969));
#35417=CARTESIAN_POINT('Ctrl Pts',(-83.3346784734204,9.54387907255568,6.48315745825352));
#35418=CARTESIAN_POINT('Ctrl Pts',(-83.2153235688317,5.26783655646332,10.2648358994969));
#35419=CARTESIAN_POINT('Ctrl Pts',(-83.0959686642429,-0.297716860125996,
11.5337904801815));
#35420=CARTESIAN_POINT('Ctrl Pts',(-82.9766137596541,-5.79039248565415,
9.9793944722816));
#35421=CARTESIAN_POINT('Ctrl Pts',(-82.8572588550654,-9.86564059407429,
5.98214765639898));
#35422=CARTESIAN_POINT('Ctrl Pts',(-82.7379039504766,-11.5258843665106,
0.520534034169221));
#35423=CARTESIAN_POINT('Ctrl Pts',(-82.6185490458878,-10.3647114037072,
-5.06850088049748));
#35424=CARTESIAN_POINT('Ctrl Pts',(-82.499194141299,-6.66636917491129,-9.416820017226));
#35425=CARTESIAN_POINT('Ctrl Pts',(-82.3798392367102,-1.33616352515641,
-11.4600008190507));
#35426=CARTESIAN_POINT('Ctrl Pts',(-82.2604843321214,4.32110767959995,-10.6978936382306));
#35427=CARTESIAN_POINT('Ctrl Pts',(-82.1411294275327,8.92064463412699,-7.31705529020618));
#35428=CARTESIAN_POINT('Ctrl Pts',(-82.0217745229439,11.3364445890174,-2.14507737917849));
#35429=CARTESIAN_POINT('Ctrl Pts',(-81.9024196183551,10.9773205983354,3.5519900017792));
#35430=CARTESIAN_POINT('Ctrl Pts',(-81.7830647137664,7.93081818705442,8.37957343457652));
#35431=CARTESIAN_POINT('Ctrl Pts',(-81.6637098091775,2.94344912458979,11.155910191377));
#35432=CARTESIAN_POINT('Ctrl Pts',(-81.5443549045888,-2.76549453716151,
11.2014042094999));
#35433=CARTESIAN_POINT('Ctrl Pts',(-81.4647849681962,-6.11821953149998,
9.40337863342461));
#35434=CARTESIAN_POINT('Ctrl Pts',(-81.425,-7.47762833958605,8.15722525234652));
#35435=CARTESIAN_POINT('Ctrl Pts',(-90.3306484991649,-4.88329262285912,
10.2483251533863));
#35436=CARTESIAN_POINT('Ctrl Pts',(-90.2908635309686,-6.59118508024046,
9.43452011569079));
#35437=CARTESIAN_POINT('Ctrl Pts',(-90.2112935945761,-9.59036774564993,
6.93705815309451));
#35438=CARTESIAN_POINT('Ctrl Pts',(-90.0919386899873,-11.7421128752158,
1.48978546614346));
#35439=CARTESIAN_POINT('Ctrl Pts',(-89.9725837853986,-11.0191152766239,
-4.32117053545506));
#35440=CARTESIAN_POINT('Ctrl Pts',(-89.8532288808097,-7.59893737949893,
-9.07484437740477));
#35441=CARTESIAN_POINT('Ctrl Pts',(-89.733873976221,-2.31853059017985,-11.6068557395893));
#35442=CARTESIAN_POINT('Ctrl Pts',(-89.6145190716322,3.52938532588192,-11.297744677539));
#35443=CARTESIAN_POINT('Ctrl Pts',(-89.4951641670434,8.51336543905939,-8.22300978186688));
#35444=CARTESIAN_POINT('Ctrl Pts',(-89.3758092624546,11.4133533201776,-3.13539495827318));
#35445=CARTESIAN_POINT('Ctrl Pts',(-89.256454357866,11.5194771350673,2.71974427108801));
#35446=CARTESIAN_POINT('Ctrl Pts',(-89.137099453277,8.80575181376569,7.90911259532042));
#35447=CARTESIAN_POINT('Ctrl Pts',(-89.0177445486884,3.93647217825255,11.1624162917873));
#35448=CARTESIAN_POINT('Ctrl Pts',(-88.8983896440995,-1.89641497438559,
11.6832764729245));
#35449=CARTESIAN_POINT('Ctrl Pts',(-88.7790347395108,-7.26507943176433,
9.34419414546267));
#35450=CARTESIAN_POINT('Ctrl Pts',(-88.659679834922,-10.8553289848437,4.71775104837488));
#35451=CARTESIAN_POINT('Ctrl Pts',(-88.5403249303331,-11.7883081235146,
-1.06354772391229));
#35452=CARTESIAN_POINT('Ctrl Pts',(-88.4209700257445,-9.83563345627059,
-6.58450127641458));
#35453=CARTESIAN_POINT('Ctrl Pts',(-88.3016151211555,-5.47529916018465,
-10.4936381381223));
#35454=CARTESIAN_POINT('Ctrl Pts',(-88.1822602165669,0.225330772320723,
-11.8340427774968));
#35455=CARTESIAN_POINT('Ctrl Pts',(-88.062905311978,5.87080210507991,-10.2775982115417));
#35456=CARTESIAN_POINT('Ctrl Pts',(-87.9435504073893,10.0791628323772,-6.20530571131349));
#35457=CARTESIAN_POINT('Ctrl Pts',(-87.8241955028005,11.8202505156445,-0.61401964082588));
#35458=CARTESIAN_POINT('Ctrl Pts',(-87.7048405982117,10.6678652023627,5.12757197828618));
#35459=CARTESIAN_POINT('Ctrl Pts',(-87.5854856936229,6.90409869651127,9.61398791138743));
#35460=CARTESIAN_POINT('Ctrl Pts',(-87.4661307890342,1.45028144969312,11.7470007272621));
#35461=CARTESIAN_POINT('Ctrl Pts',(-87.3467758844453,-4.35854944134002,
11.0044713247771));
#35462=CARTESIAN_POINT('Ctrl Pts',(-87.2274209798567,-9.10045327408744,
7.56816309128768));
#35463=CARTESIAN_POINT('Ctrl Pts',(-87.1080660752678,-11.6146618674713,
2.2792481379879));
#35464=CARTESIAN_POINT('Ctrl Pts',(-86.988711170679,-11.2857234032786,-3.56760278547595));
#35465=CARTESIAN_POINT('Ctrl Pts',(-86.8693562660902,-8.19415855763303,
-8.54114207249709));
#35466=CARTESIAN_POINT('Ctrl Pts',(-86.7500013615015,-3.0967498864584,-11.423899619261));
#35467=CARTESIAN_POINT('Ctrl Pts',(-86.6306464569127,2.75871058409,-11.5102067002922));
#35468=CARTESIAN_POINT('Ctrl Pts',(-86.5112915523239,7.9388677208545,-8.7789362499679));
#35469=CARTESIAN_POINT('Ctrl Pts',(-86.3919366477351,11.1756735436831,-3.89867454595109));
#35470=CARTESIAN_POINT('Ctrl Pts',(-86.2725817431464,11.6767920331423,1.93594167912407));
#35471=CARTESIAN_POINT('Ctrl Pts',(-86.1532268385575,9.31955465397369,7.29665974414477));
#35472=CARTESIAN_POINT('Ctrl Pts',(-86.0338719339688,4.68098832224899,10.8712322529322));
#35473=CARTESIAN_POINT('Ctrl Pts',(-85.9145170293799,-1.10343471428835,
11.7846414540931));
#35474=CARTESIAN_POINT('Ctrl Pts',(-85.7951621247912,-6.61774853912765,
9.81329438277988));
#35475=CARTESIAN_POINT('Ctrl Pts',(-85.6758072202024,-10.5121071296672,
5.43975606664726));
#35476=CARTESIAN_POINT('Ctrl Pts',(-85.5564523156136,-11.8332124653362,
-0.265377317109467));
#35477=CARTESIAN_POINT('Ctrl Pts',(-85.4370974110249,-10.2576718558679,
-5.90554912498069));
#35478=CARTESIAN_POINT('Ctrl Pts',(-85.3177425064361,-6.17116107030506,
-10.1001046239421));
#35479=CARTESIAN_POINT('Ctrl Pts',(-85.1983876018474,-0.574014965427823,
-11.8222607478303));
#35480=CARTESIAN_POINT('Ctrl Pts',(-85.0790326972585,5.16364396527142,-10.6504517918322));
#35481=CARTESIAN_POINT('Ctrl Pts',(-84.9596777926698,9.63729716650747,-6.87152426282912));
#35482=CARTESIAN_POINT('Ctrl Pts',(-84.8403228880808,11.7518413902604,-1.41051987167687));
#35483=CARTESIAN_POINT('Ctrl Pts',(-84.7209679834923,10.9896584521602,4.39576494765983));
#35484=CARTESIAN_POINT('Ctrl Pts',(-84.6016130789033,7.53732271851852,9.12601274419176));
#35485=CARTESIAN_POINT('Ctrl Pts',(-84.4822581743147,2.23992966389856,11.6223086119325));
#35486=CARTESIAN_POINT('Ctrl Pts',(-84.3629032697258,-3.60577461197105,
11.2735855794793));
#35487=CARTESIAN_POINT('Ctrl Pts',(-84.243548365137,-8.56882318981014,8.16520737717167));
#35488=CARTESIAN_POINT('Ctrl Pts',(-84.1241934605483,-11.4343139809775,
3.05807229378971));
#35489=CARTESIAN_POINT('Ctrl Pts',(-84.0048385559595,-11.5008049803207,
-2.7976467211036));
#35490=CARTESIAN_POINT('Ctrl Pts',(-83.8854836513707,-8.7520198902307,-7.96853124542365));
#35491=CARTESIAN_POINT('Ctrl Pts',(-83.766128746782,-3.86083238868385,-11.1888031369938));
#35492=CARTESIAN_POINT('Ctrl Pts',(-83.6467738421931,1.97544627287577,-11.6701737088792));
#35493=CARTESIAN_POINT('Ctrl Pts',(-83.5274189376044,7.32815646324813,-9.29480850825074));
#35494=CARTESIAN_POINT('Ctrl Pts',(-83.4080640330156,10.8870110362217,-4.64417195135637));
#35495=CARTESIAN_POINT('Ctrl Pts',(-83.2887091284268,11.7808398122987,1.14330905022713));
#35496=CARTESIAN_POINT('Ctrl Pts',(-83.169354223838,9.79084293669987,6.65092002162774));
#35497=CARTESIAN_POINT('Ctrl Pts',(-83.0499993192493,5.40415065493143,10.5304557296806));
#35498=CARTESIAN_POINT('Ctrl Pts',(-82.9306444146604,-0.30542078278036,
11.8322466365892));
#35499=CARTESIAN_POINT('Ctrl Pts',(-82.8112895100717,-5.94022859446243,
10.237628027208));
#35500=CARTESIAN_POINT('Ctrl Pts',(-82.6919346054829,-10.1209305767792,
6.13694575158375));
#35501=CARTESIAN_POINT('Ctrl Pts',(-82.5725797008941,-11.8241359389785,
0.534003724587518));
#35502=CARTESIAN_POINT('Ctrl Pts',(-82.4532247963053,-10.6329156799286,
-5.1996568343135));
#35503=CARTESIAN_POINT('Ctrl Pts',(-82.3338698917166,-6.8388726484708,-9.6604960153945));
#35504=CARTESIAN_POINT('Ctrl Pts',(-82.2145149871277,-1.37073899544396,
-11.7565475443237));
#35505=CARTESIAN_POINT('Ctrl Pts',(-82.095160082539,4.43292358189965,-10.9747195630999));
#35506=CARTESIAN_POINT('Ctrl Pts',(-81.9758051779502,9.15148126279261,-7.50639635738527));
#35507=CARTESIAN_POINT('Ctrl Pts',(-81.8564502733615,11.6297940897892,-2.2005848509751));
#35508=CARTESIAN_POINT('Ctrl Pts',(-81.7370953687727,11.2613771640467,3.64390369531744));
#35509=CARTESIAN_POINT('Ctrl Pts',(-81.6177404641838,8.13604139770176,8.59640893925447));
#35510=CARTESIAN_POINT('Ctrl Pts',(-81.4983855595951,3.01961580316925,11.4445880620795));
#35511=CARTESIAN_POINT('Ctrl Pts',(-81.3790306550063,-2.83705634258411,
11.4912593141579));
#35512=CARTESIAN_POINT('Ctrl Pts',(-81.2994607186138,-6.27653871447523,
9.64670681326287));
#35513=CARTESIAN_POINT('Ctrl Pts',(-81.2596757504175,-7.67112450349791,
8.36830712520962));
#35514=CARTESIAN_POINT('Ctrl Pts',(-90.1653242495824,-5.00646861737615,
10.5068285322322));
#35515=CARTESIAN_POINT('Ctrl Pts',(-90.1255392813862,-6.75744089163788,
9.67249610603002));
#35516=CARTESIAN_POINT('Ctrl Pts',(-90.0459693449937,-9.83227483090726,
7.11203825423161));
#35517=CARTESIAN_POINT('Ctrl Pts',(-89.9266144404048,-12.0382955009232,
1.52736376025392));
#35518=CARTESIAN_POINT('Ctrl Pts',(-89.8072595358161,-11.2970610373474,
-4.43016758299852));
#35519=CARTESIAN_POINT('Ctrl Pts',(-89.6879046312272,-7.79061269803522,
-9.30374792007628));
#35520=CARTESIAN_POINT('Ctrl Pts',(-89.5685497266386,-2.37701312098841,
-11.8996266442545));
#35521=CARTESIAN_POINT('Ctrl Pts',(-89.4491948220497,3.61841041225793,-11.5827185760805));
#35522=CARTESIAN_POINT('Ctrl Pts',(-89.329839917461,8.72810625752566,-8.43042667985563));
#35523=CARTESIAN_POINT('Ctrl Pts',(-89.2104850128721,11.7012433268928,-3.21448204602646));
#35524=CARTESIAN_POINT('Ctrl Pts',(-89.0911301082835,11.8100440050079,2.78834700110977));
#35525=CARTESIAN_POINT('Ctrl Pts',(-88.9717752036945,9.02786777545379,8.10861176215623));
#35526=CARTESIAN_POINT('Ctrl Pts',(-88.8524202991058,4.03576560850392,11.4439766720762));
#35527=CARTESIAN_POINT('Ctrl Pts',(-88.7330653945171,-1.94425007633985,
11.9779750113724));
#35528=CARTESIAN_POINT('Ctrl Pts',(-88.6137104899282,-7.44833352963752,
9.57989175683245));
#35529=CARTESIAN_POINT('Ctrl Pts',(-88.4943555853395,-11.1291434061337,
4.83675142827165));
#35530=CARTESIAN_POINT('Ctrl Pts',(-88.3750006807507,-12.0856559764755,
-1.09037461280197));
#35531=CARTESIAN_POINT('Ctrl Pts',(-88.2556457761619,-10.0837271148422,
-6.75058849578874));
#35532=CARTESIAN_POINT('Ctrl Pts',(-88.1362908715731,-5.61340790594708,
-10.7583292827231));
#35533=CARTESIAN_POINT('Ctrl Pts',(-88.0169359669844,0.231014507480469,
-12.1325442396971));
#35534=CARTESIAN_POINT('Ctrl Pts',(-87.8975810623955,6.01888700265922,-10.5368399729359));
#35535=CARTESIAN_POINT('Ctrl Pts',(-87.7782261578068,10.3333992670249,-6.36182811562228));
#35536=CARTESIAN_POINT('Ctrl Pts',(-87.658871253218,12.1184040823362,-0.629507649788865));
#35537=CARTESIAN_POINT('Ctrl Pts',(-87.5395163486293,10.9369510440597,5.25690966633021));
#35538=CARTESIAN_POINT('Ctrl Pts',(-87.4201614440405,7.07824742952097,9.85649079084144));
#35539=CARTESIAN_POINT('Ctrl Pts',(-87.3008065394516,1.48686329593746,12.0433066439708));
#35540=CARTESIAN_POINT('Ctrl Pts',(-87.181451634863,-4.46848933303842,11.2820477069948));
#35541=CARTESIAN_POINT('Ctrl Pts',(-87.0620967302741,-9.33000277463225,
7.75906216030367));
#35542=CARTESIAN_POINT('Ctrl Pts',(-86.9427418256853,-11.9076296736208,
2.33673980965908));
#35543=CARTESIAN_POINT('Ctrl Pts',(-86.8233869210965,-11.5703940776379,
-3.65759186765497));
#35544=CARTESIAN_POINT('Ctrl Pts',(-86.7040320165078,-8.4008477133969,-8.75658352774929));
#35545=CARTESIAN_POINT('Ctrl Pts',(-86.584677111919,-3.17486219233364,-11.7120556454386));
#35546=CARTESIAN_POINT('Ctrl Pts',(-86.4653222073302,2.82829619896576,-11.8005397331251));
#35547=CARTESIAN_POINT('Ctrl Pts',(-86.3459673027414,8.1391174298885,-9.00037581685552));
#35548=CARTESIAN_POINT('Ctrl Pts',(-86.2266123981526,11.4575683244089,-3.9970145701077));
#35549=CARTESIAN_POINT('Ctrl Pts',(-86.1072574935638,11.9713270083183,1.984773801233));
#35550=CARTESIAN_POINT('Ctrl Pts',(-85.9879025889751,9.55463075971132,7.48071042266241));
#35551=CARTESIAN_POINT('Ctrl Pts',(-85.8685476843863,4.79906140048653,11.1454478176748));
#35552=CARTESIAN_POINT('Ctrl Pts',(-85.7491927797975,-1.13126771116443,
12.0818968191186));
#35553=CARTESIAN_POINT('Ctrl Pts',(-85.6298378752088,-6.78467438624051,
10.0608245613788));
#35554=CARTESIAN_POINT('Ctrl Pts',(-85.5104829706199,-10.7772641354352,
5.57696827471827));
#35555=CARTESIAN_POINT('Ctrl Pts',(-85.3911280660311,-12.1316929837729,
-0.272071184850303));
#35556=CARTESIAN_POINT('Ctrl Pts',(-85.2717731614424,-10.5164109955954,
-6.05451048011913));
#35557=CARTESIAN_POINT('Ctrl Pts',(-85.1524182568537,-6.32682221143786,
-10.3548692935743));
#35558=CARTESIAN_POINT('Ctrl Pts',(-85.0330633522648,-0.588493897921702,
-12.1204650205452));
#35559=CARTESIAN_POINT('Ctrl Pts',(-84.913708447676,5.29389153179587,-10.9190983982988));
#35560=CARTESIAN_POINT('Ctrl Pts',(-84.7943535430873,9.88038799776011,-7.044851339515));
#35561=CARTESIAN_POINT('Ctrl Pts',(-84.6749986384985,12.0482694076755,-1.44609877333157));
#35562=CARTESIAN_POINT('Ctrl Pts',(-84.5556437339097,11.2668611950207,4.50664356192851));
#35563=CARTESIAN_POINT('Ctrl Pts',(-84.4362888293209,7.72744387109975,9.35620695587567));
#35564=CARTESIAN_POINT('Ctrl Pts',(-84.3169339247322,2.29642956781735,11.9154692992846));
#35565=CARTESIAN_POINT('Ctrl Pts',(-84.1975790201435,-3.69672653890549,
11.557950089815));
#35566=CARTESIAN_POINT('Ctrl Pts',(-84.0782241155545,-8.78496287255304,
8.37116626941845));
#35567=CARTESIAN_POINT('Ctrl Pts',(-83.9588692109658,-11.7227326986341,
3.13520899748206));
#35568=CARTESIAN_POINT('Ctrl Pts',(-83.839514306377,-11.7909008645129,-2.86821445967534));
#35569=CARTESIAN_POINT('Ctrl Pts',(-83.7201594017883,-8.97278051984475,
-8.16952918611646));
#35570=CARTESIAN_POINT('Ctrl Pts',(-83.6008044971995,-3.9582178836496,-11.4710290981011));
#35571=CARTESIAN_POINT('Ctrl Pts',(-83.4814495926107,2.02527485741264,-11.964541743686));
#35572=CARTESIAN_POINT('Ctrl Pts',(-83.3620946880219,7.51300161385648,-9.52926041811373));
#35573=CARTESIAN_POINT('Ctrl Pts',(-83.2427397834331,11.1616246044169,-4.76131637480104));
#35574=CARTESIAN_POINT('Ctrl Pts',(-83.1233848788443,12.0779992848507,1.17214783589458));
#35575=CARTESIAN_POINT('Ctrl Pts',(-83.0040299742556,10.0378068008441,6.81868258500195));
#35576=CARTESIAN_POINT('Ctrl Pts',(-82.8846750696668,5.54046475339955,10.7960755598643));
#35577=CARTESIAN_POINT('Ctrl Pts',(-82.7653201650779,-0.313124705434724,
12.1307027929969));
#35578=CARTESIAN_POINT('Ctrl Pts',(-82.6459652604893,-6.09006470327072,
10.4958615821344));
#35579=CARTESIAN_POINT('Ctrl Pts',(-82.5266103559004,-10.3762205594841,
6.2917438467685));
#35580=CARTESIAN_POINT('Ctrl Pts',(-82.4072554513117,-12.1223875114463,
0.547473415005821));
#35581=CARTESIAN_POINT('Ctrl Pts',(-82.2879005467229,-10.9011199561499,
-5.33081278812953));
#35582=CARTESIAN_POINT('Ctrl Pts',(-82.1685456421341,-7.01137612203031,
-9.90417201356299));
#35583=CARTESIAN_POINT('Ctrl Pts',(-82.0491907375453,-1.40531446573152,
-12.0530942695968));
#35584=CARTESIAN_POINT('Ctrl Pts',(-81.9298358329565,4.54473948419936,-11.2515454879692));
#35585=CARTESIAN_POINT('Ctrl Pts',(-81.8104809283678,9.38231789145822,-7.69573742456438));
#35586=CARTESIAN_POINT('Ctrl Pts',(-81.6911260237789,11.9231435905609,-2.25609232277172));
#35587=CARTESIAN_POINT('Ctrl Pts',(-81.5717711191902,11.5454337297581,3.73581738885568));
#35588=CARTESIAN_POINT('Ctrl Pts',(-81.4524162146014,8.34126460834911,8.81324444393242));
#35589=CARTESIAN_POINT('Ctrl Pts',(-81.3330613100126,3.0957824817487,11.733265932782));
#35590=CARTESIAN_POINT('Ctrl Pts',(-81.2137064054238,-2.9086181480067,11.7811144188159));
#35591=CARTESIAN_POINT('Ctrl Pts',(-81.1341364690313,-6.43485789745049,
9.89003499310112));
#35592=CARTESIAN_POINT('Ctrl Pts',(-81.0943515008351,-7.86462066740977,
8.57938899807272));
#35593=CARTESIAN_POINT('Ctrl Pts',(-90.,-5.12964461189318,10.765331911078));
#35594=CARTESIAN_POINT('Ctrl Pts',(-89.9602150318037,-6.92369670303529,
9.91047209636926));
#35595=CARTESIAN_POINT('Ctrl Pts',(-89.8806450954113,-10.0741819161646,
7.2870183553687));
#35596=CARTESIAN_POINT('Ctrl Pts',(-89.7612901908224,-12.3344781266306,
1.56494205436438));
#35597=CARTESIAN_POINT('Ctrl Pts',(-89.6419352862337,-11.5750067980709,
-4.53916463054197));
#35598=CARTESIAN_POINT('Ctrl Pts',(-89.5225803816448,-7.98228801657151,
-9.5326514627478));
#35599=CARTESIAN_POINT('Ctrl Pts',(-89.4032254770562,-2.43549565179697,
-12.1923975489198));
#35600=CARTESIAN_POINT('Ctrl Pts',(-89.2838705724673,3.70743549863393,-11.8676924746221));
#35601=CARTESIAN_POINT('Ctrl Pts',(-89.1645156678785,8.94284707599193,-8.63784357784438));
#35602=CARTESIAN_POINT('Ctrl Pts',(-89.0451607632897,11.989133333608,-3.29356913377973));
#35603=CARTESIAN_POINT('Ctrl Pts',(-88.925805858701,12.1006108749485,2.85694973113152));
#35604=CARTESIAN_POINT('Ctrl Pts',(-88.8064509541121,9.24998373714189,8.30811092899203));
#35605=CARTESIAN_POINT('Ctrl Pts',(-88.6870960495233,4.13505903875529,11.7255370523651));
#35606=CARTESIAN_POINT('Ctrl Pts',(-88.5677411449347,-1.9920851782941,12.2726735498203));
#35607=CARTESIAN_POINT('Ctrl Pts',(-88.4483862403458,-7.63158762751069,
9.81558936820223));
#35608=CARTESIAN_POINT('Ctrl Pts',(-88.3290313357571,-11.4029578274237,
4.95575180816843));
#35609=CARTESIAN_POINT('Ctrl Pts',(-88.2096764311682,-12.3830038294364,
-1.11720150169165));
#35610=CARTESIAN_POINT('Ctrl Pts',(-88.0903215265795,-10.3318207734139,
-6.9166757151629));
#35611=CARTESIAN_POINT('Ctrl Pts',(-87.9709666219907,-5.75151665170952,
-11.0230204273238));
#35612=CARTESIAN_POINT('Ctrl Pts',(-87.8516117174019,0.236698242640219,
-12.4310457018974));
#35613=CARTESIAN_POINT('Ctrl Pts',(-87.7322568128131,6.16697190023853,-10.79608173433));
#35614=CARTESIAN_POINT('Ctrl Pts',(-87.6129019082243,10.5876357016726,-6.51835051993107));
#35615=CARTESIAN_POINT('Ctrl Pts',(-87.4935470036357,12.416557649028,-0.644995658751849));
#35616=CARTESIAN_POINT('Ctrl Pts',(-87.3741920990467,11.2060368857567,5.38624735437424));
#35617=CARTESIAN_POINT('Ctrl Pts',(-87.2548371944581,7.25239616253066,10.0989936702955));
#35618=CARTESIAN_POINT('Ctrl Pts',(-87.1354822898692,1.52344514218181,12.3396125606794));
#35619=CARTESIAN_POINT('Ctrl Pts',(-87.0161273852805,-4.57842922473682,
11.5596240892125));
#35620=CARTESIAN_POINT('Ctrl Pts',(-86.8967724806917,-9.55955227517707,
7.94996122931966));
#35621=CARTESIAN_POINT('Ctrl Pts',(-86.7774175761029,-12.2005974797702,
2.39423148133028));
#35622=CARTESIAN_POINT('Ctrl Pts',(-86.6580626715141,-11.8550647519971,
-3.74758094983401));
#35623=CARTESIAN_POINT('Ctrl Pts',(-86.5387077669254,-8.60753686916077,
-8.97202498300148));
#35624=CARTESIAN_POINT('Ctrl Pts',(-86.4193528623365,-3.25297449820887,
-12.0002116716161));
#35625=CARTESIAN_POINT('Ctrl Pts',(-86.2999979577478,2.89788181384153,-12.090872765958));
#35626=CARTESIAN_POINT('Ctrl Pts',(-86.1806430531589,8.3393671389225,-9.22181538374314));
#35627=CARTESIAN_POINT('Ctrl Pts',(-86.0612881485703,11.7394631051347,-4.09535459426431));
#35628=CARTESIAN_POINT('Ctrl Pts',(-85.9419332439813,12.2658619834943,2.03360592334192));
#35629=CARTESIAN_POINT('Ctrl Pts',(-85.8225783393927,9.78970686544896,7.66476110118005));
#35630=CARTESIAN_POINT('Ctrl Pts',(-85.7032234348038,4.91713447872407,11.4196633824174));
#35631=CARTESIAN_POINT('Ctrl Pts',(-85.5838685302151,-1.15910070804053,
12.3791521841442));
#35632=CARTESIAN_POINT('Ctrl Pts',(-85.4645136256264,-6.95160023335335,
10.3083547399778));
#35633=CARTESIAN_POINT('Ctrl Pts',(-85.3451587210375,-11.0424211412032,
5.71418048278927));
#35634=CARTESIAN_POINT('Ctrl Pts',(-85.2258038164488,-12.4301735022096,
-0.278765052591136));
#35635=CARTESIAN_POINT('Ctrl Pts',(-85.1064489118599,-10.7751501353228,
-6.20347183525758));
#35636=CARTESIAN_POINT('Ctrl Pts',(-84.9870940072712,-6.48248335257065,
-10.6096339632065));
#35637=CARTESIAN_POINT('Ctrl Pts',(-84.8677391026824,-0.602972830415581,
-12.4186692932601));
#35638=CARTESIAN_POINT('Ctrl Pts',(-84.7483841980936,5.42413909832031,-11.1877450047655));
#35639=CARTESIAN_POINT('Ctrl Pts',(-84.6290292935049,10.1234788290128,-7.21817841620088));
#35640=CARTESIAN_POINT('Ctrl Pts',(-84.509674388916,12.3446974250905,-1.48167767498628));
#35641=CARTESIAN_POINT('Ctrl Pts',(-84.3903194843273,11.5440639378813,4.6175221761972));
#35642=CARTESIAN_POINT('Ctrl Pts',(-84.2709645797385,7.91756502368096,9.58640116755958));
#35643=CARTESIAN_POINT('Ctrl Pts',(-84.1516096751497,2.35292947173615,12.2086299866367));
#35644=CARTESIAN_POINT('Ctrl Pts',(-84.032254770561,-3.78767846583993,11.8423146001506));
#35645=CARTESIAN_POINT('Ctrl Pts',(-83.9128998659722,-9.00110255529593,
8.57712516166523));
#35646=CARTESIAN_POINT('Ctrl Pts',(-83.7935449613833,-12.0111514162906,
3.21234570117441));
#35647=CARTESIAN_POINT('Ctrl Pts',(-83.6741900567945,-12.0809967487051,
-2.93878219824708));
#35648=CARTESIAN_POINT('Ctrl Pts',(-83.5548351522058,-9.1935411494588,-8.37052712680928));
#35649=CARTESIAN_POINT('Ctrl Pts',(-83.435480247617,-4.05560337861534,-11.7532550592084));
#35650=CARTESIAN_POINT('Ctrl Pts',(-83.3161253430283,2.07510344194952,-12.2589097784928));
#35651=CARTESIAN_POINT('Ctrl Pts',(-83.1967704384394,7.69784676446482,-9.7637123279767));
#35652=CARTESIAN_POINT('Ctrl Pts',(-83.0774155338507,11.4362381726121,-4.87846079824571));
#35653=CARTESIAN_POINT('Ctrl Pts',(-82.9580606292618,12.3751587574026,1.20098662156203));
#35654=CARTESIAN_POINT('Ctrl Pts',(-82.8387057246731,10.2847706649882,6.98644514837616));
#35655=CARTESIAN_POINT('Ctrl Pts',(-82.7193508200843,5.67677885186767,11.0616953900479));
#35656=CARTESIAN_POINT('Ctrl Pts',(-82.5999959154955,-0.320828628089087,
12.4291589494046));
#35657=CARTESIAN_POINT('Ctrl Pts',(-82.4806410109069,-6.23990081207901,
10.7540951370608));
#35658=CARTESIAN_POINT('Ctrl Pts',(-82.361286106318,-10.631510542189,6.44654194195327));
#35659=CARTESIAN_POINT('Ctrl Pts',(-82.2419312017292,-12.4206390839141,
0.560943105424116));
#35660=CARTESIAN_POINT('Ctrl Pts',(-82.1225762971405,-11.1693242323713,
-5.46196874194555));
#35661=CARTESIAN_POINT('Ctrl Pts',(-82.0032213925516,-7.18387959558981,
-10.1478480117315));
#35662=CARTESIAN_POINT('Ctrl Pts',(-81.8838664879629,-1.43988993601907,
-12.3496409948698));
#35663=CARTESIAN_POINT('Ctrl Pts',(-81.764511583374,4.65655538649907,-11.5283714128385));
#35664=CARTESIAN_POINT('Ctrl Pts',(-81.6451566787854,9.61315452012383,-7.88507849174348));
#35665=CARTESIAN_POINT('Ctrl Pts',(-81.5258017741965,12.2164930913327,-2.31159979456833));
#35666=CARTESIAN_POINT('Ctrl Pts',(-81.4064468696078,11.8294902954694,3.82773108239391));
#35667=CARTESIAN_POINT('Ctrl Pts',(-81.287091965019,8.54648781899647,9.03007994861038));
#35668=CARTESIAN_POINT('Ctrl Pts',(-81.1677370604302,3.17194916032815,12.0219438034846));
#35669=CARTESIAN_POINT('Ctrl Pts',(-81.0483821558414,-2.9801799534293,12.0709695234739));
#35670=CARTESIAN_POINT('Ctrl Pts',(-80.9688122194489,-6.59317708042574,
10.1333631729394));
#35671=CARTESIAN_POINT('Ctrl Pts',(-80.9290272512526,-8.05811683132163,
8.79047087093582));
#35672=CARTESIAN_POINT('Ctrl Pts',(-82.2311568471519,-11.9258224962353,
0.000178908662697473));
#35673=CARTESIAN_POINT('Ctrl Pts',(-82.1949633304814,-11.92451531224,-1.80734341106785));
#35674=CARTESIAN_POINT('Ctrl Pts',(-82.1587698138109,-11.5076407664426,
-3.6154480232762));
#35675=CARTESIAN_POINT('Ctrl Pts',(-82.1225762971404,-10.7136359348315,
-5.23912997901492));
#35676=CARTESIAN_POINT('Ctrl Pts',(-82.0827913289442,-9.84084268677745,
-7.02392849854086));
#35677=CARTESIAN_POINT('Ctrl Pts',(-82.0430063607478,-8.51236114118363,
-8.58588825513617));
#35678=CARTESIAN_POINT('Ctrl Pts',(-82.0032213925516,-6.89078875845827,
-9.73383363062355));
#35679=CARTESIAN_POINT('Ctrl Pts',(-81.9634364243553,-5.2692163757329,-10.8817790061109));
#35680=CARTESIAN_POINT('Ctrl Pts',(-81.9236514561591,-3.35455315587599,
-11.6157100004904));
#35681=CARTESIAN_POINT('Ctrl Pts',(-81.8838664879629,-1.38114732552784,
-11.8457972340082));
#35682=CARTESIAN_POINT('Ctrl Pts',(-81.8440815197666,0.592258504820307,
-12.075884467526));
#35683=CARTESIAN_POINT('Ctrl Pts',(-81.8042965515703,2.62440694565969,-11.8021279401822));
#35684=CARTESIAN_POINT('Ctrl Pts',(-81.7645115833741,4.46658102168351,-11.0580341896612));
#35685=CARTESIAN_POINT('Ctrl Pts',(-81.7247266151778,6.30875509770729,-10.3139404391402));
#35686=CARTESIAN_POINT('Ctrl Pts',(-81.6849416469816,7.96095480891553,-9.09950946544184));
#35687=CARTESIAN_POINT('Ctrl Pts',(-81.6451566787853,9.22094442638779,-7.56338086239685));
#35688=CARTESIAN_POINT('Ctrl Pts',(-81.6053717105891,10.4809340438601,-6.02725225935181));
#35689=CARTESIAN_POINT('Ctrl Pts',(-81.5655867423928,11.3487135675964,-4.16942602696006));
#35690=CARTESIAN_POINT('Ctrl Pts',(-81.5258017741965,11.7181028634873,-2.21729109793712));
#35691=CARTESIAN_POINT('Ctrl Pts',(-81.4922011827977,12.0300724178455,-0.568605901509375));
#35692=CARTESIAN_POINT('Ctrl Pts',(-81.4586005913988,11.9865536565682,1.14734714617648));
#35693=CARTESIAN_POINT('Ctrl Pts',(-81.425,11.5970184578307,2.77968392481168));
#35694=CARTESIAN_POINT('Ctrl Pts',(-90.,-6.42475130859185,-9.01043996637154));
#35695=CARTESIAN_POINT('Ctrl Pts',(-89.9663994086011,-5.15589024403101,
-9.91327621792232));
#35696=CARTESIAN_POINT('Ctrl Pts',(-89.8930138490061,-1.9646812879697,-11.2984722410166));
#35697=CARTESIAN_POINT('Ctrl Pts',(-89.7798433212146,3.44036023950592,-11.0127707789974));
#35698=CARTESIAN_POINT('Ctrl Pts',(-89.6604884166259,8.29862462059312,-8.01559288387814));
#35699=CARTESIAN_POINT('Ctrl Pts',(-89.5411335120371,11.1254633134624,-3.0563078705199));
#35700=CARTESIAN_POINT('Ctrl Pts',(-89.4217786074483,11.2289102651267,2.65114154106624));
#35701=CARTESIAN_POINT('Ctrl Pts',(-89.3024237028595,8.5836358520776,7.70961342848463));
#35702=CARTESIAN_POINT('Ctrl Pts',(-89.1830687982707,3.83717874800117,10.8808559114985));
#35703=CARTESIAN_POINT('Ctrl Pts',(-89.063713893682,-1.84857987243133,11.3885779344766));
#35704=CARTESIAN_POINT('Ctrl Pts',(-88.9443589890932,-7.08182533389115,
9.10849653409288));
#35705=CARTESIAN_POINT('Ctrl Pts',(-88.8321642231656,-10.3715670943498,
4.8692917563021));
#35706=CARTESIAN_POINT('Ctrl Pts',(-88.7597544254343,-11.0647130263883,
1.51184016271179));
#35707=CARTESIAN_POINT('Ctrl Pts',(-88.7271295958992,-11.0662550916496,
-0.000269981886922149));
#35708=CARTESIAN_POINT('Origin',(-92.7728704041008,0.,0.));
#35709=CARTESIAN_POINT('Ctrl Pts',(-90.,6.42428395783973,-9.01020671414053));
#35710=CARTESIAN_POINT('Ctrl Pts',(-89.9602150318037,7.92584288148909,-7.93959410657265));
#35711=CARTESIAN_POINT('Ctrl Pts',(-89.8806450954112,10.3816473609839,-5.03396371914769));
#35712=CARTESIAN_POINT('Ctrl Pts',(-89.7612901908224,11.5241044785577,0.559683279179561));
#35713=CARTESIAN_POINT('Ctrl Pts',(-89.6419352862336,9.84536941628095,6.01529970711026));
#35714=CARTESIAN_POINT('Ctrl Pts',(-89.5225803816449,5.75668384652155,9.99893950199032));
#35715=CARTESIAN_POINT('Ctrl Pts',(-89.4032254770561,0.258777053280351,
11.5347028377517));
#35716=CARTESIAN_POINT('Ctrl Pts',(-89.2838705724674,-5.30245378001128,
10.2470084955505));
#35717=CARTESIAN_POINT('Ctrl Pts',(-89.1645156678784,-9.56571023252816,
6.45089830374292));
#35718=CARTESIAN_POINT('Ctrl Pts',(-89.0775156117564,-10.9664491639747,
2.53281638713329));
#35719=CARTESIAN_POINT('Ctrl Pts',(-89.0303005238305,-11.0665694714916,
0.344653378612825));
#35720=CARTESIAN_POINT('Ctrl Pts',(-89.0228704041008,-11.0662155972561,
0.000275354078309552));
#35721=CARTESIAN_POINT('Ctrl Pts',(-90.4959727487473,6.9230012965212,-9.70966930684902));
#35722=CARTESIAN_POINT('Ctrl Pts',(-90.4561877805511,8.54112628032454,-8.55594501338601));
#35723=CARTESIAN_POINT('Ctrl Pts',(-90.3766178441585,11.1875749284727,-5.4247504598192));
#35724=CARTESIAN_POINT('Ctrl Pts',(-90.2572629395698,12.4187210232109,0.603131507391253));
#35725=CARTESIAN_POINT('Ctrl Pts',(-90.137908034981,10.6096657123112,6.48226758726452));
#35726=CARTESIAN_POINT('Ctrl Pts',(-90.0185531303922,6.20357537037213,10.7751574479583));
#35727=CARTESIAN_POINT('Ctrl Pts',(-89.8991982258034,0.278865922977081,
12.4301421333179));
#35728=CARTESIAN_POINT('Ctrl Pts',(-89.7798433212147,-5.71408341142283,
11.0424840442474));
#35729=CARTESIAN_POINT('Ctrl Pts',(-89.6604884166258,-10.3082965785042,
6.95168171482198));
#35730=CARTESIAN_POINT('Ctrl Pts',(-89.5411335120371,-12.3791417069743,
1.15920985029086));
#35731=CARTESIAN_POINT('Ctrl Pts',(-89.4217786074483,-11.4197057842347,
-4.9170383670988));
#35732=CARTESIAN_POINT('Ctrl Pts',(-89.3024237028595,-7.66484473635443,
-9.78964058399421));
#35733=CARTESIAN_POINT('Ctrl Pts',(-89.1830687982707,-2.0337109283889,-12.2658449959716));
#35734=CARTESIAN_POINT('Ctrl Pts',(-89.0637138936819,4.09525421691159,-11.7394980107209));
#35735=CARTESIAN_POINT('Ctrl Pts',(-88.9443589890932,9.22174406413998,-8.33944614371624));
#35736=CARTESIAN_POINT('Ctrl Pts',(-88.8250040845043,12.0908480304004,-2.89798521694021));
#35737=CARTESIAN_POINT('Ctrl Pts',(-88.7056491799157,12.0002395423682,3.25287183483145));
#35738=CARTESIAN_POINT('Ctrl Pts',(-88.5862942753267,8.97209865335899,8.60746016016937));
#35739=CARTESIAN_POINT('Ctrl Pts',(-88.4669393707381,3.74768237847767,11.8550327346267));
#35740=CARTESIAN_POINT('Ctrl Pts',(-88.3475844661492,-2.39412711940671,
12.2006180109483));
#35741=CARTESIAN_POINT('Ctrl Pts',(-88.2282295615605,-7.94987948258836,
9.55962031973835));
#35742=CARTESIAN_POINT('Ctrl Pts',(-88.1088746569717,-11.559584967541,4.57852813059656));
#35743=CARTESIAN_POINT('Ctrl Pts',(-87.9895197523829,-12.3396256411026,
-1.52333958832352));
#35744=CARTESIAN_POINT('Ctrl Pts',(-87.8701648477942,-10.0990557505557,
-7.25230979806363));
#35745=CARTESIAN_POINT('Ctrl Pts',(-87.7508099432053,-5.38634323820261,
-11.2059908523829));
#35746=CARTESIAN_POINT('Ctrl Pts',(-87.6314550386166,0.644889443233899,
-12.4165632148108));
#35747=CARTESIAN_POINT('Ctrl Pts',(-87.5121001340277,6.51825997214534,-10.5876915046587));
#35748=CARTESIAN_POINT('Ctrl Pts',(-87.3927452294391,10.796029021505,-6.16706427960833));
#35749=CARTESIAN_POINT('Ctrl Pts',(-87.2733903248502,12.4310437232692,-0.236804586541372));
#35750=CARTESIAN_POINT('Ctrl Pts',(-87.1540354202615,11.0230696761805,5.75142237852022));
#35751=CARTESIAN_POINT('Ctrl Pts',(-87.0346805156726,6.91676411733848,10.3317616410336));
#35752=CARTESIAN_POINT('Ctrl Pts',(-86.9153256110839,1.11730745581452,12.3829943273524));
#35753=CARTESIAN_POINT('Ctrl Pts',(-86.7959707064951,-4.95565431861441,
11.4030002515323));
#35754=CARTESIAN_POINT('Ctrl Pts',(-86.6766158019064,-9.81552404136514,
7.63167165537372));
#35755=CARTESIAN_POINT('Ctrl Pts',(-86.5572608973175,-12.2726567223273,
1.99219011089958));
#35756=CARTESIAN_POINT('Ctrl Pts',(-86.4379059927288,-11.7255721262879,
-4.13495861808445));
#35757=CARTESIAN_POINT('Ctrl Pts',(-86.31855108814,-8.30819080790685,-9.24991297048049));
#35758=CARTESIAN_POINT('Ctrl Pts',(-86.1991961835512,-2.85705176856468,
-12.100585921921));
#35759=CARTESIAN_POINT('Ctrl Pts',(-86.0798412789625,3.29346349212934,-11.9891627183912));
#35760=CARTESIAN_POINT('Ctrl Pts',(-85.9604863743736,8.63777353189284,-8.94291858812224));
#35761=CARTESIAN_POINT('Ctrl Pts',(-85.8411314697849,11.867647466544,-3.70754205261153));
#35762=CARTESIAN_POINT('Ctrl Pts',(-85.7217765651961,12.192446129963,2.43540177999482));
#35763=CARTESIAN_POINT('Ctrl Pts',(-85.6024216606073,9.53266222570474,7.98218487337101));
#35764=CARTESIAN_POINT('Ctrl Pts',(-85.4830667560185,4.53938287687979,11.575013069502));
#35765=CARTESIAN_POINT('Ctrl Pts',(-85.3637118514297,-1.56508965319305,
12.3343998167531));
#35766=CARTESIAN_POINT('Ctrl Pts',(-85.244356946841,-7.28644469839213,10.0744552269254));
#35767=CARTESIAN_POINT('Ctrl Pts',(-85.1250020422522,-11.224154723112,5.34838996462391));
#35768=CARTESIAN_POINT('Ctrl Pts',(-85.0056471376634,-12.4143097316831,
-0.686904904551077));
#35769=CARTESIAN_POINT('Ctrl Pts',(-84.8862922330746,-10.5655722965231,
-6.55405267822735));
#35770=CARTESIAN_POINT('Ctrl Pts',(-84.7669373284858,-6.13049389601684,
-10.8168372943746));
#35771=CARTESIAN_POINT('Ctrl Pts',(-84.6475824238971,-0.194735072702333,
-12.4317739166017));
#35772=CARTESIAN_POINT('Ctrl Pts',(-84.5282275193082,5.78869284809667,-11.003543046328));
#35773=CARTESIAN_POINT('Ctrl Pts',(-84.4088726147195,10.3551096474539,-6.88176057789721));
#35774=CARTESIAN_POINT('Ctrl Pts',(-84.2895177101307,12.3867045241691,-1.07539550506673));
#35775=CARTESIAN_POINT('Ctrl Pts',(-84.1701628055419,11.3861644217084,4.99421507598957));
#35776=CARTESIAN_POINT('Ctrl Pts',(-84.0508079009532,7.59841103272048,9.84129433752252));
#35777=CARTESIAN_POINT('Ctrl Pts',(-83.9314529963644,1.95064654649944,12.2793282599065));
#35778=CARTESIAN_POINT('Ctrl Pts',(-83.8120980917756,-4.17461569768676,
11.7115117829036));
#35779=CARTESIAN_POINT('Ctrl Pts',(-83.6927431871868,-9.27797592714853,
8.27684040805947));
#35780=CARTESIAN_POINT('Ctrl Pts',(-83.573388282598,-12.1101852435648,2.81608555969103));
#35781=CARTESIAN_POINT('Ctrl Pts',(-83.4540333780092,-11.9779485826422,
-3.33401741156248));
#35782=CARTESIAN_POINT('Ctrl Pts',(-83.3346784734205,-8.91363611698198,
-8.66798799194735));
#35783=CARTESIAN_POINT('Ctrl Pts',(-83.2153235688317,-3.66735924645335,
-11.8801262790221));
#35784=CARTESIAN_POINT('Ctrl Pts',(-83.0959686642429,2.47664850863613,-12.1841346256725));
#35785=CARTESIAN_POINT('Ctrl Pts',(-82.9766137596541,8.01439893416919,-9.50559494678961));
#35786=CARTESIAN_POINT('Ctrl Pts',(-82.8572588550654,11.5903084357114,-4.50018566393989));
#35787=CARTESIAN_POINT('Ctrl Pts',(-82.7379039504766,12.3290330986776,1.60682184985248));
#35788=CARTESIAN_POINT('Ctrl Pts',(-82.6185490458878,10.0497385722665,7.32049603683421));
#35789=CARTESIAN_POINT('Ctrl Pts',(-82.499194141299,5.31037700842289,11.2421902906159));
#35790=CARTESIAN_POINT('Ctrl Pts',(-82.3798392367102,-0.728915757906636,
12.4119135791479));
#35791=CARTESIAN_POINT('Ctrl Pts',(-82.2604843321214,-6.58976355633953,
10.5433331203244));
#35792=CARTESIAN_POINT('Ctrl Pts',(-82.1411294275327,-10.8375357501615,
6.09385116031955));
#35793=CARTESIAN_POINT('Ctrl Pts',(-82.0217745229439,-12.4323325327718,
0.152667783329525));
#35794=CARTESIAN_POINT('Ctrl Pts',(-81.9024196183551,-10.9839510962759,
-5.82590625729596));
#35795=CARTESIAN_POINT('Ctrl Pts',(-81.7830647137663,-6.84655244795005,
-10.3783196702241));
#35796=CARTESIAN_POINT('Ctrl Pts',(-81.6637098091776,-1.03373760445683,
-12.390310166928));
#35797=CARTESIAN_POINT('Ctrl Pts',(-81.5443549045887,5.03323825502514,-11.3690924439751));
#35798=CARTESIAN_POINT('Ctrl Pts',(-81.4647849681962,8.25438701496757,-8.83290032863896));
#35799=CARTESIAN_POINT('Ctrl Pts',(-81.425,9.46357049537284,-7.25578792958482));
#35800=CARTESIAN_POINT('Ctrl Pts',(-90.3306484991649,6.75676218362737,-9.47651510927952));
#35801=CARTESIAN_POINT('Ctrl Pts',(-90.2908635309686,8.33603181404606,-8.35049471111489));
#35802=CARTESIAN_POINT('Ctrl Pts',(-90.2112935945761,10.9189324059764,-5.2944882129287));
#35803=CARTESIAN_POINT('Ctrl Pts',(-90.0919386899874,12.1205155083265,0.588648764654024));
#35804=CARTESIAN_POINT('Ctrl Pts',(-89.9725837853985,10.3549002803011,6.3266116272131));
#35805=CARTESIAN_POINT('Ctrl Pts',(-89.8532288808098,6.0546115290886,10.5164181326357));
#35806=CARTESIAN_POINT('Ctrl Pts',(-89.733873976221,0.272169633078173,12.1316623681291));
#35807=CARTESIAN_POINT('Ctrl Pts',(-89.6145190716323,-5.57687353428564,
10.7773255280151));
#35808=CARTESIAN_POINT('Ctrl Pts',(-89.4951641670433,-10.0607677965122,
6.78475391112896));
#35809=CARTESIAN_POINT('Ctrl Pts',(-89.3758092624547,-12.0818865935326,
1.1313742326279));
#35810=CARTESIAN_POINT('Ctrl Pts',(-89.2564543578658,-11.1454892013152,
-4.79896759674922));
#35811=CARTESIAN_POINT('Ctrl Pts',(-89.1370994532771,-7.48079204954058,
-9.55456606984521));
#35812=CARTESIAN_POINT('Ctrl Pts',(-89.0177445486883,-1.98487628483803,
-11.9713104287099));
#35813=CARTESIAN_POINT('Ctrl Pts',(-88.8983896440995,3.99691660307405,-11.457602391822));
#35814=CARTESIAN_POINT('Ctrl Pts',(-88.7790347395108,9.00030620981994,-8.13919453757342));
#35815=CARTESIAN_POINT('Ctrl Pts',(-88.6596798349219,11.8005155915321,-2.8283971190894));
#35816=CARTESIAN_POINT('Ctrl Pts',(-88.5403249303332,11.712082846942,3.17476199416864));
#35817=CARTESIAN_POINT('Ctrl Pts',(-88.4209700257444,8.75665542909154,8.40077284638618));
#35818=CARTESIAN_POINT('Ctrl Pts',(-88.3016151211556,3.65769086073536,11.570362829087));
#35819=CARTESIAN_POINT('Ctrl Pts',(-88.1822602165668,-2.33663795373441,
11.9076497117923));
#35820=CARTESIAN_POINT('Ctrl Pts',(-88.0629053119781,-7.75898237652218,
9.33006918526815));
#35821=CARTESIAN_POINT('Ctrl Pts',(-87.9435504073892,-11.2820095247355,
4.46858586391342));
#35822=CARTESIAN_POINT('Ctrl Pts',(-87.8241955028005,-12.0433194102992,
-1.48676027669951));
#35823=CARTESIAN_POINT('Ctrl Pts',(-87.7048405982117,-9.85655138039453,
-7.07816313888748));
#35824=CARTESIAN_POINT('Ctrl Pts',(-87.5854856936229,-5.25700324774061,
-10.9369061160659));
#35825=CARTESIAN_POINT('Ctrl Pts',(-87.4661307890341,0.629403984779391,
-12.1184095144703));
#35826=CARTESIAN_POINT('Ctrl Pts',(-87.3467758844454,6.36173974212238,-10.3334537300374));
#35827=CARTESIAN_POINT('Ctrl Pts',(-87.2274209798566,10.5367885258817,-6.01897716376213));
#35828=CARTESIAN_POINT('Ctrl Pts',(-87.1080660752678,12.1325423085809,-0.231118297790334));
#35829=CARTESIAN_POINT('Ctrl Pts',(-86.988711170679,10.7583773489877,5.61331589650015));
#35830=CARTESIAN_POINT('Ctrl Pts',(-86.8693562660902,6.75067477520012,10.0836694023829));
#35831=CARTESIAN_POINT('Ctrl Pts',(-86.7500013615015,1.09047802269313,12.085646702561));
#35832=CARTESIAN_POINT('Ctrl Pts',(-86.6306464569127,-4.83665627969321,
11.1291848115301));
#35833=CARTESIAN_POINT('Ctrl Pts',(-86.5112915523239,-9.57982799866117,
7.44841553977487));
#35834=CARTESIAN_POINT('Ctrl Pts',(-86.3919366477351,-11.9779585879509,
1.94435248924289));
#35835=CARTESIAN_POINT('Ctrl Pts',(-86.2725817431463,-11.4440109037837,
-4.03566759919234));
#35836=CARTESIAN_POINT('Ctrl Pts',(-86.1532268385576,-8.10868972297233,
-9.02779870808241));
#35837=CARTESIAN_POINT('Ctrl Pts',(-86.0338719339688,-2.78844658836103,
-11.8100196511669));
#35838=CARTESIAN_POINT('Ctrl Pts',(-85.91451702938,3.21437894110451,-11.7012720060716));
#35839=CARTESIAN_POINT('Ctrl Pts',(-85.7951621247913,8.43035831588801,-8.72817605246533));
#35840=CARTESIAN_POINT('Ctrl Pts',(-85.6758072202024,11.5826746487625,-3.61851440759975));
#35841=CARTESIAN_POINT('Ctrl Pts',(-85.5564523156137,11.8996740587416,2.37692150329029));
#35842=CARTESIAN_POINT('Ctrl Pts',(-85.4370974110249,9.30375842458687,7.79051203156894));
#35843=CARTESIAN_POINT('Ctrl Pts',(-85.317742506436,4.43038058867899,11.2970671581852));
#35844=CARTESIAN_POINT('Ctrl Pts',(-85.1983876018474,-1.52750781485411,
12.0382190714678));
#35845=CARTESIAN_POINT('Ctrl Pts',(-85.0790326972585,-7.11147837223829,
9.83254157877195));
#35846=CARTESIAN_POINT('Ctrl Pts',(-84.9596777926698,-10.9546338254212,
5.21996133012747));
#35847=CARTESIAN_POINT('Ctrl Pts',(-84.8403228880809,-12.1162101432834,
-0.670410546528588));
#35848=CARTESIAN_POINT('Ctrl Pts',(-84.7209679834922,-10.311865661126,-6.3966729730357));
#35849=CARTESIAN_POINT('Ctrl Pts',(-84.6016130789034,-5.98328492938166,
-10.5570971384632));
#35850=CARTESIAN_POINT('Ctrl Pts',(-84.4822581743146,-0.190058981459703,
-12.1332549680886));
#35851=CARTESIAN_POINT('Ctrl Pts',(-84.3629032697258,5.64969140599582,-10.7393196038696));
#35852=CARTESIAN_POINT('Ctrl Pts',(-84.243548365137,10.1064567629635,-6.71651176100154));
#35853=CARTESIAN_POINT('Ctrl Pts',(-84.1241934605483,12.0892678079849,-1.04957248595764));
#35854=CARTESIAN_POINT('Ctrl Pts',(-84.0048385559594,11.1127532533934,4.8742910938504));
#35855=CARTESIAN_POINT('Ctrl Pts',(-83.8854836513707,7.41595359043792,9.60497948355609));
#35856=CARTESIAN_POINT('Ctrl Pts',(-83.7661287467819,1.90380649294891,11.9844699247096));
#35857=CARTESIAN_POINT('Ctrl Pts',(-83.6467738421932,-4.07437241005299,
11.4302881855003));
#35858=CARTESIAN_POINT('Ctrl Pts',(-83.5274189376044,-9.05518780079726,
8.07809212706594));
#35859=CARTESIAN_POINT('Ctrl Pts',(-83.4080640330156,-11.8193884683451,
2.74846408379857));
#35860=CARTESIAN_POINT('Ctrl Pts',(-83.2887091284268,-11.6903271506389,
-3.25395905635905));
#35861=CARTESIAN_POINT('Ctrl Pts',(-83.169354223838,-8.69959672896538,-8.45984724884512));
#35862=CARTESIAN_POINT('Ctrl Pts',(-83.0499993192493,-3.57929649423348,
-11.5948538127748));
#35863=CARTESIAN_POINT('Ctrl Pts',(-82.9306444146604,2.41717779161743,-11.8915621351014));
#35864=CARTESIAN_POINT('Ctrl Pts',(-82.8112895100718,7.82195254969964,-9.27734110083463));
#35865=CARTESIAN_POINT('Ctrl Pts',(-82.6919346054828,11.3119952432111,-4.39212460189635));
#35866=CARTESIAN_POINT('Ctrl Pts',(-82.5725797008941,12.032981222132,1.56823791386042));
#35867=CARTESIAN_POINT('Ctrl Pts',(-82.4532247963053,9.80841843472616,7.14471205023903));
#35868=CARTESIAN_POINT('Ctrl Pts',(-82.3338698917165,5.18286116302566,10.9722363124425));
#35869=CARTESIAN_POINT('Ctrl Pts',(-82.2145149871278,-0.711412610965203,
12.1138715285492));
#35870=CARTESIAN_POINT('Ctrl Pts',(-82.095160082539,-6.43152634087976,10.2901605048943));
#35871=CARTESIAN_POINT('Ctrl Pts',(-81.9758051779502,-10.5772985709532,
5.94752208025603));
#35872=CARTESIAN_POINT('Ctrl Pts',(-81.8564502733614,-12.1338001704439,
0.149001836180137));
#35873=CARTESIAN_POINT('Ctrl Pts',(-81.7370953687727,-10.7201981070584,
-5.68601122528114));
#35874=CARTESIAN_POINT('Ctrl Pts',(-81.6177404641839,-6.68214906904267,
-10.1291094532373));
#35875=CARTESIAN_POINT('Ctrl Pts',(-81.4983855595951,-1.00891489896113,
-12.0927868699637));
#35876=CARTESIAN_POINT('Ctrl Pts',(-81.3790306550063,4.91237722573152,-11.0960912178675));
#35877=CARTESIAN_POINT('Ctrl Pts',(-81.2994607186138,8.05617789784086,-8.62079961508711));
#35878=CARTESIAN_POINT('Ctrl Pts',(-81.2596757504175,9.23632576486131,-7.08155775150208));
#35879=CARTESIAN_POINT('Ctrl Pts',(-90.1653242495824,6.59052307073355,-9.24336091171003));
#35880=CARTESIAN_POINT('Ctrl Pts',(-90.1255392813862,8.13093734776757,-8.14504440884377));
#35881=CARTESIAN_POINT('Ctrl Pts',(-90.0459693449936,10.6502898834801,-5.16422596603819));
#35882=CARTESIAN_POINT('Ctrl Pts',(-89.9266144404049,11.8223099934421,0.574166021916792));
#35883=CARTESIAN_POINT('Ctrl Pts',(-89.807259535816,10.100134848291,6.17095566716168));
#35884=CARTESIAN_POINT('Ctrl Pts',(-89.6879046312274,5.90564768780508,10.257678817313));
#35885=CARTESIAN_POINT('Ctrl Pts',(-89.5685497266385,0.265473343179258,
11.8331826029404));
#35886=CARTESIAN_POINT('Ctrl Pts',(-89.4491948220497,-5.43966365714846,
10.5121670117828));
#35887=CARTESIAN_POINT('Ctrl Pts',(-89.329839917461,-9.81323901452016,6.61782610743594));
#35888=CARTESIAN_POINT('Ctrl Pts',(-89.2104850128722,-11.7846314800909,
1.10353861496494));
#35889=CARTESIAN_POINT('Ctrl Pts',(-89.0911301082834,-10.8712726183956,
-4.68089682639964));
#35890=CARTESIAN_POINT('Ctrl Pts',(-88.9717752036946,-7.29673936272674,
-9.31949155569622));
#35891=CARTESIAN_POINT('Ctrl Pts',(-88.8524202991058,-1.93604164128715,
-11.6767758614481));
#35892=CARTESIAN_POINT('Ctrl Pts',(-88.7330653945171,3.89857898923652,-11.175706772923));
#35893=CARTESIAN_POINT('Ctrl Pts',(-88.6137104899282,8.7788683554999,-7.9389429314306));
#35894=CARTESIAN_POINT('Ctrl Pts',(-88.4943555853395,11.5101831526637,-2.7588090212386));
#35895=CARTESIAN_POINT('Ctrl Pts',(-88.3750006807507,11.4239261515159,3.09665215350583));
#35896=CARTESIAN_POINT('Ctrl Pts',(-88.2556457761619,8.54121220482409,8.19408553260299));
#35897=CARTESIAN_POINT('Ctrl Pts',(-88.1362908715732,3.56769934299305,11.2856929235474));
#35898=CARTESIAN_POINT('Ctrl Pts',(-88.0169359669843,-2.27914878806212,
11.6146814126363));
#35899=CARTESIAN_POINT('Ctrl Pts',(-87.8975810623956,-7.56808527045601,
9.10051805079796));
#35900=CARTESIAN_POINT('Ctrl Pts',(-87.7782261578068,-11.00443408193,4.35864359723029));
#35901=CARTESIAN_POINT('Ctrl Pts',(-87.658871253218,-11.7470131794959,-1.45018096507549));
#35902=CARTESIAN_POINT('Ctrl Pts',(-87.5395163486293,-9.61404701023339,
-6.90401647971133));
#35903=CARTESIAN_POINT('Ctrl Pts',(-87.4201614440405,-5.12766325727862,
-10.6678213797489));
#35904=CARTESIAN_POINT('Ctrl Pts',(-87.3008065394517,0.613918526324883,
-11.8202558141297));
#35905=CARTESIAN_POINT('Ctrl Pts',(-87.1814516348629,6.20521951209942,-10.0792159554161));
#35906=CARTESIAN_POINT('Ctrl Pts',(-87.0620967302741,10.2775480302584,-5.87089004791594));
#35907=CARTESIAN_POINT('Ctrl Pts',(-86.9427418256853,11.8340408938926,-0.225432009039294));
#35908=CARTESIAN_POINT('Ctrl Pts',(-86.8233869210966,10.4936850217949,5.47520941448009));
#35909=CARTESIAN_POINT('Ctrl Pts',(-86.7040320165078,6.58458543306176,9.83557716373216));
#35910=CARTESIAN_POINT('Ctrl Pts',(-86.584677111919,1.06364858957175,11.7882990777696));
#35911=CARTESIAN_POINT('Ctrl Pts',(-86.4653222073302,-4.71765824077202,
10.8553693715279));
#35912=CARTESIAN_POINT('Ctrl Pts',(-86.3459673027413,-9.3441319559572,7.26515942417602));
#35913=CARTESIAN_POINT('Ctrl Pts',(-86.2266123981528,-11.6832604535745,
1.89651486758619));
#35914=CARTESIAN_POINT('Ctrl Pts',(-86.1072574935638,-11.1624496812795,
-3.93637658030022));
#35915=CARTESIAN_POINT('Ctrl Pts',(-85.9879025889751,-7.90918863803782,
-8.80568444568433));
#35916=CARTESIAN_POINT('Ctrl Pts',(-85.8685476843863,-2.71984140815738,
-11.5194533804129));
#35917=CARTESIAN_POINT('Ctrl Pts',(-85.7491927797975,3.13529439007966,-11.413381293752));
#35918=CARTESIAN_POINT('Ctrl Pts',(-85.6298378752087,8.2229430998832,-8.51343351680839));
#35919=CARTESIAN_POINT('Ctrl Pts',(-85.51048297062,11.2977018309809,-3.52948676258799));
#35920=CARTESIAN_POINT('Ctrl Pts',(-85.3911280660312,11.6069019875202,2.31844122658576));
#35921=CARTESIAN_POINT('Ctrl Pts',(-85.2717731614424,9.07485462346901,7.59883918976686));
#35922=CARTESIAN_POINT('Ctrl Pts',(-85.1524182568537,4.32137830047819,11.0191212468685));
#35923=CARTESIAN_POINT('Ctrl Pts',(-85.0330633522648,-1.48992597651517,
11.7420383261825));
#35924=CARTESIAN_POINT('Ctrl Pts',(-84.9137084476761,-6.93651204608445,
9.59062793061848));
#35925=CARTESIAN_POINT('Ctrl Pts',(-84.7943535430873,-10.6851129277304,
5.09153269563102));
#35926=CARTESIAN_POINT('Ctrl Pts',(-84.6749986384985,-11.8181105548836,
-0.653916188506099));
#35927=CARTESIAN_POINT('Ctrl Pts',(-84.5556437339097,-10.058159025729,-6.23929326784405));
#35928=CARTESIAN_POINT('Ctrl Pts',(-84.436288829321,-5.83607596274649,-10.2973569825517));
#35929=CARTESIAN_POINT('Ctrl Pts',(-84.3169339247321,-0.185382890217079,
-11.8347360195755));
#35930=CARTESIAN_POINT('Ctrl Pts',(-84.1975790201434,5.510689963895,-10.4750961614113));
#35931=CARTESIAN_POINT('Ctrl Pts',(-84.0782241155545,9.85780387847308,-6.55126294410587));
#35932=CARTESIAN_POINT('Ctrl Pts',(-83.9588692109658,11.7918310918008,-1.02374946684855));
#35933=CARTESIAN_POINT('Ctrl Pts',(-83.839514306377,10.8393420850784,4.75436711171122));
#35934=CARTESIAN_POINT('Ctrl Pts',(-83.7201594017883,7.23349614815536,9.36866462958968));
#35935=CARTESIAN_POINT('Ctrl Pts',(-83.6008044971995,1.85696643939838,11.6896115895125));
#35936=CARTESIAN_POINT('Ctrl Pts',(-83.4814495926107,-3.97412912241924,
11.149064588097));
#35937=CARTESIAN_POINT('Ctrl Pts',(-83.3620946880219,-8.83239967444598,
7.87934384607241));
#35938=CARTESIAN_POINT('Ctrl Pts',(-83.2427397834332,-11.5285916931254,
2.68084260790612));
#35939=CARTESIAN_POINT('Ctrl Pts',(-83.1233848788443,-11.4027057186355,
-3.17390070115562));
#35940=CARTESIAN_POINT('Ctrl Pts',(-83.0040299742556,-8.48555734094881,
-8.25170650574289));
#35941=CARTESIAN_POINT('Ctrl Pts',(-82.8846750696667,-3.49123374201361,
-11.3095813465276));
#35942=CARTESIAN_POINT('Ctrl Pts',(-82.765320165078,2.35770707459874,-11.5989896445302));
#35943=CARTESIAN_POINT('Ctrl Pts',(-82.6459652604892,7.6295061652301,-9.04908725487964));
#35944=CARTESIAN_POINT('Ctrl Pts',(-82.5266103559004,11.0336820507108,-4.28406353985282));
#35945=CARTESIAN_POINT('Ctrl Pts',(-82.4072554513116,11.7369293455864,1.52965397786838));
#35946=CARTESIAN_POINT('Ctrl Pts',(-82.2879005467229,9.56709829718583,6.96892806364386));
#35947=CARTESIAN_POINT('Ctrl Pts',(-82.1685456421341,5.05534531762843,10.7022823342691));
#35948=CARTESIAN_POINT('Ctrl Pts',(-82.0491907375453,-0.69390946402377,
11.8158294779506));
#35949=CARTESIAN_POINT('Ctrl Pts',(-81.9298358329566,-6.27328912541999,
10.0369878894641));
#35950=CARTESIAN_POINT('Ctrl Pts',(-81.8104809283677,-10.3170613917449,
5.8011930001925));
#35951=CARTESIAN_POINT('Ctrl Pts',(-81.691126023779,-11.8352678081161,0.145335889030752));
#35952=CARTESIAN_POINT('Ctrl Pts',(-81.5717711191901,-10.4564451178409,
-5.54611619326633));
#35953=CARTESIAN_POINT('Ctrl Pts',(-81.4524162146015,-6.5177456901353,-9.87989923625037));
#35954=CARTESIAN_POINT('Ctrl Pts',(-81.3330613100126,-0.984092193465425,
-11.7952635729993));
#35955=CARTESIAN_POINT('Ctrl Pts',(-81.2137064054239,4.79151619643789,-10.82308999176));
#35956=CARTESIAN_POINT('Ctrl Pts',(-81.1341364690313,7.85796878071416,-8.40869890153527));
#35957=CARTESIAN_POINT('Ctrl Pts',(-81.0943515008351,9.00908103434978,-6.90732757341935));
#35958=CARTESIAN_POINT('Ctrl Pts',(-90.,6.42428395783973,-9.01020671414053));
#35959=CARTESIAN_POINT('Ctrl Pts',(-89.9602150318037,7.92584288148909,-7.93959410657265));
#35960=CARTESIAN_POINT('Ctrl Pts',(-89.8806450954112,10.3816473609839,-5.03396371914769));
#35961=CARTESIAN_POINT('Ctrl Pts',(-89.7612901908224,11.5241044785577,0.559683279179561));
#35962=CARTESIAN_POINT('Ctrl Pts',(-89.6419352862336,9.84536941628095,6.01529970711026));
#35963=CARTESIAN_POINT('Ctrl Pts',(-89.5225803816449,5.75668384652155,9.99893950199032));
#35964=CARTESIAN_POINT('Ctrl Pts',(-89.4032254770561,0.258777053280351,
11.5347028377517));
#35965=CARTESIAN_POINT('Ctrl Pts',(-89.2838705724674,-5.30245378001128,
10.2470084955505));
#35966=CARTESIAN_POINT('Ctrl Pts',(-89.1645156678784,-9.56571023252816,
6.45089830374292));
#35967=CARTESIAN_POINT('Ctrl Pts',(-89.0451607632898,-11.4873763666492,
1.07570299730198));
#35968=CARTESIAN_POINT('Ctrl Pts',(-88.925805858701,-10.5970560354761,-4.56282605605006));
#35969=CARTESIAN_POINT('Ctrl Pts',(-88.8064509541122,-7.11268667591289,
-9.08441704154723));
#35970=CARTESIAN_POINT('Ctrl Pts',(-88.6870960495234,-1.88720699773628,
-11.3822412941864));
#35971=CARTESIAN_POINT('Ctrl Pts',(-88.5677411449346,3.80024137539898,-10.8938111540241));
#35972=CARTESIAN_POINT('Ctrl Pts',(-88.4483862403457,8.55743050117986,-7.73869132528777));
#35973=CARTESIAN_POINT('Ctrl Pts',(-88.3290313357571,11.2198507137954,-2.6892209233878));
#35974=CARTESIAN_POINT('Ctrl Pts',(-88.2096764311682,11.1357694560897,3.01854231284303));
#35975=CARTESIAN_POINT('Ctrl Pts',(-88.0903215265796,8.32576898055664,7.9873982188198));
#35976=CARTESIAN_POINT('Ctrl Pts',(-87.9709666219907,3.47770782525073,11.0010230180077));
#35977=CARTESIAN_POINT('Ctrl Pts',(-87.8516117174019,-2.22165962238982,
11.3217131134804));
#35978=CARTESIAN_POINT('Ctrl Pts',(-87.7322568128132,-7.37718816438983,
8.87096691632776));
#35979=CARTESIAN_POINT('Ctrl Pts',(-87.6129019082243,-10.7268586391246,
4.24870133054717));
#35980=CARTESIAN_POINT('Ctrl Pts',(-87.4935470036356,-11.4507069486926,
-1.41360165345147));
#35981=CARTESIAN_POINT('Ctrl Pts',(-87.3741920990468,-9.37154264007224,
-6.72986982053519));
#35982=CARTESIAN_POINT('Ctrl Pts',(-87.2548371944581,-4.99832326681662,
-10.398736643432));
#35983=CARTESIAN_POINT('Ctrl Pts',(-87.1354822898692,0.598433067870375,
-11.5221021137892));
#35984=CARTESIAN_POINT('Ctrl Pts',(-87.0161273852805,6.04869928207646,-9.82497818079478));
#35985=CARTESIAN_POINT('Ctrl Pts',(-86.8967724806917,10.0183075346351,-5.72280293206974));
#35986=CARTESIAN_POINT('Ctrl Pts',(-86.7774175761028,11.5355394792043,-0.219745720288259));
#35987=CARTESIAN_POINT('Ctrl Pts',(-86.6580626715142,10.2289926946021,5.33710293246003));
#35988=CARTESIAN_POINT('Ctrl Pts',(-86.5387077669253,6.41849609092341,9.58748492508142));
#35989=CARTESIAN_POINT('Ctrl Pts',(-86.4193528623365,1.03681915645036,11.4909514529782));
#35990=CARTESIAN_POINT('Ctrl Pts',(-86.2999979577478,-4.59866020185083,
10.5815539315257));
#35991=CARTESIAN_POINT('Ctrl Pts',(-86.1806430531589,-9.10843591325322,
7.08190330857717));
#35992=CARTESIAN_POINT('Ctrl Pts',(-86.0612881485703,-11.3885623191981,
1.8486772459295));
#35993=CARTESIAN_POINT('Ctrl Pts',(-85.9419332439815,-10.8808884587753,
-3.83708556140811));
#35994=CARTESIAN_POINT('Ctrl Pts',(-85.8225783393926,-7.7096875531033,-8.58357018328625));
#35995=CARTESIAN_POINT('Ctrl Pts',(-85.7032234348039,-2.65123622795373,
-11.2288871096588));
#35996=CARTESIAN_POINT('Ctrl Pts',(-85.583868530215,3.05620983905482,-11.1254905814324));
#35997=CARTESIAN_POINT('Ctrl Pts',(-85.4645136256263,8.01552788387837,-8.29869098115147));
#35998=CARTESIAN_POINT('Ctrl Pts',(-85.3451587210375,11.0127290131994,-3.44045911757623));
#35999=CARTESIAN_POINT('Ctrl Pts',(-85.2258038164487,11.3141299162988,2.25996094988123));
#36000=CARTESIAN_POINT('Ctrl Pts',(-85.10644891186,8.84595082235115,7.40716634796478));
#36001=CARTESIAN_POINT('Ctrl Pts',(-84.9870940072712,4.21237601227739,10.7411753355518));
#36002=CARTESIAN_POINT('Ctrl Pts',(-84.8677391026824,-1.45234413817624,
11.4458575808972));
#36003=CARTESIAN_POINT('Ctrl Pts',(-84.7483841980936,-6.7615457199306,9.34871428246502));
#36004=CARTESIAN_POINT('Ctrl Pts',(-84.6290292935049,-10.4155920300395,
4.96310406113458));
#36005=CARTESIAN_POINT('Ctrl Pts',(-84.509674388916,-11.5200109664838,-0.637421830483606));
#36006=CARTESIAN_POINT('Ctrl Pts',(-84.3903194843273,-9.80445239033203,
-6.08191356265241));
#36007=CARTESIAN_POINT('Ctrl Pts',(-84.2709645797384,-5.68886699611132,
-10.0376168266402));
#36008=CARTESIAN_POINT('Ctrl Pts',(-84.1516096751498,-0.180706798974452,
-11.5362170710623));
#36009=CARTESIAN_POINT('Ctrl Pts',(-84.0322547705609,5.37168852179416,-10.2108727189529));
#36010=CARTESIAN_POINT('Ctrl Pts',(-83.9128998659722,9.60915099398264,-6.38601412721019));
#36011=CARTESIAN_POINT('Ctrl Pts',(-83.7935449613833,11.4943943756167,-0.99792644773947));
#36012=CARTESIAN_POINT('Ctrl Pts',(-83.6741900567946,10.5659309167634,4.63444312957206));
#36013=CARTESIAN_POINT('Ctrl Pts',(-83.5548351522057,7.0510387058728,9.13234977562325));
#36014=CARTESIAN_POINT('Ctrl Pts',(-83.4354802476171,1.81012638584784,11.3947532543155));
#36015=CARTESIAN_POINT('Ctrl Pts',(-83.3161253430282,-3.87388583478548,
10.8678409906937));
#36016=CARTESIAN_POINT('Ctrl Pts',(-83.1967704384395,-8.6096115480947,7.68059556507888));
#36017=CARTESIAN_POINT('Ctrl Pts',(-83.0774155338507,-11.2377949179057,
2.61322113201366));
#36018=CARTESIAN_POINT('Ctrl Pts',(-82.9580606292619,-11.1150842866322,
-3.09384234595218));
#36019=CARTESIAN_POINT('Ctrl Pts',(-82.8387057246731,-8.27151795293221,
-8.04356576264067));
#36020=CARTESIAN_POINT('Ctrl Pts',(-82.7193508200843,-3.40317098979375,
-11.0243088802804));
#36021=CARTESIAN_POINT('Ctrl Pts',(-82.5999959154955,2.29823635758004,-11.306417153959));
#36022=CARTESIAN_POINT('Ctrl Pts',(-82.4806410109068,7.43705978076056,-8.82083340892465));
#36023=CARTESIAN_POINT('Ctrl Pts',(-82.361286106318,10.7553688582105,-4.17600247780928));
#36024=CARTESIAN_POINT('Ctrl Pts',(-82.2419312017292,11.4408774690408,1.49107004187632));
#36025=CARTESIAN_POINT('Ctrl Pts',(-82.1225762971404,9.32577815964549,6.79314407704868));
#36026=CARTESIAN_POINT('Ctrl Pts',(-82.0032213925517,4.92782947223121,10.4323283560957));
#36027=CARTESIAN_POINT('Ctrl Pts',(-81.8838664879629,-0.676406317082347,
11.5177874273519));
#36028=CARTESIAN_POINT('Ctrl Pts',(-81.7645115833741,-6.1150519099602,9.78381527403391));
#36029=CARTESIAN_POINT('Ctrl Pts',(-81.6451566787853,-10.0568242125366,
5.65486392012898));
#36030=CARTESIAN_POINT('Ctrl Pts',(-81.5258017741966,-11.5367354457883,
0.14166994188137));
#36031=CARTESIAN_POINT('Ctrl Pts',(-81.4064468696077,-10.1926921286234,
-5.40622116125151));
#36032=CARTESIAN_POINT('Ctrl Pts',(-81.287091965019,-6.35334231122792,-9.63068901926348));
#36033=CARTESIAN_POINT('Ctrl Pts',(-81.1677370604302,-0.959269487969727,
-11.497740276035));
#36034=CARTESIAN_POINT('Ctrl Pts',(-81.0483821558414,4.67065516714427,-10.5500887656525));
#36035=CARTESIAN_POINT('Ctrl Pts',(-80.9688122194489,7.65975966358745,-8.19659818798342));
#36036=CARTESIAN_POINT('Ctrl Pts',(-80.9290272512526,8.78183630383825,-6.73309739533661));
#36037=CARTESIAN_POINT('Ctrl Pts',(-81.425,9.46357049537263,-7.25578792958508));
#36038=CARTESIAN_POINT('Ctrl Pts',(-81.4647849681962,8.25438701496738,-8.8329003286391));
#36039=CARTESIAN_POINT('Ctrl Pts',(-81.5045699363925,6.64381263499625,-10.1009963863071));
#36040=CARTESIAN_POINT('Ctrl Pts',(-81.5443549045888,4.82736280176375,-10.9052473689665));
#36041=CARTESIAN_POINT('Ctrl Pts',(-81.584139872785,3.01091296853115,-11.7094983516261));
#36042=CARTESIAN_POINT('Ctrl Pts',(-81.6239248409813,0.988587682037159,
-12.049904259277));
#36043=CARTESIAN_POINT('Ctrl Pts',(-81.6637098091776,-0.991377435125372,
-11.8847754636519));
#36044=CARTESIAN_POINT('Ctrl Pts',(-81.7034947773738,-2.97134255228793,
-11.7196466680267));
#36045=CARTESIAN_POINT('Ctrl Pts',(-81.7432797455701,-4.90894750011903,
-11.0489831691254));
#36046=CARTESIAN_POINT('Ctrl Pts',(-81.7830647137663,-6.56731641542222,
-9.95491585085338));
#36047=CARTESIAN_POINT('Ctrl Pts',(-81.8228496819626,-8.22568533072536,
-8.86084853258138));
#36048=CARTESIAN_POINT('Ctrl Pts',(-81.8626346501588,-9.6048182135006,-7.34337739493867));
#36049=CARTESIAN_POINT('Ctrl Pts',(-81.9024196183551,-10.5357815609709,
-5.58821281934641));
#36050=CARTESIAN_POINT('Ctrl Pts',(-81.9412274631861,-11.4438803422434,
-3.87615528629842));
#36051=CARTESIAN_POINT('Ctrl Pts',(-81.9800353080171,-11.9255534427014,
-1.93793649480206));
#36052=CARTESIAN_POINT('Ctrl Pts',(-82.0188431528482,-11.9260172048445,
5.30405712340781E-5));
#36053=CARTESIAN_POINT('Origin',(-85.75,0.,0.));
#36054=CARTESIAN_POINT('Origin',(-81.425,0.,0.));
#36055=CARTESIAN_POINT('Origin',(-94.,-5.,-2.88675134594813));
#36056=CARTESIAN_POINT('',(-89.,-5.,-2.88675134594813));
#36057=CARTESIAN_POINT('',(-94.,-5.,-2.88675134594813));
#36058=CARTESIAN_POINT('',(-89.,-5.,-2.88675134594813));
#36059=CARTESIAN_POINT('Origin',(-94.,-5.,2.88675134594813));
#36060=CARTESIAN_POINT('',(-89.,-5.,2.88675134594813));
#36061=CARTESIAN_POINT('',(-94.,-5.,2.88675134594813));
#36062=CARTESIAN_POINT('',(-89.,-5.,2.88675134594813));
#36063=CARTESIAN_POINT('Origin',(-94.,3.53525079574969E-16,5.77350269189626));
#36064=CARTESIAN_POINT('',(-89.,3.53525079574969E-16,5.77350269189626));
#36065=CARTESIAN_POINT('Origin',(-89.,0.,0.));
#36066=CARTESIAN_POINT('Origin',(-81.25,0.,0.));
#36067=CARTESIAN_POINT('',(-81.,-11.5,-1.40834381901946E-15));
#36068=CARTESIAN_POINT('Origin',(-81.,0.,0.));
#36069=CARTESIAN_POINT('',(-81.25,-11.75,-1.43895998899814E-15));
#36070=CARTESIAN_POINT('Origin',(-81.,0.,0.));
#36071=CARTESIAN_POINT('',(0.,0.,0.));
#36072=CARTESIAN_POINT('Origin',(-27.,-76.,44.));
#36073=CARTESIAN_POINT('',(-45.,-77.5,44.));
#36074=CARTESIAN_POINT('',(-42.,-80.5,44.));
#36075=CARTESIAN_POINT('Origin',(-42.,-77.5,44.));
#36076=CARTESIAN_POINT('',(-45.,-74.5,44.));
#36077=CARTESIAN_POINT('',(-45.,-74.5,44.));
#36078=CARTESIAN_POINT('',(-42.,-71.5,44.));
#36079=CARTESIAN_POINT('Origin',(-42.,-74.5,44.));
#36080=CARTESIAN_POINT('',(-12.,-71.5,44.));
#36081=CARTESIAN_POINT('',(-12.,-71.5,44.));
#36082=CARTESIAN_POINT('',(-9.,-74.5,44.));
#36083=CARTESIAN_POINT('Origin',(-12.,-74.5,44.));
#36084=CARTESIAN_POINT('',(-9.,-77.5,44.));
#36085=CARTESIAN_POINT('',(-9.,-77.5,44.));
#36086=CARTESIAN_POINT('',(-12.,-80.5,44.));
#36087=CARTESIAN_POINT('Origin',(-12.,-77.5,44.));
#36088=CARTESIAN_POINT('',(-42.,-80.5,44.));
#36089=CARTESIAN_POINT('',(-17.,-76.,44.));
#36090=CARTESIAN_POINT('Origin',(-14.,-76.,44.));
#36091=CARTESIAN_POINT('Origin',(-45.,-74.5,44.));
#36092=CARTESIAN_POINT('',(-45.,-77.5,47.));
#36093=CARTESIAN_POINT('',(-45.,-77.5,44.));
#36094=CARTESIAN_POINT('',(-45.,-74.5,47.));
#36095=CARTESIAN_POINT('',(-45.,-74.5,47.));
#36096=CARTESIAN_POINT('',(-45.,-74.5,44.));
#36097=CARTESIAN_POINT('Origin',(-42.,-74.5,44.));
#36098=CARTESIAN_POINT('',(-42.,-71.5,47.));
#36099=CARTESIAN_POINT('Origin',(-42.,-74.5,47.));
#36100=CARTESIAN_POINT('',(-42.,-71.5,44.));
#36101=CARTESIAN_POINT('Origin',(-12.,-71.5,44.));
#36102=CARTESIAN_POINT('',(-12.,-71.5,47.));
#36103=CARTESIAN_POINT('',(-12.,-71.5,47.));
#36104=CARTESIAN_POINT('',(-12.,-71.5,44.));
#36105=CARTESIAN_POINT('Origin',(-12.,-74.5,44.));
#36106=CARTESIAN_POINT('',(-9.,-74.5,47.));
#36107=CARTESIAN_POINT('Origin',(-12.,-74.5,47.));
#36108=CARTESIAN_POINT('',(-9.,-74.5,44.));
#36109=CARTESIAN_POINT('Origin',(-9.,-77.5,44.));
#36110=CARTESIAN_POINT('',(-8.99999999999999,-77.5,47.));
#36111=CARTESIAN_POINT('',(-9.,-77.5,47.));
#36112=CARTESIAN_POINT('',(-9.,-77.5,44.));
#36113=CARTESIAN_POINT('Origin',(-12.,-77.5,44.));
#36114=CARTESIAN_POINT('',(-12.,-80.5,47.));
#36115=CARTESIAN_POINT('Origin',(-12.,-77.5,47.));
#36116=CARTESIAN_POINT('',(-12.,-80.5,44.));
#36117=CARTESIAN_POINT('Origin',(-42.,-80.5,44.));
#36118=CARTESIAN_POINT('',(-42.,-80.5,47.));
#36119=CARTESIAN_POINT('',(-42.,-80.5,47.));
#36120=CARTESIAN_POINT('',(-42.,-80.5,44.));
#36121=CARTESIAN_POINT('Origin',(-42.,-77.5,44.));
#36122=CARTESIAN_POINT('Origin',(-42.,-77.5,47.));
#36123=CARTESIAN_POINT('Origin',(-27.,-76.,47.));
#36124=CARTESIAN_POINT('Origin',(-14.,-76.,38.));
#36125=CARTESIAN_POINT('',(-17.,-76.,38.0829037686548));
#36126=CARTESIAN_POINT('',(-17.,-76.,38.));
#36127=CARTESIAN_POINT('',(-14.,-79.,39.8149545762236));
#36128=CARTESIAN_POINT('Origin',(-14.,-76.,39.8149545762236));
#36129=CARTESIAN_POINT('',(-14.,-73.,39.8149545762236));
#36130=CARTESIAN_POINT('Origin',(-14.,-76.,39.8149545762236));
#36131=CARTESIAN_POINT('Origin',(-14.,-76.,39.8149545762236));
#36132=CARTESIAN_POINT('Origin',(-5.5,-72.,34.9074772881118));
#36133=CARTESIAN_POINT('',(-14.,-95.,39.8149545762236));
#36134=CARTESIAN_POINT('',(-14.,-72.,39.8149545762236));
#36135=CARTESIAN_POINT('',(-12.3117376914899,-95.,38.8402358779426));
#36136=CARTESIAN_POINT('',(-5.5,-95.,34.9074772881118));
#36137=CARTESIAN_POINT('',(-7.1882623085101,-95.,35.8821959863928));
#36138=CARTESIAN_POINT('',(-5.5,-95.,34.9074772881118));
#36139=CARTESIAN_POINT('',(-5.5,-95.,34.9074772881118));
#36140=CARTESIAN_POINT('',(-5.5,-95.,34.9074772881118));
#36141=CARTESIAN_POINT('',(-5.5,-72.,34.9074772881118));
#36142=CARTESIAN_POINT('',(-5.5,-72.,34.9074772881118));
#36143=CARTESIAN_POINT('',(-14.,-72.,39.8149545762236));
#36144=CARTESIAN_POINT('',(-5.5,-72.,34.9074772881118));
#36145=CARTESIAN_POINT('',(-14.,-72.,39.8149545762236));
#36146=CARTESIAN_POINT('Origin',(-8.4,-96.,30.));
#36147=CARTESIAN_POINT('',(-19.6,-96.,30.));
#36148=CARTESIAN_POINT('Origin',(-14.,-96.,30.));
#36149=CARTESIAN_POINT('Origin',(-14.,-100.55,30.));
#36150=CARTESIAN_POINT('',(-19.6,-105.,30.));
#36151=CARTESIAN_POINT('',(-19.6,-100.55,30.));
#36152=CARTESIAN_POINT('Origin',(-14.,-105.,30.));
#36153=CARTESIAN_POINT('Origin',(-5.,-95.,30.));
#36154=CARTESIAN_POINT('',(-12.3117376914899,-95.,21.1597641220574));
#36155=CARTESIAN_POINT('',(-7.18826230851011,-95.,24.1178040136072));
#36156=CARTESIAN_POINT('',(-14.,-95.,20.1850454237764));
#36157=CARTESIAN_POINT('Origin',(-14.,-95.,30.));
#36158=CARTESIAN_POINT('Origin',(-5.,-95.,30.));
#36159=CARTESIAN_POINT('',(-20.8117376914899,-95.,24.1178040136072));
#36160=CARTESIAN_POINT('',(-15.6882623085101,-95.,21.1597641220574));
#36161=CARTESIAN_POINT('',(-22.5,-95.,25.0925227118882));
#36162=CARTESIAN_POINT('Origin',(-14.,-95.,30.));
#36163=CARTESIAN_POINT('Origin',(-5.,-95.,30.));
#36164=CARTESIAN_POINT('',(-5.5,-95.,27.0419601084502));
#36165=CARTESIAN_POINT('',(-5.5,-95.,32.9580398915498));
#36166=CARTESIAN_POINT('',(-5.5,-95.,25.0925227118882));
#36167=CARTESIAN_POINT('Origin',(-14.,-95.,30.));
#36168=CARTESIAN_POINT('Origin',(-5.,-95.,30.));
#36169=CARTESIAN_POINT('',(-22.5,-95.,32.9580398915498));
#36170=CARTESIAN_POINT('',(-22.5,-95.,27.0419601084502));
#36171=CARTESIAN_POINT('',(-22.5,-95.,34.9074772881118));
#36172=CARTESIAN_POINT('',(-23.,-95.,30.));
#36173=CARTESIAN_POINT('Origin',(-14.,-95.,30.));
#36174=CARTESIAN_POINT('Origin',(-14.,-95.,30.));
#36175=CARTESIAN_POINT('Origin',(-5.,-95.,30.));
#36176=CARTESIAN_POINT('Origin',(-14.,-95.,30.));
#36177=CARTESIAN_POINT('Origin',(-5.,-95.,30.));
#36178=CARTESIAN_POINT('',(-15.6882623085101,-95.,38.8402358779426));
#36179=CARTESIAN_POINT('',(-20.8117376914899,-95.,35.8821959863928));
#36180=CARTESIAN_POINT('',(-14.,-95.,39.8149545762236));
#36181=CARTESIAN_POINT('Origin',(-14.,-95.,30.));
#36182=CARTESIAN_POINT('Origin',(-14.,-99.5,30.));
#36183=CARTESIAN_POINT('',(-23.,-104.,30.));
#36184=CARTESIAN_POINT('Origin',(-14.,-104.,30.));
#36185=CARTESIAN_POINT('',(-23.,-99.5,30.));
#36186=CARTESIAN_POINT('Origin',(-14.,-95.,30.));
#36187=CARTESIAN_POINT('Origin',(-14.,-95.,30.));
#36188=CARTESIAN_POINT('Origin',(-14.,-95.,30.));
#36189=CARTESIAN_POINT('Origin',(-14.,-95.,30.));
#36190=CARTESIAN_POINT('Origin',(-14.,-95.,30.));
#36191=CARTESIAN_POINT('Origin',(-14.,-95.,30.));
#36192=CARTESIAN_POINT('Origin',(-14.,-104.5,30.));
#36193=CARTESIAN_POINT('',(-22.,-105.,30.));
#36194=CARTESIAN_POINT('Origin',(-14.,-105.,30.));
#36195=CARTESIAN_POINT('',(-22.5,-104.5,30.));
#36196=CARTESIAN_POINT('Origin',(-14.,-105.,30.));
#36197=CARTESIAN_POINT('Origin',(-14.,-95.,30.));
#36198=CARTESIAN_POINT('',(-5.5,-95.,25.0925227118882));
#36199=CARTESIAN_POINT('',(-14.,-95.,20.1850454237764));
#36200=CARTESIAN_POINT('',(-5.5,-95.,25.0925227118882));
#36201=CARTESIAN_POINT('Origin',(-14.,-95.,30.));
#36202=CARTESIAN_POINT('',(-5.5,-95.,25.0925227118882));
#36203=CARTESIAN_POINT('Origin',(-14.,-95.,30.));
#36204=CARTESIAN_POINT('',(-14.,-95.,20.1850454237764));
#36205=CARTESIAN_POINT('',(-22.5,-95.,25.0925227118882));
#36206=CARTESIAN_POINT('',(-14.,-95.,20.1850454237764));
#36207=CARTESIAN_POINT('Origin',(-14.,-95.,30.));
#36208=CARTESIAN_POINT('',(-14.,-95.,39.8149545762236));
#36209=CARTESIAN_POINT('Origin',(-14.,-95.,30.));
#36210=CARTESIAN_POINT('',(-22.5,-95.,25.0925227118882));
#36211=CARTESIAN_POINT('',(-22.5,-95.,34.9074772881118));
#36212=CARTESIAN_POINT('',(-22.5,-95.,25.0925227118882));
#36213=CARTESIAN_POINT('Origin',(-14.,-72.,30.));
#36214=CARTESIAN_POINT('',(-14.,-72.,20.1850454237764));
#36215=CARTESIAN_POINT('',(-5.5,-72.,25.0925227118882));
#36216=CARTESIAN_POINT('',(-14.,-72.,20.1850454237764));
#36217=CARTESIAN_POINT('',(-22.5,-72.,25.0925227118882));
#36218=CARTESIAN_POINT('',(-22.5,-72.,25.0925227118882));
#36219=CARTESIAN_POINT('',(-22.5,-72.,34.9074772881118));
#36220=CARTESIAN_POINT('',(-22.5,-72.,34.9074772881118));
#36221=CARTESIAN_POINT('',(-14.,-72.,39.8149545762236));
#36222=CARTESIAN_POINT('',(-5.5,-72.,25.0925227118882));
#36223=CARTESIAN_POINT('',(-20.8,-72.,30.));
#36224=CARTESIAN_POINT('Origin',(-14.,-72.,30.));
#36225=CARTESIAN_POINT('Origin',(-22.5,-72.,25.0925227118882));
#36226=CARTESIAN_POINT('',(-14.,-72.,20.1850454237764));
#36227=CARTESIAN_POINT('',(-22.5,-72.,25.0925227118882));
#36228=CARTESIAN_POINT('Origin',(-22.5,-72.,34.9074772881118));
#36229=CARTESIAN_POINT('',(-22.5,-95.,34.9074772881118));
#36230=CARTESIAN_POINT('',(-22.5,-95.,34.9074772881118));
#36231=CARTESIAN_POINT('',(-22.5,-72.,34.9074772881118));
#36232=CARTESIAN_POINT('Origin',(-14.,-72.,39.8149545762236));
#36233=CARTESIAN_POINT('',(-14.,-95.,39.8149545762236));
#36234=CARTESIAN_POINT('Origin',(-5.5,-72.,25.0925227118882));
#36235=CARTESIAN_POINT('',(-5.5,-72.,25.0925227118882));
#36236=CARTESIAN_POINT('Origin',(-14.,-72.,20.1850454237764));
#36237=CARTESIAN_POINT('Origin',(-14.,-95.,30.));
#36238=CARTESIAN_POINT('Origin',(-7.5,-60.5,30.));
#36239=CARTESIAN_POINT('',(-20.5,-60.5,30.));
#36240=CARTESIAN_POINT('Origin',(-14.,-60.5,30.));
#36241=CARTESIAN_POINT('Origin',(-14.,-60.75,30.));
#36242=CARTESIAN_POINT('',(-20.8,-61.,30.));
#36243=CARTESIAN_POINT('Origin',(-14.,-61.,30.));
#36244=CARTESIAN_POINT('',(-20.65,-60.75,30.));
#36245=CARTESIAN_POINT('Origin',(-14.,-66.5,30.));
#36246=CARTESIAN_POINT('',(-20.8,-66.5,30.));
#36247=CARTESIAN_POINT('',(0.,0.,0.));
#36248=CARTESIAN_POINT('Origin',(16.,70.,-17.6076951545867));
#36249=CARTESIAN_POINT('',(15.5669872981078,70.5,-17.2803448853971));
#36250=CARTESIAN_POINT('',(16.4330127018922,70.5,-17.2803448853971));
#36251=CARTESIAN_POINT('',(15.5669872981078,70.5,-17.2803448853971));
#36252=CARTESIAN_POINT('',(16.,70.,-17.6076951545867));
#36253=CARTESIAN_POINT('',(16.,70.,-17.6076951545867));
#36254=CARTESIAN_POINT('',(16.4330127018922,70.5,-17.2803448853971));
#36255=CARTESIAN_POINT('Origin',(7.,70.,-22.8038475772934));
#36256=CARTESIAN_POINT('',(6.5,70.5,-23.0151724426986));
#36257=CARTESIAN_POINT('',(6.93301270189222,70.5,-22.2651724426986));
#36258=CARTESIAN_POINT('',(6.5,70.5,-23.0151724426986));
#36259=CARTESIAN_POINT('',(7.,70.,-22.8038475772934));
#36260=CARTESIAN_POINT('',(7.,70.,-22.8038475772934));
#36261=CARTESIAN_POINT('',(6.93301270189222,70.5,-22.2651724426986));
#36262=CARTESIAN_POINT('Origin',(25.,70.,-22.8038475772934));
#36263=CARTESIAN_POINT('',(25.0669872981078,70.5,-22.2651724426986));
#36264=CARTESIAN_POINT('',(25.5,70.5,-23.0151724426986));
#36265=CARTESIAN_POINT('',(25.0669872981078,70.5,-22.2651724426986));
#36266=CARTESIAN_POINT('',(25.,70.,-22.8038475772934));
#36267=CARTESIAN_POINT('',(25.,70.,-22.8038475772934));
#36268=CARTESIAN_POINT('',(25.5,70.5,-23.0151724426986));
#36269=CARTESIAN_POINT('Origin',(18.25,70.25,-18.6180581256686));
#36270=CARTESIAN_POINT('',(18.125,70.,-18.8345644766147));
#36271=CARTESIAN_POINT('',(18.375,70.5,-18.4015517747225));
#36272=CARTESIAN_POINT('Origin',(7.,70.,-33.1961524227066));
#36273=CARTESIAN_POINT('',(6.93301270189222,70.5,-33.7348275573014));
#36274=CARTESIAN_POINT('',(6.5,70.5,-32.9848275573015));
#36275=CARTESIAN_POINT('',(6.93301270189222,70.5,-33.7348275573015));
#36276=CARTESIAN_POINT('',(7.,70.,-33.1961524227066));
#36277=CARTESIAN_POINT('',(7.,70.,-33.1961524227066));
#36278=CARTESIAN_POINT('',(6.5,70.5,-32.9848275573015));
#36279=CARTESIAN_POINT('Origin',(25.0669872981078,70.5,-33.7348275573015));
#36280=CARTESIAN_POINT('',(25.,70.,-33.1961524227066));
#36281=CARTESIAN_POINT('',(25.5,70.5,-32.9848275573015));
#36282=CARTESIAN_POINT('',(25.,70.,-33.1961524227066));
#36283=CARTESIAN_POINT('',(25.0669872981078,70.5,-33.7348275573015));
#36284=CARTESIAN_POINT('',(25.0669872981078,70.5,-33.7348275573015));
#36285=CARTESIAN_POINT('',(25.5,70.5,-32.9848275573015));
#36286=CARTESIAN_POINT('Origin',(16.,70.,-38.3923048454133));
#36287=CARTESIAN_POINT('',(16.4330127018922,70.5,-38.7196551146029));
#36288=CARTESIAN_POINT('',(15.5669872981078,70.5,-38.7196551146029));
#36289=CARTESIAN_POINT('',(16.4330127018922,70.5,-38.7196551146029));
#36290=CARTESIAN_POINT('',(16.,70.,-38.3923048454133));
#36291=CARTESIAN_POINT('',(16.,70.,-38.3923048454133));
#36292=CARTESIAN_POINT('',(15.5669872981078,70.5,-38.7196551146029));
#36293=CARTESIAN_POINT('Origin',(23.,70.25,-34.6395280956807));
#36294=CARTESIAN_POINT('',(22.875,70.,-34.4230217447346));
#36295=CARTESIAN_POINT('',(23.125,70.5,-34.8560344466268));
#36296=CARTESIAN_POINT('Origin',(13.75,70.25,-37.3819418743314));
#36297=CARTESIAN_POINT('',(13.875,70.,-37.1654355233853));
#36298=CARTESIAN_POINT('',(13.625,70.5,-37.5984482252775));
#36299=CARTESIAN_POINT('Origin',(16.,70.,-38.7196551146029));
#36300=CARTESIAN_POINT('',(15.5669872981078,74.,-38.7196551146029));
#36301=CARTESIAN_POINT('',(16.4330127018922,74.,-38.7196551146029));
#36302=CARTESIAN_POINT('',(16.,74.,-38.7196551146029));
#36303=CARTESIAN_POINT('',(16.4330127018922,70.,-38.7196551146029));
#36304=CARTESIAN_POINT('',(15.5669872981078,70.,-38.7196551146029));
#36305=CARTESIAN_POINT('Origin',(25.2834936490539,70.,-33.3598275573014));
#36306=CARTESIAN_POINT('',(25.0669872981078,74.,-33.7348275573015));
#36307=CARTESIAN_POINT('',(25.5,74.,-32.9848275573015));
#36308=CARTESIAN_POINT('',(25.2834936490539,74.,-33.3598275573014));
#36309=CARTESIAN_POINT('',(25.5,70.,-32.9848275573015));
#36310=CARTESIAN_POINT('',(25.0669872981078,70.,-33.7348275573015));
#36311=CARTESIAN_POINT('Origin',(25.25,70.25,-25.2575862213493));
#36312=CARTESIAN_POINT('',(25.,70.,-25.2575862213493));
#36313=CARTESIAN_POINT('',(25.5,70.5,-25.2575862213493));
#36314=CARTESIAN_POINT('Origin',(6.75,70.25,-30.7424137786507));
#36315=CARTESIAN_POINT('',(7.,70.,-30.7424137786507));
#36316=CARTESIAN_POINT('',(6.5,70.5,-30.7424137786507));
#36317=CARTESIAN_POINT('Origin',(6.71650635094611,70.,-33.3598275573014));
#36318=CARTESIAN_POINT('',(6.5,74.,-32.9848275573015));
#36319=CARTESIAN_POINT('',(6.93301270189222,74.,-33.7348275573014));
#36320=CARTESIAN_POINT('',(6.71650635094611,74.,-33.3598275573015));
#36321=CARTESIAN_POINT('',(6.93301270189222,70.,-33.7348275573015));
#36322=CARTESIAN_POINT('',(6.5,70.,-32.9848275573015));
#36323=CARTESIAN_POINT('Origin',(25.2834936490539,70.,-22.6401724426986));
#36324=CARTESIAN_POINT('',(25.5,74.,-23.0151724426986));
#36325=CARTESIAN_POINT('',(25.0669872981078,74.,-22.2651724426986));
#36326=CARTESIAN_POINT('',(25.2834936490539,74.,-22.6401724426985));
#36327=CARTESIAN_POINT('',(25.0669872981078,70.,-22.2651724426986));
#36328=CARTESIAN_POINT('',(25.5,70.,-23.0151724426986));
#36329=CARTESIAN_POINT('Origin',(9.,70.25,-21.3604719043193));
#36330=CARTESIAN_POINT('',(9.125,70.,-21.5769782552654));
#36331=CARTESIAN_POINT('',(8.875,70.5,-21.1439655533732));
#36332=CARTESIAN_POINT('Origin',(6.71650635094611,70.,-22.6401724426986));
#36333=CARTESIAN_POINT('',(6.93301270189222,74.,-22.2651724426986));
#36334=CARTESIAN_POINT('',(6.5,74.,-23.0151724426986));
#36335=CARTESIAN_POINT('',(6.71650635094611,74.,-22.6401724426985));
#36336=CARTESIAN_POINT('',(6.5,70.,-23.0151724426986));
#36337=CARTESIAN_POINT('',(6.93301270189222,70.,-22.2651724426986));
#36338=CARTESIAN_POINT('Origin',(16.,70.,-17.2803448853971));
#36339=CARTESIAN_POINT('',(16.4330127018922,74.,-17.2803448853971));
#36340=CARTESIAN_POINT('',(15.5669872981078,74.,-17.2803448853971));
#36341=CARTESIAN_POINT('',(16.,74.,-17.2803448853971));
#36342=CARTESIAN_POINT('',(15.5669872981078,70.,-17.2803448853971));
#36343=CARTESIAN_POINT('',(16.4330127018922,70.,-17.2803448853971));
#36344=CARTESIAN_POINT('Origin',(16.,70.,-38.9696551146029));
#36345=CARTESIAN_POINT('',(6.5,74.,-33.4848275573014));
#36346=CARTESIAN_POINT('Origin',(6.5,70.,-33.4848275573014));
#36347=CARTESIAN_POINT('',(6.5,74.,-22.5151724426986));
#36348=CARTESIAN_POINT('Origin',(6.5,70.,-22.5151724426986));
#36349=CARTESIAN_POINT('',(16.,74.,-17.0303448853971));
#36350=CARTESIAN_POINT('Origin',(16.,70.,-28.));
#36351=CARTESIAN_POINT('',(7.5,70.,-28.));
#36352=CARTESIAN_POINT('Origin',(16.,70.,-28.));
#36353=CARTESIAN_POINT('Origin',(16.,81.4267766952966,-28.));
#36354=CARTESIAN_POINT('',(28.,81.,-28.));
#36355=CARTESIAN_POINT('',(4.,81.,-28.));
#36356=CARTESIAN_POINT('Origin',(16.,81.,-28.));
#36357=CARTESIAN_POINT('Origin',(16.,81.,-28.));
#36358=CARTESIAN_POINT('',(27.6464466094067,81.8535533905933,-28.));
#36359=CARTESIAN_POINT('',(27.8232233047034,81.4267766952966,-28.));
#36360=CARTESIAN_POINT('',(4.35355339059327,81.8535533905933,-28.));
#36361=CARTESIAN_POINT('Origin',(16.,81.8535533905933,-28.));
#36362=CARTESIAN_POINT('Origin',(16.,81.8535533905933,-28.));
#36363=CARTESIAN_POINT('Origin',(16.,82.25,-28.));
#36364=CARTESIAN_POINT('',(5.14644660940672,82.6464466094067,-28.));
#36365=CARTESIAN_POINT('',(4.75000000000001,82.25,-28.));
#36366=CARTESIAN_POINT('',(26.8535533905933,82.6464466094067,-28.));
#36367=CARTESIAN_POINT('Origin',(16.,82.6464466094067,-28.));
#36368=CARTESIAN_POINT('Origin',(16.,82.6464466094067,-28.));
#36369=CARTESIAN_POINT('Origin',(16.,77.75,-28.));
#36370=CARTESIAN_POINT('',(4.,79.7,-28.));
#36371=CARTESIAN_POINT('Origin',(16.,79.7,-28.));
#36372=CARTESIAN_POINT('',(4.,77.75,-28.));
#36373=CARTESIAN_POINT('Origin',(16.,82.8232233047034,-28.));
#36374=CARTESIAN_POINT('',(26.,83.,-28.));
#36375=CARTESIAN_POINT('',(26.4267766952966,82.8232233047034,-28.));
#36376=CARTESIAN_POINT('Origin',(16.,83.,-28.));
#36377=CARTESIAN_POINT('Origin',(26.5,83.,-28.));
#36378=CARTESIAN_POINT('Origin',(16.,74.25,-28.));
#36379=CARTESIAN_POINT('',(27.5,74.,-28.));
#36380=CARTESIAN_POINT('Origin',(16.,74.,-28.));
#36381=CARTESIAN_POINT('',(28.,74.5,-28.));
#36382=CARTESIAN_POINT('',(27.75,74.25,-28.));
#36383=CARTESIAN_POINT('',(4.,74.5,-28.));
#36384=CARTESIAN_POINT('Origin',(16.,74.5,-28.));
#36385=CARTESIAN_POINT('Origin',(16.,74.5,-28.));
#36386=CARTESIAN_POINT('Origin',(16.,77.75,-28.));
#36387=CARTESIAN_POINT('',(4.,75.5,-28.));
#36388=CARTESIAN_POINT('',(4.,77.75,-28.));
#36389=CARTESIAN_POINT('Origin',(16.,75.5,-28.));
#36390=CARTESIAN_POINT('Origin',(16.,74.,-28.));
#36391=CARTESIAN_POINT('',(25.5,74.,-33.4848275573015));
#36392=CARTESIAN_POINT('',(16.,74.,-38.9696551146029));
#36393=CARTESIAN_POINT('',(25.5,74.,-22.5151724426986));
#36394=CARTESIAN_POINT('Origin',(28.1,79.7,-28.));
#36395=CARTESIAN_POINT('',(5.,79.7,-28.));
#36396=CARTESIAN_POINT('Origin',(16.,79.7,-28.));
#36397=CARTESIAN_POINT('Origin',(27.,78.5,-28.));
#36398=CARTESIAN_POINT('',(4.,78.5,-28.));
#36399=CARTESIAN_POINT('Origin',(16.,78.5,-28.));
#36400=CARTESIAN_POINT('',(5.,78.5,-28.));
#36401=CARTESIAN_POINT('Origin',(16.,78.5,-28.));
#36402=CARTESIAN_POINT('Origin',(16.,79.1,-28.));
#36403=CARTESIAN_POINT('',(5.,79.1,-28.));
#36404=CARTESIAN_POINT('Origin',(16.,77.75,-28.));
#36405=CARTESIAN_POINT('',(4.,76.7,-28.));
#36406=CARTESIAN_POINT('Origin',(16.,76.7,-28.));
#36407=CARTESIAN_POINT('',(4.,77.75,-28.));
#36408=CARTESIAN_POINT('Origin',(28.1,76.7,-28.));
#36409=CARTESIAN_POINT('',(5.,76.7,-28.));
#36410=CARTESIAN_POINT('Origin',(16.,76.7,-28.));
#36411=CARTESIAN_POINT('Origin',(27.,75.5,-28.));
#36412=CARTESIAN_POINT('',(5.,75.5,-28.));
#36413=CARTESIAN_POINT('Origin',(16.,75.5,-28.));
#36414=CARTESIAN_POINT('Origin',(16.,76.1,-28.));
#36415=CARTESIAN_POINT('',(5.,76.1,-28.));
#36416=CARTESIAN_POINT('Origin',(25.5,70.,-22.5151724426986));
#36417=CARTESIAN_POINT('Origin',(16.,70.,-17.0303448853971));
#36418=CARTESIAN_POINT('Origin',(25.5,70.,-33.4848275573015));
#36419=CARTESIAN_POINT('Origin',(16.,64.5,-28.));
#36420=CARTESIAN_POINT('',(7.5,59.,-28.));
#36421=CARTESIAN_POINT('Origin',(16.,59.,-28.));
#36422=CARTESIAN_POINT('',(7.5,64.5,-28.));
#36423=CARTESIAN_POINT('Origin',(16.,58.75,-28.));
#36424=CARTESIAN_POINT('',(7.8,58.5,-28.));
#36425=CARTESIAN_POINT('Origin',(16.,58.5,-28.));
#36426=CARTESIAN_POINT('',(7.65,58.75,-28.));
#36427=CARTESIAN_POINT('Origin',(16.,58.5,-28.));
#36428=CARTESIAN_POINT('',(0.,0.,0.));
#36429=CARTESIAN_POINT('Origin',(0.,0.,0.));
#36430=CARTESIAN_POINT('',(-4.89858719658941E-16,-5.99903913064743E-32,
8.));
#36431=CARTESIAN_POINT('',(-4.89858719658941E-16,-5.99903913064743E-32,
-8.));
#36432=CARTESIAN_POINT('Origin',(0.,0.,0.));
#36433=CARTESIAN_POINT('',(0.,0.,0.));
#36434=CARTESIAN_POINT('Origin',(3.,0.,0.));
#36435=CARTESIAN_POINT('',(6.,-6.,-7.34788079488412E-16));
#36436=CARTESIAN_POINT('Origin',(6.,0.,0.));
#36437=CARTESIAN_POINT('',(0.,-6.,-7.34788079488412E-16));
#36438=CARTESIAN_POINT('',(3.,-6.,-7.34788079488412E-16));
#36439=CARTESIAN_POINT('Origin',(0.,0.,0.));
#36440=CARTESIAN_POINT('Origin',(0.,12.5,0.));
#36441=CARTESIAN_POINT('',(6.93889390390723E-17,-12.5,-1.53080849893419E-15));
#36442=CARTESIAN_POINT('Origin',(0.,0.,0.));
#36443=CARTESIAN_POINT('Origin',(0.25,0.,0.));
#36444=CARTESIAN_POINT('',(0.500000000000001,-13.,-1.59204083889156E-15));
#36445=CARTESIAN_POINT('Origin',(0.5,0.,0.));
#36446=CARTESIAN_POINT('',(0.25,-12.75,-1.56142466891288E-15));
#36447=CARTESIAN_POINT('Origin',(3.,0.,0.));
#36448=CARTESIAN_POINT('',(5.5,-13.,-1.59204083889156E-15));
#36449=CARTESIAN_POINT('Origin',(5.5,0.,0.));
#36450=CARTESIAN_POINT('',(3.,-13.,-1.59204083889156E-15));
#36451=CARTESIAN_POINT('Origin',(5.75,0.,0.));
#36452=CARTESIAN_POINT('',(6.,-12.5,-1.53080849893419E-15));
#36453=CARTESIAN_POINT('Origin',(6.,0.,0.));
#36454=CARTESIAN_POINT('',(5.75,-12.75,-1.56142466891288E-15));
#36455=CARTESIAN_POINT('Origin',(6.,6.,0.));
#36456=CARTESIAN_POINT('',(0.,0.,0.));
#36457=CARTESIAN_POINT('Origin',(61.,-66.,18.25));
#36458=CARTESIAN_POINT('',(57.,-66.,18.));
#36459=CARTESIAN_POINT('Origin',(61.,-66.,18.));
#36460=CARTESIAN_POINT('',(57.5,-66.,18.5));
#36461=CARTESIAN_POINT('',(57.25,-66.,18.25));
#36462=CARTESIAN_POINT('Origin',(61.,-66.,18.5));
#36463=CARTESIAN_POINT('Origin',(80.,-72.5,18.));
#36464=CARTESIAN_POINT('',(42.8,-72.,18.));
#36465=CARTESIAN_POINT('',(79.2,-72.,18.));
#36466=CARTESIAN_POINT('',(70.5,-72.,18.));
#36467=CARTESIAN_POINT('',(42.8,72.,18.));
#36468=CARTESIAN_POINT('',(42.8,-72.5,18.));
#36469=CARTESIAN_POINT('',(79.2,72.,18.));
#36470=CARTESIAN_POINT('',(70.5,72.,18.));
#36471=CARTESIAN_POINT('',(79.2,-72.5,18.));
#36472=CARTESIAN_POINT('',(57.,66.,18.));
#36473=CARTESIAN_POINT('Origin',(61.,66.,18.));
#36474=CARTESIAN_POINT('',(56.5,52.5,18.));
#36475=CARTESIAN_POINT('Origin',(61.,52.5,18.));
#36476=CARTESIAN_POINT('',(56.5,-25.,18.));
#36477=CARTESIAN_POINT('Origin',(61.,-25.,18.));
#36478=CARTESIAN_POINT('',(56.5,25.,18.));
#36479=CARTESIAN_POINT('Origin',(61.,25.,18.));
#36480=CARTESIAN_POINT('',(56.5,-52.5,18.));
#36481=CARTESIAN_POINT('Origin',(61.,-52.5,18.));
#36482=CARTESIAN_POINT('Origin',(61.,-66.,21.));
#36483=CARTESIAN_POINT('',(57.5,-66.,20.5));
#36484=CARTESIAN_POINT('Origin',(61.,-66.,20.5));
#36485=CARTESIAN_POINT('',(57.5,-66.,21.));
#36486=CARTESIAN_POINT('Origin',(61.,66.,18.25));
#36487=CARTESIAN_POINT('',(57.5,66.,18.5));
#36488=CARTESIAN_POINT('',(57.25,66.,18.25));
#36489=CARTESIAN_POINT('Origin',(61.,66.,18.5));
#36490=CARTESIAN_POINT('Origin',(61.,66.,21.));
#36491=CARTESIAN_POINT('',(57.5,66.,20.5));
#36492=CARTESIAN_POINT('Origin',(61.,66.,20.5));
#36493=CARTESIAN_POINT('',(57.5,66.,21.));
#36494=CARTESIAN_POINT('Origin',(50.,-72.25,20.75));
#36495=CARTESIAN_POINT('',(39.8,-72.,21.));
#36496=CARTESIAN_POINT('',(39.8,-72.5,20.5));
#36497=CARTESIAN_POINT('',(39.8,-72.,21.));
#36498=CARTESIAN_POINT('',(82.2,-72.5,20.5));
#36499=CARTESIAN_POINT('',(50.,-72.5,20.5));
#36500=CARTESIAN_POINT('',(82.2,-72.,21.));
#36501=CARTESIAN_POINT('',(82.2,-72.5,20.5));
#36502=CARTESIAN_POINT('',(50.,-72.,21.));
#36503=CARTESIAN_POINT('Origin',(39.8,-72.25,20.2));
#36504=CARTESIAN_POINT('',(39.,-72.,20.2));
#36505=CARTESIAN_POINT('Origin',(39.8,-72.,20.2));
#36506=CARTESIAN_POINT('',(39.5,-72.5,20.2));
#36507=CARTESIAN_POINT('',(39.,-72.,20.2));
#36508=CARTESIAN_POINT('Origin',(39.8,-72.5,20.2));
#36509=CARTESIAN_POINT('Origin',(39.25,-72.25,9.75));
#36510=CARTESIAN_POINT('',(39.,-72.,6.8));
#36511=CARTESIAN_POINT('',(39.5,-72.5,6.8));
#36512=CARTESIAN_POINT('',(39.,-72.,6.8));
#36513=CARTESIAN_POINT('',(39.5,-72.5,9.75));
#36514=CARTESIAN_POINT('',(39.,-72.,9.75));
#36515=CARTESIAN_POINT('Origin',(39.8,-72.25,6.8));
#36516=CARTESIAN_POINT('',(39.8,-72.,6.));
#36517=CARTESIAN_POINT('Origin',(39.8,-72.,6.8));
#36518=CARTESIAN_POINT('',(39.8,-72.5,6.5));
#36519=CARTESIAN_POINT('',(39.8,-72.,6.));
#36520=CARTESIAN_POINT('Origin',(39.8,-72.5,6.8));
#36521=CARTESIAN_POINT('Origin',(51.5,-72.25,6.25));
#36522=CARTESIAN_POINT('',(41.2,-72.,6.));
#36523=CARTESIAN_POINT('',(41.2,-72.5,6.5));
#36524=CARTESIAN_POINT('',(41.2,-72.,6.));
#36525=CARTESIAN_POINT('',(51.5,-72.5,6.5));
#36526=CARTESIAN_POINT('',(51.5,-72.,6.));
#36527=CARTESIAN_POINT('Origin',(41.2,-72.25,6.8));
#36528=CARTESIAN_POINT('',(42.,-72.,6.8));
#36529=CARTESIAN_POINT('Origin',(41.2,-72.,6.8));
#36530=CARTESIAN_POINT('',(41.5,-72.5,6.8));
#36531=CARTESIAN_POINT('',(42.,-72.,6.8));
#36532=CARTESIAN_POINT('Origin',(41.2,-72.5,6.8));
#36533=CARTESIAN_POINT('Origin',(41.75,-72.25,15.75));
#36534=CARTESIAN_POINT('',(42.,-72.,17.2));
#36535=CARTESIAN_POINT('',(41.5,-72.5,17.2));
#36536=CARTESIAN_POINT('',(42.,-72.,17.2));
#36537=CARTESIAN_POINT('',(41.5,-72.5,15.75));
#36538=CARTESIAN_POINT('',(42.,-72.,15.75));
#36539=CARTESIAN_POINT('Origin',(42.8,-72.25,17.2));
#36540=CARTESIAN_POINT('Origin',(42.8,-72.,17.2));
#36541=CARTESIAN_POINT('',(42.8,-72.5,18.5));
#36542=CARTESIAN_POINT('',(42.8,-72.,18.));
#36543=CARTESIAN_POINT('Origin',(42.8,-72.5,17.2));
#36544=CARTESIAN_POINT('Origin',(70.5,-72.25,18.25));
#36545=CARTESIAN_POINT('',(79.2,-72.5,18.5));
#36546=CARTESIAN_POINT('',(79.2,-72.,18.));
#36547=CARTESIAN_POINT('',(70.5,-72.5,18.5));
#36548=CARTESIAN_POINT('Origin',(79.2,-72.25,17.2));
#36549=CARTESIAN_POINT('',(80.,-72.,17.2));
#36550=CARTESIAN_POINT('Origin',(79.2,-72.,17.2));
#36551=CARTESIAN_POINT('',(80.5,-72.5,17.2));
#36552=CARTESIAN_POINT('',(80.,-72.,17.2));
#36553=CARTESIAN_POINT('Origin',(79.2,-72.5,17.2));
#36554=CARTESIAN_POINT('Origin',(80.25,-72.25,9.75));
#36555=CARTESIAN_POINT('',(80.,-72.,6.8));
#36556=CARTESIAN_POINT('',(80.5,-72.5,6.8));
#36557=CARTESIAN_POINT('',(80.,-72.,6.8));
#36558=CARTESIAN_POINT('',(80.5,-72.5,9.75));
#36559=CARTESIAN_POINT('',(80.,-72.,9.75));
#36560=CARTESIAN_POINT('Origin',(80.8,-72.25,6.8));
#36561=CARTESIAN_POINT('',(80.8,-72.,6.));
#36562=CARTESIAN_POINT('Origin',(80.8,-72.,6.8));
#36563=CARTESIAN_POINT('',(80.8,-72.5,6.5));
#36564=CARTESIAN_POINT('',(80.8,-72.,6.));
#36565=CARTESIAN_POINT('Origin',(80.8,-72.5,6.8));
#36566=CARTESIAN_POINT('Origin',(72.,-72.25,6.25));
#36567=CARTESIAN_POINT('',(82.2,-72.,6.));
#36568=CARTESIAN_POINT('',(82.2,-72.5,6.5));
#36569=CARTESIAN_POINT('',(82.2,-72.,6.));
#36570=CARTESIAN_POINT('',(72.,-72.5,6.5));
#36571=CARTESIAN_POINT('',(72.,-72.,6.));
#36572=CARTESIAN_POINT('Origin',(82.2,-72.25,6.8));
#36573=CARTESIAN_POINT('',(83.,-72.,6.8));
#36574=CARTESIAN_POINT('Origin',(82.2,-72.,6.8));
#36575=CARTESIAN_POINT('',(82.5,-72.5,6.8));
#36576=CARTESIAN_POINT('',(83.,-72.,6.8));
#36577=CARTESIAN_POINT('Origin',(82.2,-72.5,6.8));
#36578=CARTESIAN_POINT('Origin',(82.75,-72.25,17.25));
#36579=CARTESIAN_POINT('',(83.,-72.,20.2));
#36580=CARTESIAN_POINT('',(82.5,-72.5,20.2));
#36581=CARTESIAN_POINT('',(83.,-72.,20.2));
#36582=CARTESIAN_POINT('',(82.5,-72.5,17.25));
#36583=CARTESIAN_POINT('',(83.,-72.,17.25));
#36584=CARTESIAN_POINT('Origin',(82.2,-72.25,20.2));
#36585=CARTESIAN_POINT('Origin',(82.2,-72.,20.2));
#36586=CARTESIAN_POINT('Origin',(82.2,-72.5,20.2));
#36587=CARTESIAN_POINT('Origin',(42.8,-72.5,17.2));
#36588=CARTESIAN_POINT('',(42.,72.,17.2));
#36589=CARTESIAN_POINT('',(42.,-72.5,17.2));
#36590=CARTESIAN_POINT('Origin',(42.8,72.,17.2));
#36591=CARTESIAN_POINT('Origin',(42.,-72.5,18.));
#36592=CARTESIAN_POINT('',(42.,72.,6.8));
#36593=CARTESIAN_POINT('',(42.,-72.5,6.8));
#36594=CARTESIAN_POINT('',(42.,72.,15.75));
#36595=CARTESIAN_POINT('Origin',(41.2,-72.5,6.8));
#36596=CARTESIAN_POINT('',(41.2,72.,6.));
#36597=CARTESIAN_POINT('',(41.2,-72.5,6.));
#36598=CARTESIAN_POINT('Origin',(41.2,72.,6.8));
#36599=CARTESIAN_POINT('Origin',(42.,-72.5,6.));
#36600=CARTESIAN_POINT('',(39.8,72.,6.));
#36601=CARTESIAN_POINT('',(39.8,-72.5,6.));
#36602=CARTESIAN_POINT('',(51.5,72.,6.));
#36603=CARTESIAN_POINT('Origin',(39.8,-72.5,6.8));
#36604=CARTESIAN_POINT('',(39.,72.,6.8));
#36605=CARTESIAN_POINT('',(39.,-72.5,6.8));
#36606=CARTESIAN_POINT('Origin',(39.8,72.,6.8));
#36607=CARTESIAN_POINT('Origin',(39.,-72.5,6.));
#36608=CARTESIAN_POINT('',(39.,72.,20.2));
#36609=CARTESIAN_POINT('',(39.,-72.5,20.2));
#36610=CARTESIAN_POINT('',(39.,72.,9.75));
#36611=CARTESIAN_POINT('Origin',(39.8,-72.5,20.2));
#36612=CARTESIAN_POINT('',(39.8,72.,21.));
#36613=CARTESIAN_POINT('',(39.8,-72.5,21.));
#36614=CARTESIAN_POINT('Origin',(39.8,72.,20.2));
#36615=CARTESIAN_POINT('Origin',(39.,-72.5,21.));
#36616=CARTESIAN_POINT('',(82.2,72.,21.));
#36617=CARTESIAN_POINT('',(82.2,-72.5,21.));
#36618=CARTESIAN_POINT('',(50.,72.,21.));
#36619=CARTESIAN_POINT('',(57.,-66.,21.));
#36620=CARTESIAN_POINT('Origin',(61.,-66.,21.));
#36621=CARTESIAN_POINT('',(56.5,-52.5,21.));
#36622=CARTESIAN_POINT('Origin',(61.,-52.5,21.));
#36623=CARTESIAN_POINT('',(56.5,25.,21.));
#36624=CARTESIAN_POINT('Origin',(61.,25.,21.));
#36625=CARTESIAN_POINT('',(56.5,-25.,21.));
#36626=CARTESIAN_POINT('Origin',(61.,-25.,21.));
#36627=CARTESIAN_POINT('',(56.5,52.5,21.));
#36628=CARTESIAN_POINT('Origin',(61.,52.5,21.));
#36629=CARTESIAN_POINT('',(57.,66.,21.));
#36630=CARTESIAN_POINT('Origin',(61.,66.,21.));
#36631=CARTESIAN_POINT('Origin',(61.,-72.5,13.5));
#36632=CARTESIAN_POINT('Origin',(50.,72.25,20.75));
#36633=CARTESIAN_POINT('',(82.2,72.5,20.5));
#36634=CARTESIAN_POINT('',(82.2,72.,21.));
#36635=CARTESIAN_POINT('',(39.8,72.5,20.5));
#36636=CARTESIAN_POINT('',(50.,72.5,20.5));
#36637=CARTESIAN_POINT('',(39.8,72.5,20.5));
#36638=CARTESIAN_POINT('Origin',(82.2,72.25,20.2));
#36639=CARTESIAN_POINT('',(83.,72.,20.2));
#36640=CARTESIAN_POINT('Origin',(82.2,72.,20.2));
#36641=CARTESIAN_POINT('',(82.5,72.5,20.2));
#36642=CARTESIAN_POINT('',(83.,72.,20.2));
#36643=CARTESIAN_POINT('Origin',(82.2,72.5,20.2));
#36644=CARTESIAN_POINT('Origin',(82.75,72.25,17.25));
#36645=CARTESIAN_POINT('',(83.,72.,6.8));
#36646=CARTESIAN_POINT('',(82.5,72.5,6.8));
#36647=CARTESIAN_POINT('',(83.,72.,6.8));
#36648=CARTESIAN_POINT('',(82.5,72.5,17.25));
#36649=CARTESIAN_POINT('',(83.,72.,17.25));
#36650=CARTESIAN_POINT('Origin',(82.2,72.25,6.8));
#36651=CARTESIAN_POINT('',(82.2,72.,6.));
#36652=CARTESIAN_POINT('Origin',(82.2,72.,6.8));
#36653=CARTESIAN_POINT('',(82.2,72.5,6.5));
#36654=CARTESIAN_POINT('',(82.2,72.,6.));
#36655=CARTESIAN_POINT('Origin',(82.2,72.5,6.8));
#36656=CARTESIAN_POINT('Origin',(72.,72.25,6.25));
#36657=CARTESIAN_POINT('',(80.8,72.,6.));
#36658=CARTESIAN_POINT('',(80.8,72.5,6.5));
#36659=CARTESIAN_POINT('',(80.8,72.,6.));
#36660=CARTESIAN_POINT('',(72.,72.5,6.5));
#36661=CARTESIAN_POINT('',(72.,72.,6.));
#36662=CARTESIAN_POINT('Origin',(80.8,72.25,6.8));
#36663=CARTESIAN_POINT('',(80.,72.,6.8));
#36664=CARTESIAN_POINT('Origin',(80.8,72.,6.8));
#36665=CARTESIAN_POINT('',(80.5,72.5,6.8));
#36666=CARTESIAN_POINT('',(80.,72.,6.8));
#36667=CARTESIAN_POINT('Origin',(80.8,72.5,6.8));
#36668=CARTESIAN_POINT('Origin',(80.25,72.25,9.75));
#36669=CARTESIAN_POINT('',(80.,72.,17.2));
#36670=CARTESIAN_POINT('',(80.5,72.5,17.2));
#36671=CARTESIAN_POINT('',(80.,72.,17.2));
#36672=CARTESIAN_POINT('',(80.5,72.5,9.75));
#36673=CARTESIAN_POINT('',(80.,72.,9.75));
#36674=CARTESIAN_POINT('Origin',(79.2,72.25,17.2));
#36675=CARTESIAN_POINT('Origin',(79.2,72.,17.2));
#36676=CARTESIAN_POINT('',(79.2,72.5,18.5));
#36677=CARTESIAN_POINT('',(79.2,72.,18.));
#36678=CARTESIAN_POINT('Origin',(79.2,72.5,17.2));
#36679=CARTESIAN_POINT('Origin',(70.5,72.25,18.25));
#36680=CARTESIAN_POINT('',(42.8,72.5,18.5));
#36681=CARTESIAN_POINT('',(42.8,72.,18.));
#36682=CARTESIAN_POINT('',(70.5,72.5,18.5));
#36683=CARTESIAN_POINT('Origin',(42.8,72.25,17.2));
#36684=CARTESIAN_POINT('',(41.5,72.5,17.2));
#36685=CARTESIAN_POINT('',(42.,72.,17.2));
#36686=CARTESIAN_POINT('Origin',(42.8,72.5,17.2));
#36687=CARTESIAN_POINT('Origin',(41.75,72.25,15.75));
#36688=CARTESIAN_POINT('',(41.5,72.5,6.8));
#36689=CARTESIAN_POINT('',(42.,72.,6.8));
#36690=CARTESIAN_POINT('',(41.5,72.5,15.75));
#36691=CARTESIAN_POINT('Origin',(41.2,72.25,6.8));
#36692=CARTESIAN_POINT('',(41.2,72.5,6.5));
#36693=CARTESIAN_POINT('',(41.2,72.,6.));
#36694=CARTESIAN_POINT('Origin',(41.2,72.5,6.8));
#36695=CARTESIAN_POINT('Origin',(51.5,72.25,6.25));
#36696=CARTESIAN_POINT('',(39.8,72.5,6.5));
#36697=CARTESIAN_POINT('',(39.8,72.,6.));
#36698=CARTESIAN_POINT('',(51.5,72.5,6.5));
#36699=CARTESIAN_POINT('Origin',(39.8,72.25,6.8));
#36700=CARTESIAN_POINT('',(39.5,72.5,6.8));
#36701=CARTESIAN_POINT('',(39.,72.,6.8));
#36702=CARTESIAN_POINT('Origin',(39.8,72.5,6.8));
#36703=CARTESIAN_POINT('Origin',(39.25,72.25,9.75));
#36704=CARTESIAN_POINT('',(39.5,72.5,20.2));
#36705=CARTESIAN_POINT('',(39.,72.,20.2));
#36706=CARTESIAN_POINT('',(39.5,72.5,9.75));
#36707=CARTESIAN_POINT('Origin',(39.8,72.25,20.2));
#36708=CARTESIAN_POINT('Origin',(39.8,72.5,20.2));
#36709=CARTESIAN_POINT('Origin',(79.2,-72.5,17.2));
#36710=CARTESIAN_POINT('',(80.,-72.5,17.2));
#36711=CARTESIAN_POINT('Origin',(80.,-72.5,6.));
#36712=CARTESIAN_POINT('',(80.,-72.5,6.8));
#36713=CARTESIAN_POINT('Origin',(80.8,-72.5,6.8));
#36714=CARTESIAN_POINT('',(80.8,-72.5,6.));
#36715=CARTESIAN_POINT('Origin',(83.,-72.5,6.));
#36716=CARTESIAN_POINT('',(82.2,-72.5,6.));
#36717=CARTESIAN_POINT('Origin',(82.2,-72.5,6.8));
#36718=CARTESIAN_POINT('',(83.,-72.5,6.8));
#36719=CARTESIAN_POINT('Origin',(83.,-72.5,21.));
#36720=CARTESIAN_POINT('',(83.,-72.5,20.2));
#36721=CARTESIAN_POINT('Origin',(82.2,-72.5,20.2));
#36722=CARTESIAN_POINT('Origin',(61.,72.5,13.5));
#36723=CARTESIAN_POINT('Origin',(61.,66.,20.75));
#36724=CARTESIAN_POINT('',(57.25,66.,20.75));
#36725=CARTESIAN_POINT('Origin',(61.,-66.,20.75));
#36726=CARTESIAN_POINT('',(57.25,-66.,20.75));
#36727=CARTESIAN_POINT('Origin',(61.,-52.5,21.));
#36728=CARTESIAN_POINT('',(56.5,-52.5,21.));
#36729=CARTESIAN_POINT('Origin',(61.,25.,21.));
#36730=CARTESIAN_POINT('',(56.5,25.,21.));
#36731=CARTESIAN_POINT('Origin',(61.,-25.,21.));
#36732=CARTESIAN_POINT('',(56.5,-25.,21.));
#36733=CARTESIAN_POINT('Origin',(61.,52.5,21.));
#36734=CARTESIAN_POINT('',(56.5,52.5,21.));
#36735=CARTESIAN_POINT('',(0.,0.,0.));
#36736=CARTESIAN_POINT('Origin',(23.75,0.,0.));
#36737=CARTESIAN_POINT('',(18.404163522035,-3.93613844682217,0.0030445838845216));
#36738=CARTESIAN_POINT('',(18.220836477965,-3.93627057114866,0.00387085077091485));
#36739=CARTESIAN_POINT('',(23.75,-3.933,-4.81653586104654E-16));
#36740=CARTESIAN_POINT('',(18.,1.74869447533107,3.5228619944509));
#36741=CARTESIAN_POINT('Ctrl Pts',(18.404163522035,-3.93613844682217,0.0030445838845216));
#36742=CARTESIAN_POINT('Ctrl Pts',(18.3945483991958,-3.93767917958426,0.192676392097596));
#36743=CARTESIAN_POINT('Ctrl Pts',(18.3849332763566,-3.92513522773623,0.38209457511149));
#36744=CARTESIAN_POINT('Ctrl Pts',(18.3753181535174,-3.89779650413505,0.569340254555103));
#36745=CARTESIAN_POINT('Ctrl Pts',(18.3098697216666,-3.71170667268696,1.84388830717668));
#36746=CARTESIAN_POINT('Ctrl Pts',(18.2444212898158,-2.84013321415606,3.01777812376358));
#36747=CARTESIAN_POINT('Ctrl Pts',(18.178972857965,-1.67389089476471,3.56551633596367));
#36748=CARTESIAN_POINT('Ctrl Pts',(18.1193152386434,-0.610836542511951,
4.06479121279916));
#36749=CARTESIAN_POINT('Ctrl Pts',(18.0596576193217,0.697049477382223,4.04381518476905));
#36750=CARTESIAN_POINT('Ctrl Pts',(18.,1.75280451302835,3.52727163111204));
#36751=CARTESIAN_POINT('',(18.,-1.74869447533112,3.52286199445088));
#36752=CARTESIAN_POINT('Origin',(18.,0.,0.));
#36753=CARTESIAN_POINT('Ctrl Pts',(18.,-1.74869447533111,3.52286199445088));
#36754=CARTESIAN_POINT('Ctrl Pts',(18.0654484318508,-2.90764455848562,2.94757701002937));
#36755=CARTESIAN_POINT('Ctrl Pts',(18.1308968637015,-3.7512349686817,1.76098836716689));
#36756=CARTESIAN_POINT('Ctrl Pts',(18.1963452955523,-3.90885202961768,0.484525031295026));
#36757=CARTESIAN_POINT('Ctrl Pts',(18.2045090230232,-3.92851243543427,0.325305039219235));
#36758=CARTESIAN_POINT('Ctrl Pts',(18.2126727504941,-3.93749985993302,0.164686697017349));
#36759=CARTESIAN_POINT('Ctrl Pts',(18.220836477965,-3.93627057114866,0.00387085077091485));
#36760=CARTESIAN_POINT('Origin',(23.75,0.,0.));
#36761=CARTESIAN_POINT('',(19.654163522035,-3.92689321902701,-0.000266995866781417));
#36762=CARTESIAN_POINT('',(19.470836477965,-3.9268765274925,0.000201000649742641));
#36763=CARTESIAN_POINT('',(23.75,-3.933,-4.81653586104654E-16));
#36764=CARTESIAN_POINT('Ctrl Pts',(19.654163522035,-3.92689321902701,-0.000266995866781417));
#36765=CARTESIAN_POINT('Ctrl Pts',(19.6205723236338,-3.92647671847103,0.666255959009758));
#36766=CARTESIAN_POINT('Ctrl Pts',(19.5869811252325,-3.76529862270708,1.33296720638558));
#36767=CARTESIAN_POINT('Ctrl Pts',(19.5533899268313,-3.44451966305658,1.91112423318315));
#36768=CARTESIAN_POINT('Ctrl Pts',(19.4879414949806,-2.81952023228035,3.03759403981093));
#36769=CARTESIAN_POINT('Ctrl Pts',(19.4224930631298,-1.58864622066021,3.82789554528875));
#36770=CARTESIAN_POINT('Ctrl Pts',(19.357044631279,-0.304251272167243,3.92740159534381));
#36771=CARTESIAN_POINT('Ctrl Pts',(19.2915961994282,0.980143676325715,4.02690764539886));
#36772=CARTESIAN_POINT('Ctrl Pts',(19.2261477675775,2.3180595616915,3.43561824003117));
#36773=CARTESIAN_POINT('Ctrl Pts',(19.1606993357267,3.10909064786165,2.41883077544061));
#36774=CARTESIAN_POINT('Ctrl Pts',(19.0952509038759,3.9001217340318,1.40204331085005));
#36775=CARTESIAN_POINT('Ctrl Pts',(19.0298024720251,4.14426802100631,-0.0402422129633744));
#36776=CARTESIAN_POINT('Ctrl Pts',(18.9643540401743,3.7319893739621,-1.26070538200933));
#36777=CARTESIAN_POINT('Ctrl Pts',(18.8989056083236,3.31971072691789,-2.48116855105527));
#36778=CARTESIAN_POINT('Ctrl Pts',(18.8334571764728,2.25100714585497,-3.47980936533375));
#36779=CARTESIAN_POINT('Ctrl Pts',(18.768008744622,1.00542163713921,-3.80865813843412));
#36780=CARTESIAN_POINT('Ctrl Pts',(18.7025603127713,-0.240163871576541,
-4.13750691153448));
#36781=CARTESIAN_POINT('Ctrl Pts',(18.6371118809205,-1.66263130794512,-3.79656364345673));
#36782=CARTESIAN_POINT('Ctrl Pts',(18.5716634490697,-2.62356192394677,-2.93848886508973));
#36783=CARTESIAN_POINT('Ctrl Pts',(18.5158301400581,-3.44332084718932,-2.20647508109503));
#36784=CARTESIAN_POINT('Ctrl Pts',(18.4599968310465,-3.92719168557441,-1.09811361486684));
#36785=CARTESIAN_POINT('Ctrl Pts',(18.404163522035,-3.93613844682217,0.0030445838845216));
#36786=CARTESIAN_POINT('Ctrl Pts',(18.220836477965,-3.93627057114866,0.00387085077091485));
#36787=CARTESIAN_POINT('Ctrl Pts',(18.2781211823449,-3.92764467754057,-1.12457056825791));
#36788=CARTESIAN_POINT('Ctrl Pts',(18.3354058867248,-3.41596831095298,-2.26273669035632));
#36789=CARTESIAN_POINT('Ctrl Pts',(18.3926905911047,-2.55888297838309,-2.99573282302492));
#36790=CARTESIAN_POINT('Ctrl Pts',(18.4581390229554,-1.57965315453669,-3.83318931259173));
#36791=CARTESIAN_POINT('Ctrl Pts',(18.5235874548062,-0.149549795168021,
-4.14176426284409));
#36792=CARTESIAN_POINT('Ctrl Pts',(18.589035886657,1.08866631561176,-3.78545010096408));
#36793=CARTESIAN_POINT('Ctrl Pts',(18.6544843185077,2.32688242639155,-3.42913593908406));
#36794=CARTESIAN_POINT('Ctrl Pts',(18.7199327503585,3.37321128858245,-2.40793266507167));
#36795=CARTESIAN_POINT('Ctrl Pts',(18.7853811822093,3.75861745519042,-1.1788821270789));
#36796=CARTESIAN_POINT('Ctrl Pts',(18.8508296140601,4.14402362179839,0.0501684109138591));
#36797=CARTESIAN_POINT('Ctrl Pts',(18.9162780459109,3.86850709282343,1.48706621288699));
#36798=CARTESIAN_POINT('Ctrl Pts',(18.9817264777616,3.05544614190684,2.48637190452309));
#36799=CARTESIAN_POINT('Ctrl Pts',(19.0471749096124,2.24238519099026,3.4856775961592));
#36800=CARTESIAN_POINT('Ctrl Pts',(19.1126233414632,0.891779818132044,4.04739117745827));
#36801=CARTESIAN_POINT('Ctrl Pts',(19.178071773314,-0.390146913530757,3.91976270565962));
#36802=CARTESIAN_POINT('Ctrl Pts',(19.2435202051647,-1.67207364519356,3.79213423386097));
#36803=CARTESIAN_POINT('Ctrl Pts',(19.3089686370155,-2.88532173566096,2.97516370896458));
#36804=CARTESIAN_POINT('Ctrl Pts',(19.3744170688663,-3.48551032220533,1.83530485432315));
#36805=CARTESIAN_POINT('Ctrl Pts',(19.4065568718992,-3.78024531292475,1.27555364199425));
#36806=CARTESIAN_POINT('Ctrl Pts',(19.4386966749321,-3.92714077791773,0.637937789729678));
#36807=CARTESIAN_POINT('Ctrl Pts',(19.470836477965,-3.9268765274925,0.000201000649742641));
#36808=CARTESIAN_POINT('Origin',(23.75,0.,0.));
#36809=CARTESIAN_POINT('',(20.904163522035,-3.93705835258154,-0.00244415858371427));
#36810=CARTESIAN_POINT('',(20.720836477965,-3.93634147379978,-0.00275764000347982));
#36811=CARTESIAN_POINT('',(23.75,-3.933,-4.81653586104654E-16));
#36812=CARTESIAN_POINT('Ctrl Pts',(20.904163522035,-3.93705835258154,-0.00244415858371427));
#36813=CARTESIAN_POINT('Ctrl Pts',(20.8465962480717,-3.92872844902641,1.13228879098002));
#36814=CARTESIAN_POINT('Ctrl Pts',(20.7890289741085,-3.41049682016329,2.27366756012711));
#36815=CARTESIAN_POINT('Ctrl Pts',(20.7314617001453,-2.54581885219839,3.00597915976938));
#36816=CARTESIAN_POINT('Ctrl Pts',(20.6660132682945,-1.5627634951674,3.83854673719779));
#36817=CARTESIAN_POINT('Ctrl Pts',(20.6005648364438,-0.131909118660247,
4.14237477626342));
#36818=CARTESIAN_POINT('Ctrl Pts',(20.535116404593,1.10464315307146,3.78111974646024));
#36819=CARTESIAN_POINT('Ctrl Pts',(20.4696679727422,2.34119542480316,3.41986471665706));
#36820=CARTESIAN_POINT('Ctrl Pts',(20.4042195408914,3.38344559175942,2.39352661798506));
#36821=CARTESIAN_POINT('Ctrl Pts',(20.3387711090406,3.76367980962101,1.1626776497403));
#36822=CARTESIAN_POINT('Ctrl Pts',(20.2733226771899,4.14391402748261,-0.0681713185044673));
#36823=CARTESIAN_POINT('Ctrl Pts',(20.2078742453391,3.86213229624954,-1.503531156322));
#36824=CARTESIAN_POINT('Ctrl Pts',(20.1424258134883,3.04478561004353,-2.49927715158322));
#36825=CARTESIAN_POINT('Ctrl Pts',(20.0769773816376,2.22743892383752,-3.49502314684444));
#36826=CARTESIAN_POINT('Ctrl Pts',(20.0115289497868,0.874527282658571,-4.05115529954934));
#36827=CARTESIAN_POINT('Ctrl Pts',(19.946080517936,-0.40682594379375,-3.9181104320261));
#36828=CARTESIAN_POINT('Ctrl Pts',(19.8806320860852,-1.68817917024607,-3.78506556450286));
#36829=CARTESIAN_POINT('Ctrl Pts',(19.8151836542344,-2.89797398197177,-2.96284367675147));
#36830=CARTESIAN_POINT('Ctrl Pts',(19.7497352223837,-3.49330896286845,-1.82041367898691));
#36831=CARTESIAN_POINT('Ctrl Pts',(19.7178779889341,-3.78309016817464,-1.2643322250943));
#36832=CARTESIAN_POINT('Ctrl Pts',(19.6860207554845,-3.92728821998187,-0.632384288003329));
#36833=CARTESIAN_POINT('Ctrl Pts',(19.654163522035,-3.92689321902701,-0.000266995866781417));
#36834=CARTESIAN_POINT('Ctrl Pts',(19.470836477965,-3.9268765274925,0.000201000649742641));
#36835=CARTESIAN_POINT('Ctrl Pts',(19.5041451067829,-3.92660266709205,-0.66072831398253));
#36836=CARTESIAN_POINT('Ctrl Pts',(19.5374537356008,-3.76827097225227,-1.32178752157556));
#36837=CARTESIAN_POINT('Ctrl Pts',(19.5707623644186,-3.45263815106435,-1.89643882110259));
#36838=CARTESIAN_POINT('Ctrl Pts',(19.6362107962694,-2.83244831075765,-3.02557645750042));
#36839=CARTESIAN_POINT('Ctrl Pts',(19.7016592281202,-1.60493954752288,-3.8211045459096));
#36840=CARTESIAN_POINT('Ctrl Pts',(19.7671076599709,-0.320979108461926,
-3.92607034958216));
#36841=CARTESIAN_POINT('Ctrl Pts',(19.8325560918217,0.962981330599031,-4.03103615325472));
#36842=CARTESIAN_POINT('Ctrl Pts',(19.8980045236725,2.30339344548619,-3.44543967219065));
#36843=CARTESIAN_POINT('Ctrl Pts',(19.9634529555233,3.09875161344691,-2.43204719578226));
#36844=CARTESIAN_POINT('Ctrl Pts',(20.028901387374,3.89410978140763,-1.41865471937386));
#36845=CARTESIAN_POINT('Ctrl Pts',(20.0943498192248,4.14441400244192,0.022533752378857));
#36846=CARTESIAN_POINT('Ctrl Pts',(20.1597982510756,3.73733454864532,1.24476807205102));
#36847=CARTESIAN_POINT('Ctrl Pts',(20.2252466829264,3.33025509484873,2.46700239172319));
#36848=CARTESIAN_POINT('Ctrl Pts',(20.2906951147771,2.26579196622125,3.4702825593148));
#36849=CARTESIAN_POINT('Ctrl Pts',(20.3561435466279,1.02162940702816,3.80438874667093));
#36850=CARTESIAN_POINT('Ctrl Pts',(20.4215919784787,-0.222533152164935,
4.13849493402707));
#36851=CARTESIAN_POINT('Ctrl Pts',(20.4870404103295,-1.64639514192364,3.80342714114774));
#36852=CARTESIAN_POINT('Ctrl Pts',(20.5524888421803,-2.61099445316008,2.94954526738738));
#36853=CARTESIAN_POINT('Ctrl Pts',(20.6086047207752,-3.4380476966283,2.21742181985246));
#36854=CARTESIAN_POINT('Ctrl Pts',(20.6647205993701,-3.92747625062555,1.1038947635718));
#36855=CARTESIAN_POINT('Ctrl Pts',(20.720836477965,-3.93634147379978,-0.00275764000347982));
#36856=CARTESIAN_POINT('Origin',(23.75,0.,0.));
#36857=CARTESIAN_POINT('',(22.154163522035,-3.93253297961002,0.00339845520594975));
#36858=CARTESIAN_POINT('',(21.970836477965,-3.93336915469688,0.00337969667030601));
#36859=CARTESIAN_POINT('',(23.75,-3.933,-4.81653586104654E-16));
#36860=CARTESIAN_POINT('Ctrl Pts',(22.154163522035,-3.93253297961002,0.00339845520594975));
#36861=CARTESIAN_POINT('Ctrl Pts',(22.1380686043605,-3.93532255328355,0.32159861761589));
#36862=CARTESIAN_POINT('Ctrl Pts',(22.1219736866861,-3.89986016195786,0.639185244649252));
#36863=CARTESIAN_POINT('Ctrl Pts',(22.1058787690116,-3.82372336883648,0.94670144792028));
#36864=CARTESIAN_POINT('Ctrl Pts',(22.0404303371608,-3.51412043598972,2.19718645690713));
#36865=CARTESIAN_POINT('Ctrl Pts',(21.97498190531,-2.5319402955714,3.2811505782075));
#36866=CARTESIAN_POINT('Ctrl Pts',(21.9095334734592,-1.31793994286403,3.71216087310869));
#36867=CARTESIAN_POINT('Ctrl Pts',(21.8440850416085,-0.103939590156664,
4.14317116800988));
#36868=CARTESIAN_POINT('Ctrl Pts',(21.7786366097577,1.34188097483974,3.92122763651189));
#36869=CARTESIAN_POINT('Ctrl Pts',(21.7131881779069,2.3707043932351,3.14592827253841));
#36870=CARTESIAN_POINT('Ctrl Pts',(21.6477397460562,3.39952781163046,2.37062890856494));
#36871=CARTESIAN_POINT('Ctrl Pts',(21.5822913142054,4.01135408342477,1.04197371211599));
#36872=CARTESIAN_POINT('Ctrl Pts',(21.5168428823546,3.93162388784021,-0.24379836679225));
#36873=CARTESIAN_POINT('Ctrl Pts',(21.4513944505038,3.85189369225565,-1.52957044570049));
#36874=CARTESIAN_POINT('Ctrl Pts',(21.3859460186531,3.08060702929222,-2.77245940706802));
#36875=CARTESIAN_POINT('Ctrl Pts',(21.3204975868023,1.96388166738833,-3.41471417252903));
#36876=CARTESIAN_POINT('Ctrl Pts',(21.2550491549515,0.84715630548443,-4.05696893799003));
#36877=CARTESIAN_POINT('Ctrl Pts',(21.1896007231007,-0.615007755359946,
-4.09858950754451));
#36878=CARTESIAN_POINT('Ctrl Pts',(21.1241522912499,-1.76645896380458,-3.52089855434547));
#36879=CARTESIAN_POINT('Ctrl Pts',(21.0587038593992,-2.91791017224922,-2.94320760114644));
#36880=CARTESIAN_POINT('Ctrl Pts',(20.9932554275484,-3.75864852829412,-1.74620512519392));
#36881=CARTESIAN_POINT('Ctrl Pts',(20.9278069956976,-3.91138953753916,-0.467050329322068));
#36882=CARTESIAN_POINT('Ctrl Pts',(20.9199258378101,-3.92978227783443,-0.313017289510358));
#36883=CARTESIAN_POINT('Ctrl Pts',(20.9120446799225,-3.93819874504042,-0.157793003857012));
#36884=CARTESIAN_POINT('Ctrl Pts',(20.904163522035,-3.93705835258154,-0.00244415858371427));
#36885=CARTESIAN_POINT('Ctrl Pts',(20.720836477965,-3.93634147379978,-0.00275764000347982));
#36886=CARTESIAN_POINT('Ctrl Pts',(20.7301690312209,-3.93781583666231,-0.186803452894212));
#36887=CARTESIAN_POINT('Ctrl Pts',(20.7395015844767,-3.92599851426311,-0.370659122854381));
#36888=CARTESIAN_POINT('Ctrl Pts',(20.7488341377326,-3.90023200959619,-0.552538626230935));
#36889=CARTESIAN_POINT('Ctrl Pts',(20.8142825695833,-3.71953362208168,-1.8280446914475));
#36890=CARTESIAN_POINT('Ctrl Pts',(20.8797310014341,-2.8528002143385,-3.00636086723926));
#36891=CARTESIAN_POINT('Ctrl Pts',(20.9451794332849,-1.68898196160953,-3.55871417944791));
#36892=CARTESIAN_POINT('Ctrl Pts',(21.0106278651357,-0.525163708880573,
-4.11106749165656));
#36893=CARTESIAN_POINT('Ctrl Pts',(21.0760762969865,0.935739388834165,-4.0374579402821));
#36894=CARTESIAN_POINT('Ctrl Pts',(21.1415247288372,2.03814179849579,-3.37091767673898));
#36895=CARTESIAN_POINT('Ctrl Pts',(21.206973160688,3.14054420815743,-2.70437741319586));
#36896=CARTESIAN_POINT('Ctrl Pts',(21.2724215925388,3.88444592976595,-1.44490643748405));
#36897=CARTESIAN_POINT('Ctrl Pts',(21.3378700243896,3.936018208958,-0.157697248386007));
#36898=CARTESIAN_POINT('Ctrl Pts',(21.4033184562403,3.98759048815004,1.12951194071202));
#36899=CARTESIAN_POINT('Ctrl Pts',(21.4687668880911,3.34683332492562,2.44445934319629));
#36900=CARTESIAN_POINT('Ctrl Pts',(21.5342153199419,2.30128892652022,3.19705752490842));
#36901=CARTESIAN_POINT('Ctrl Pts',(21.5996637517926,1.25574452811482,3.94965570662055));
#36902=CARTESIAN_POINT('Ctrl Pts',(21.6651121836434,-0.194587105471541,
4.13990466756053));
#36903=CARTESIAN_POINT('Ctrl Pts',(21.7305606154942,-1.3988642776945,3.68242942294792));
#36904=CARTESIAN_POINT('Ctrl Pts',(21.796009047345,-2.60314144991746,3.22495417833531));
#36905=CARTESIAN_POINT('Ctrl Pts',(21.8614574791958,-3.561364160777,2.11975472817009));
#36906=CARTESIAN_POINT('Ctrl Pts',(21.9269059110465,-3.84352638982112,0.862793468370925));
#36907=CARTESIAN_POINT('Ctrl Pts',(21.9415494333527,-3.90665775566324,0.581559224473073));
#36908=CARTESIAN_POINT('Ctrl Pts',(21.9561929556589,-3.93594539582555,0.292727753415705));
#36909=CARTESIAN_POINT('Ctrl Pts',(21.970836477965,-3.93336915469688,0.00337969667030601));
#36910=CARTESIAN_POINT('Origin',(23.75,0.,0.));
#36911=CARTESIAN_POINT('',(23.404163522035,-3.92812465671341,-0.00212229078741105));
#36912=CARTESIAN_POINT('',(23.220836477965,-3.92768863108871,-0.00174943043258178));
#36913=CARTESIAN_POINT('',(23.75,-3.933,-4.81653586104654E-16));
#36914=CARTESIAN_POINT('Ctrl Pts',(23.404163522035,-3.92812465671341,-0.00212229078741105));
#36915=CARTESIAN_POINT('Ctrl Pts',(23.3640925287985,-3.92414083826686,0.792347133215219));
#36916=CARTESIAN_POINT('Ctrl Pts',(23.324021535562,-3.68976240124988,1.58897831133289));
#36917=CARTESIAN_POINT('Ctrl Pts',(23.2839505423256,-3.24164538944974,2.23804361037454));
#36918=CARTESIAN_POINT('Ctrl Pts',(23.2185021104748,-2.5097305218822,3.29816971556831));
#36919=CARTESIAN_POINT('Ctrl Pts',(23.153053678624,-1.20762356863968,3.96463315855812));
#36920=CARTESIAN_POINT('Ctrl Pts',(23.0876052467732,0.0803501277369667,
3.93835598823379));
#36921=CARTESIAN_POINT('Ctrl Pts',(23.0221568149224,1.3683238241136,3.91207881790945));
#36922=CARTESIAN_POINT('Ctrl Pts',(22.9567083830717,2.64216426362435,3.19306103427099));
#36923=CARTESIAN_POINT('Ctrl Pts',(22.8912599512209,3.33023080703671,2.10396454450698));
#36924=CARTESIAN_POINT('Ctrl Pts',(22.8258115193701,4.01829735044907,1.01486805474297));
#36925=CARTESIAN_POINT('Ctrl Pts',(22.7603630875193,4.12058999776305,-0.444307141146586));
#36926=CARTESIAN_POINT('Ctrl Pts',(22.6949146556685,3.59120454263221,-1.61875074232297));
#36927=CARTESIAN_POINT('Ctrl Pts',(22.6294662238178,3.06181908750136,-2.79319434349935));
#36928=CARTESIAN_POINT('Ctrl Pts',(22.564017791967,1.90075552992569,-3.68290634996255));
#36929=CARTESIAN_POINT('Ctrl Pts',(22.4985693601163,0.62904546370725,-3.88862518619208));
#36930=CARTESIAN_POINT('Ctrl Pts',(22.4331209282655,-0.642664602511191,
-4.0943440224216));
#36931=CARTESIAN_POINT('Ctrl Pts',(22.3676724964147,-2.02502117737241,-3.61606968841744));
#36932=CARTESIAN_POINT('Ctrl Pts',(22.3022240645639,-2.89768660216542,-2.66842957307869));
#36933=CARTESIAN_POINT('Ctrl Pts',(22.2528705503876,-3.55574828822536,-1.95383078829727));
#36934=CARTESIAN_POINT('Ctrl Pts',(22.2035170362113,-3.92397902073757,-0.972331681725521));
#36935=CARTESIAN_POINT('Ctrl Pts',(22.154163522035,-3.93253297961002,0.00339845520594975));
#36936=CARTESIAN_POINT('Ctrl Pts',(21.970836477965,-3.93336915469688,0.00337969667030601));
#36937=CARTESIAN_POINT('Ctrl Pts',(22.0216413875096,-3.92443102527893,-1.00049775456773));
#36938=CARTESIAN_POINT('Ctrl Pts',(22.0724462970542,-3.53194559205172,-2.01059337634254));
#36939=CARTESIAN_POINT('Ctrl Pts',(22.1232512065988,-2.83859494485778,-2.73120603295504));
#36940=CARTESIAN_POINT('Ctrl Pts',(22.1886996384496,-1.94539952362163,-3.65952120504872));
#36941=CARTESIAN_POINT('Ctrl Pts',(22.2541480703004,-0.55290693392065,-4.10742847980296));
#36942=CARTESIAN_POINT('Ctrl Pts',(22.3195965021512,0.713996594007594,-3.8739277927898));
#36943=CARTESIAN_POINT('Ctrl Pts',(22.385044934002,1.98090012193584,-3.64042710577664));
#36944=CARTESIAN_POINT('Ctrl Pts',(22.4504933658528,3.12221458809134,-2.72551845699607));
#36945=CARTESIAN_POINT('Ctrl Pts',(22.5159417977035,3.62577087549378,-1.53977051229877));
#36946=CARTESIAN_POINT('Ctrl Pts',(22.5813902295543,4.12932716289623,-0.35402256760147));
#36947=CARTESIAN_POINT('Ctrl Pts',(22.646838661405,3.99512527154563,1.10256467301257));
#36948=CARTESIAN_POINT('Ctrl Pts',(22.7122870932558,3.28338880059249,2.17634226495933));
#36949=CARTESIAN_POINT('Ctrl Pts',(22.7777355251066,2.57165232963934,3.25011985690608));
#36950=CARTESIAN_POINT('Ctrl Pts',(22.8431839569574,1.28238127908365,3.94108780018556));
#36951=CARTESIAN_POINT('Ctrl Pts',(22.9086323888082,-0.00585916808317544,
3.93917165702054));
#36952=CARTESIAN_POINT('Ctrl Pts',(22.974080820659,-1.29409961525001,3.93725551385553));
#36953=CARTESIAN_POINT('Ctrl Pts',(23.0395292525097,-2.58130945902797,3.24245528424603));
#36954=CARTESIAN_POINT('Ctrl Pts',(23.1049776843605,-3.28984849000153,2.16656515823267));
#36955=CARTESIAN_POINT('Ctrl Pts',(23.1435972822287,-3.7079408976622,1.53170741081231));
#36956=CARTESIAN_POINT('Ctrl Pts',(23.1822168800969,-3.92454558560357,0.764157755427278));
#36957=CARTESIAN_POINT('Ctrl Pts',(23.220836477965,-3.92768863108871,-0.00174943043258178));
#36958=CARTESIAN_POINT('Origin',(23.75,0.,0.));
#36959=CARTESIAN_POINT('',(24.654163522035,-3.93909475595853,-0.000490377207084114));
#36960=CARTESIAN_POINT('',(24.470836477965,-3.93885420654145,-0.000985259163277196));
#36961=CARTESIAN_POINT('',(23.75,-3.933,-4.81653586104654E-16));
#36962=CARTESIAN_POINT('Ctrl Pts',(24.654163522035,-3.93909475595853,-0.000490377207084114));
#36963=CARTESIAN_POINT('Ctrl Pts',(24.5901164532365,-3.93683716814358,1.26023770975936));
#36964=CARTESIAN_POINT('Ctrl Pts',(24.526069384438,-3.27732068913603,2.52300066969272));
#36965=CARTESIAN_POINT('Ctrl Pts',(24.4620223156395,-2.24041894240288,3.24000416594111));
#36966=CARTESIAN_POINT('Ctrl Pts',(24.3965738837887,-1.18082957195824,3.9726958463149));
#36967=CARTESIAN_POINT('Ctrl Pts',(24.331125451938,0.272840271641166,4.13548412538781));
#36968=CARTESIAN_POINT('Ctrl Pts',(24.2656770200872,1.46825083487448,3.6553171570425));
#36969=CARTESIAN_POINT('Ctrl Pts',(24.2002285882364,2.6636613981078,3.17515018869718));
#36970=CARTESIAN_POINT('Ctrl Pts',(24.1347801563856,3.60081268097502,2.05202797293364));
#36971=CARTESIAN_POINT('Ctrl Pts',(24.0693317245348,3.85915455648697,0.789955784984271));
#36972=CARTESIAN_POINT('Ctrl Pts',(24.0038832926841,4.11749643199892,-0.472116402965099));
#36973=CARTESIAN_POINT('Ctrl Pts',(23.9384348608333,3.69702890015558,-1.8731385631003));
#36974=CARTESIAN_POINT('Ctrl Pts',(23.8729864289825,2.78643833118525,-2.7843967855499));
#36975=CARTESIAN_POINT('Ctrl Pts',(23.8075379971318,1.87584776221493,-3.6956550079995));
#36976=CARTESIAN_POINT('Ctrl Pts',(23.742089565281,0.475134156117602,-4.11714929276351));
#36977=CARTESIAN_POINT('Ctrl Pts',(23.6766411334302,-0.787127042068175,
-3.85973251049337));
#36978=CARTESIAN_POINT('Ctrl Pts',(23.6111927015794,-2.04938824025396,-3.60231572822324));
#36979=CARTESIAN_POINT('Ctrl Pts',(23.5457442697286,-3.1731970305282,-2.66598787891895));
#36980=CARTESIAN_POINT('Ctrl Pts',(23.4802958378779,-3.65424003471902,-1.47092957056794));
#36981=CARTESIAN_POINT('Ctrl Pts',(23.4549183992636,-3.84076305695926,-1.00754919607961));
#36982=CARTESIAN_POINT('Ctrl Pts',(23.4295409606493,-3.9306476565173,-0.505269265946798));
#36983=CARTESIAN_POINT('Ctrl Pts',(23.404163522035,-3.92812465671341,-0.00212229078741105));
#36984=CARTESIAN_POINT('Ctrl Pts',(23.220836477965,-3.92768863108871,-0.00174943043258178));
#36985=CARTESIAN_POINT('Ctrl Pts',(23.2476653119476,-3.92987208845688,-0.533821173013996));
#36986=CARTESIAN_POINT('Ctrl Pts',(23.2744941459302,-3.8290387712291,-1.06510025837181));
#36987=CARTESIAN_POINT('Ctrl Pts',(23.3013229799128,-3.62117429826454,-1.55054970043114));
#36988=CARTESIAN_POINT('Ctrl Pts',(23.3667714117636,-3.11409285738485,-2.73479441066429));
#36989=CARTESIAN_POINT('Ctrl Pts',(23.4322198436144,-1.97006175745636,-3.64630380871338));
#36990=CARTESIAN_POINT('Ctrl Pts',(23.4976682754651,-0.702469213319956,
-3.87603465885666));
#36991=CARTESIAN_POINT('Ctrl Pts',(23.5631167073159,0.565123330816479,-4.10576550899994));
#36992=CARTESIAN_POINT('Ctrl Pts',(23.6285651391667,1.95627731916084,-3.65371781123739));
#36993=CARTESIAN_POINT('Ctrl Pts',(23.6940135710175,2.8467072206701,-2.72274965281462));
#36994=CARTESIAN_POINT('Ctrl Pts',(23.7594620028682,3.73713712217935,-1.79178149439185));
#36995=CARTESIAN_POINT('Ctrl Pts',(23.824910434719,4.12684293685351,-0.381892875308882));
#36996=CARTESIAN_POINT('Ctrl Pts',(23.8903588665698,3.84094272963275,0.874223438163058));
#36997=CARTESIAN_POINT('Ctrl Pts',(23.9558072984206,3.55504252241199,2.13033975163501));
#36998=CARTESIAN_POINT('Ctrl Pts',(24.0212557302713,2.59353629329628,3.23268375949592));
#36999=CARTESIAN_POINT('Ctrl Pts',(24.0867041621221,1.38790354194334,3.68657448458775));
#37000=CARTESIAN_POINT('Ctrl Pts',(24.1521525939729,0.182270790590404,4.14046520967958));
#37001=CARTESIAN_POINT('Ctrl Pts',(24.2176010258237,-1.26748848299976,3.94590265200234));
#37002=CARTESIAN_POINT('Ctrl Pts',(24.2830494576745,-2.31078940792255,3.19019748359728));
#37003=CARTESIAN_POINT('Ctrl Pts',(24.3456451311047,-3.30861505689732,2.46743190169848));
#37004=CARTESIAN_POINT('Ctrl Pts',(24.4082408045348,-3.93464344142654,1.2313756263831));
#37005=CARTESIAN_POINT('Ctrl Pts',(24.470836477965,-3.93885420654145,-0.000985259163277196));
#37006=CARTESIAN_POINT('Origin',(23.75,0.,0.));
#37007=CARTESIAN_POINT('',(25.904163522035,-3.92919769550165,0.00273228871909281));
#37008=CARTESIAN_POINT('',(25.720836477965,-3.92985825803548,0.00297976440258395));
#37009=CARTESIAN_POINT('',(23.75,-3.933,-4.81653586104654E-16));
#37010=CARTESIAN_POINT('Ctrl Pts',(25.904163522035,-3.92919769550165,0.00273228871909281));
#37011=CARTESIAN_POINT('Ctrl Pts',(25.8815888095252,-3.93213961178236,0.450002964145652));
#37012=CARTESIAN_POINT('Ctrl Pts',(25.8590140970155,-3.8614845501863,0.896372500728469));
#37013=CARTESIAN_POINT('Ctrl Pts',(25.8364393845058,-3.71312585452063,1.31521879246953));
#37014=CARTESIAN_POINT('Ctrl Pts',(25.770990952655,-3.28300547187737,2.52953472092949));
#37015=CARTESIAN_POINT('Ctrl Pts',(25.7055425208042,-2.19976150773091,3.51250908524159));
#37016=CARTESIAN_POINT('Ctrl Pts',(25.6400940889535,-0.949503751846705,
3.82302846763078));
#37017=CARTESIAN_POINT('Ctrl Pts',(25.5746456571027,0.300754004037498,4.13354785001997));
#37018=CARTESIAN_POINT('Ctrl Pts',(25.5091972252519,1.71802555165944,3.77161225048626));
#37019=CARTESIAN_POINT('Ctrl Pts',(25.4437487934011,2.66630502260462,2.89964162311381));
#37020=CARTESIAN_POINT('Ctrl Pts',(25.3783003615503,3.61458449354981,2.02767099574135));
#37021=CARTESIAN_POINT('Ctrl Pts',(25.3128519296996,4.09387188781823,0.645665340530145));
#37022=CARTESIAN_POINT('Ctrl Pts',(25.2474034978488,3.88908519554681,-0.626195163358931));
#37023=CARTESIAN_POINT('Ctrl Pts',(25.181955065998,3.6842985032754,-1.898055667248));
#37024=CARTESIAN_POINT('Ctrl Pts',(25.1165066341473,2.79543772446416,-3.05977101981493));
#37025=CARTESIAN_POINT('Ctrl Pts',(25.0510582022965,1.62138244634291,-3.59001713026159));
#37026=CARTESIAN_POINT('Ctrl Pts',(24.9856097704457,0.447327168221664,-4.12026324070824));
#37027=CARTESIAN_POINT('Ctrl Pts',(24.9201613385949,-1.0119226092096,-4.01904010903461));
#37028=CARTESIAN_POINT('Ctrl Pts',(24.8547129067441,-2.1015231180563,-3.33177199326797));
#37029=CARTESIAN_POINT('Ctrl Pts',(24.7892644748934,-3.191123626903,-2.64450387750133));
#37030=CARTESIAN_POINT('Ctrl Pts',(24.7238160430426,-3.91107486716513,-1.37119077764169));
#37031=CARTESIAN_POINT('Ctrl Pts',(24.6583676111918,-3.93829603865126,-0.0832366868745308));
#37032=CARTESIAN_POINT('Ctrl Pts',(24.6569662481396,-3.93887889056813,-0.0556593832661226));
#37033=CARTESIAN_POINT('Ctrl Pts',(24.6555648850873,-3.93914415244474,-0.0280753673276151));
#37034=CARTESIAN_POINT('Ctrl Pts',(24.654163522035,-3.93909475595853,-0.000490377207084114));
#37035=CARTESIAN_POINT('Ctrl Pts',(24.470836477965,-3.93885420654145,-0.000985259163277196));
#37036=CARTESIAN_POINT('Ctrl Pts',(24.4736892363856,-3.93904610951143,-0.0571493309080139));
#37037=CARTESIAN_POINT('Ctrl Pts',(24.4765419948062,-3.93794648282358,-0.113305727242253));
#37038=CARTESIAN_POINT('Ctrl Pts',(24.4793947532268,-3.9355316597942,-0.16940551076599));
#37039=CARTESIAN_POINT('Ctrl Pts',(24.5448431850775,-3.88013041048765,-1.45645555759133));
#37040=CARTESIAN_POINT('Ctrl Pts',(24.6102916169283,-3.13248533561915,-2.71370787210913));
#37041=CARTESIAN_POINT('Ctrl Pts',(24.6757400487791,-2.02810494588332,-3.37696579793198));
#37042=CARTESIAN_POINT('Ctrl Pts',(24.7411884806299,-0.923724556147519,
-4.04022372375482));
#37043=CARTESIAN_POINT('Ctrl Pts',(24.8066369124807,0.537391148455583,-4.10948726088273));
#37044=CARTESIAN_POINT('Ctrl Pts',(24.8720853443314,1.69956105657403,-3.55367413911433));
#37045=CARTESIAN_POINT('Ctrl Pts',(24.9375337761822,2.8617309646925,-2.99786101734593));
#37046=CARTESIAN_POINT('Ctrl Pts',(25.002982208033,3.7249550763263,-1.81697123668122));
#37047=CARTESIAN_POINT('Ctrl Pts',(25.0684306398838,3.90185835737233,-0.540933482350884));
#37048=CARTESIAN_POINT('Ctrl Pts',(25.1338790717345,4.07876163841836,0.735104271979422));
#37049=CARTESIAN_POINT('Ctrl Pts',(25.1993275035853,3.56934408887662,2.10628999997535));
#37050=CARTESIAN_POINT('Ctrl Pts',(25.2647759354361,2.60220873153787,2.95729900206465));
#37051=CARTESIAN_POINT('Ctrl Pts',(25.3302243672869,1.63507337419909,3.80830800415396));
#37052=CARTESIAN_POINT('Ctrl Pts',(25.3956727991376,0.21022020906327,4.13914028033664));
#37053=CARTESIAN_POINT('Ctrl Pts',(25.4611212309884,-1.0329426038841,3.80133361456278));
#37054=CARTESIAN_POINT('Ctrl Pts',(25.5265696628392,-2.27610541683143,3.46352694878893));
#37055=CARTESIAN_POINT('Ctrl Pts',(25.59201809469,-3.3375778775903,2.45708134105862));
#37056=CARTESIAN_POINT('Ctrl Pts',(25.6574665265407,-3.74102026390006,1.2336430055299));
#37057=CARTESIAN_POINT('Ctrl Pts',(25.6785898436822,-3.87123028167017,0.838781352873692));
#37058=CARTESIAN_POINT('Ctrl Pts',(25.6997131608236,-3.93289597643157,0.421316448174291));
#37059=CARTESIAN_POINT('Ctrl Pts',(25.720836477965,-3.92985825803548,0.00297976440258395));
#37060=CARTESIAN_POINT('Origin',(23.75,0.,0.));
#37061=CARTESIAN_POINT('',(27.154163522035,-3.93098047339281,-0.00325343987953419));
#37062=CARTESIAN_POINT('',(26.970836477965,-3.93023513714109,-0.00309016900265477));
#37063=CARTESIAN_POINT('',(23.75,-3.933,-4.81653586104654E-16));
#37064=CARTESIAN_POINT('Ctrl Pts',(27.154163522035,-3.93098047339281,-0.00325343987953419));
#37065=CARTESIAN_POINT('Ctrl Pts',(27.1076127339632,-3.92351105440917,0.917992942990856));
#37066=CARTESIAN_POINT('Ctrl Pts',(27.0610619458915,-3.59950298381568,1.84397406686046));
#37067=CARTESIAN_POINT('Ctrl Pts',(27.0145111578198,-3.00784466327321,2.54361478474492));
#37068=CARTESIAN_POINT('Ctrl Pts',(26.949062725969,-2.17599818172083,3.52727993288205));
#37069=CARTESIAN_POINT('Ctrl Pts',(26.8836142941182,-0.815083000998221,
4.06353423725179));
#37070=CARTESIAN_POINT('Ctrl Pts',(26.8181658622674,0.464183581722977,3.9117308993607));
#37071=CARTESIAN_POINT('Ctrl Pts',(26.7527174304166,1.74345016444418,3.75992756146961));
#37072=CARTESIAN_POINT('Ctrl Pts',(26.6872689985659,2.94106814916398,2.92006658131768));
#37073=CARTESIAN_POINT('Ctrl Pts',(26.6218205667151,3.51960279979861,1.76903905110911));
#37074=CARTESIAN_POINT('Ctrl Pts',(26.5563721348643,4.09813745043322,0.618011520900572));
#37075=CARTESIAN_POINT('Ctrl Pts',(26.4909237030135,4.0575887669827,-0.84418255936459));
#37076=CARTESIAN_POINT('Ctrl Pts',(26.4254752711628,3.41615271487111,-1.96137833317676));
#37077=CARTESIAN_POINT('Ctrl Pts',(26.360026839312,2.77471666275951,-3.07857410698896));
#37078=CARTESIAN_POINT('Ctrl Pts',(26.2945784074612,1.53239324198682,-3.85077157434815));
#37079=CARTESIAN_POINT('Ctrl Pts',(26.2291299756104,0.246679921490786,-3.93144415461087));
#37080=CARTESIAN_POINT('Ctrl Pts',(26.1636815437597,-1.03903339900524,-4.01211673487358));
#37081=CARTESIAN_POINT('Ctrl Pts',(26.0982331119089,-2.3681366192246,-3.40126442803983));
#37082=CARTESIAN_POINT('Ctrl Pts',(26.0327846800581,-3.14418982876426,-2.37300952831905));
#37083=CARTESIAN_POINT('Ctrl Pts',(25.9899109607171,-3.65256392664006,-1.69942406973689));
#37084=CARTESIAN_POINT('Ctrl Pts',(25.947037241376,-3.92361043086253,-0.84672071757979));
#37085=CARTESIAN_POINT('Ctrl Pts',(25.904163522035,-3.92919769550165,0.00273228871909281));
#37086=CARTESIAN_POINT('Ctrl Pts',(25.720836477965,-3.92985825803548,0.00297976440258395));
#37087=CARTESIAN_POINT('Ctrl Pts',(25.7651615926744,-3.92348391751595,-0.874856863772733));
#37088=CARTESIAN_POINT('Ctrl Pts',(25.8094867073837,-3.63220286020098,-1.75653217218374));
#37089=CARTESIAN_POINT('Ctrl Pts',(25.8538118220931,-3.09150438011423,-2.44125138467072));
#37090=CARTESIAN_POINT('Ctrl Pts',(25.9192602539439,-2.29313379815808,-3.4522763760154));
#37091=CARTESIAN_POINT('Ctrl Pts',(25.9847086857946,-0.950980322385189,
-4.03389529537762));
#37092=CARTESIAN_POINT('Ctrl Pts',(26.0501571176454,0.332659693891018,-3.92510448349789));
#37093=CARTESIAN_POINT('Ctrl Pts',(26.1156055494962,1.61629971016724,-3.81631367161816));
#37094=CARTESIAN_POINT('Ctrl Pts',(26.1810539813469,2.84142626694679,-3.01711312849645));
#37095=CARTESIAN_POINT('Ctrl Pts',(26.2465024131977,3.45825923142778,-1.8861470808627));
#37096=CARTESIAN_POINT('Ctrl Pts',(26.3119508450485,4.07509219590877,-0.755181033228954));
#37097=CARTESIAN_POINT('Ctrl Pts',(26.3773992768993,4.08363156809121,0.707550518916832));
#37098=CARTESIAN_POINT('Ctrl Pts',(26.44284770875,3.48004533087329,1.84564136168573));
#37099=CARTESIAN_POINT('Ctrl Pts',(26.5082961406008,2.87645909365536,2.98373220445462));
#37100=CARTESIAN_POINT('Ctrl Pts',(26.5737445724516,1.66074724703709,3.79718233784663));
#37101=CARTESIAN_POINT('Ctrl Pts',(26.6391930043024,0.378464894959196,3.92095295644834));
#37102=CARTESIAN_POINT('Ctrl Pts',(26.7046414361532,-0.903817457118713,
4.04472357505004));
#37103=CARTESIAN_POINT('Ctrl Pts',(26.7700898680039,-2.25267031465624,3.47881467886142));
#37104=CARTESIAN_POINT('Ctrl Pts',(26.8355382998547,-3.06279071672218,2.4771800499131));
#37105=CARTESIAN_POINT('Ctrl Pts',(26.8806376925581,-3.6210308015747,1.78697079357367));
#37106=CARTESIAN_POINT('Ctrl Pts',(26.9257370852616,-3.92346175853291,0.889863626098021));
#37107=CARTESIAN_POINT('Ctrl Pts',(26.970836477965,-3.93023513714109,-0.00309016900265477));
#37108=CARTESIAN_POINT('Origin',(23.75,0.,0.));
#37109=CARTESIAN_POINT('',(28.404163522035,-3.93818417569795,0.00170700930730246));
#37110=CARTESIAN_POINT('',(28.220836477965,-3.93866152695812,0.00124115044389661));
#37111=CARTESIAN_POINT('',(23.75,-3.933,-4.81653586104654E-16));
#37112=CARTESIAN_POINT('Ctrl Pts',(28.404163522035,-3.93818417569795,0.00170700930730246));
#37113=CARTESIAN_POINT('Ctrl Pts',(28.399085090252,-3.9387267147927,0.101734442167589));
#37114=CARTESIAN_POINT('Ctrl Pts',(28.394006658469,-3.93523450213126,0.201722834433012));
#37115=CARTESIAN_POINT('Ctrl Pts',(28.388928226686,-3.92758354814724,0.301391698975487));
#37116=CARTESIAN_POINT('Ctrl Pts',(28.3234797948353,-3.82898166437366,1.58587698250684));
#37117=CARTESIAN_POINT('Ctrl Pts',(28.2580313629845,-3.03966117892474,2.81729242473998));
#37118=CARTESIAN_POINT('Ctrl Pts',(28.1925829311337,-1.91366888952096,3.44310820754633));
#37119=CARTESIAN_POINT('Ctrl Pts',(28.1271344992829,-0.787676600117176,
4.06892399035268));
#37120=CARTESIAN_POINT('Ctrl Pts',(28.0616860674322,0.674987493241486,4.08914011373224));
#37121=CARTESIAN_POINT('Ctrl Pts',(27.9962376355814,1.81786335315111,3.49464730782801));
#37122=CARTESIAN_POINT('Ctrl Pts',(27.9307892037306,2.96073921306072,2.90015450192379));
#37123=CARTESIAN_POINT('Ctrl Pts',(27.8653407718798,3.7838268395213,1.69095276673577));
#37124=CARTESIAN_POINT('Ctrl Pts',(27.7998923400291,3.91780578128033,0.409694993734216));
#37125=CARTESIAN_POINT('Ctrl Pts',(27.7344439081783,4.05178472303937,-0.871562779267352));
#37126=CARTESIAN_POINT('Ctrl Pts',(27.6689954763275,3.49665498009686,-2.22487659008246));
#37127=CARTESIAN_POINT('Ctrl Pts',(27.6035470444767,2.50151091037662,-3.04295164422803));
#37128=CARTESIAN_POINT('Ctrl Pts',(27.538098612626,1.50636684065638,-3.86102669837359));
#37129=CARTESIAN_POINT('Ctrl Pts',(27.4726501807752,0.0712084441584163,
-4.14386299584961));
#37130=CARTESIAN_POINT('Ctrl Pts',(27.4072017489244,-1.15992021363229,-3.76453165356687));
#37131=CARTESIAN_POINT('Ctrl Pts',(27.3417533170736,-2.39104887142302,-3.38520031128414));
#37132=CARTESIAN_POINT('Ctrl Pts',(27.2763048852229,-3.41814779050649,-2.34370132924263));
#37133=CARTESIAN_POINT('Ctrl Pts',(27.2108564533721,-3.78030835885712,-1.10741384226963));
#37134=CARTESIAN_POINT('Ctrl Pts',(27.191958809593,-3.88487895310921,-0.750446992543413));
#37135=CARTESIAN_POINT('Ctrl Pts',(27.173061165814,-3.93401274040774,-0.377240362493561));
#37136=CARTESIAN_POINT('Ctrl Pts',(27.154163522035,-3.93098047339281,-0.00325343987953419));
#37137=CARTESIAN_POINT('Ctrl Pts',(26.970836477965,-3.93023513714109,-0.00309016900265477));
#37138=CARTESIAN_POINT('Ctrl Pts',(26.9911855171124,-3.9332913145793,-0.405994745850263));
#37139=CARTESIAN_POINT('Ctrl Pts',(27.0115345562597,-3.87615595376113,-0.808053757116241));
#37140=CARTESIAN_POINT('Ctrl Pts',(27.031883595407,-3.75516863334752,-1.18988033548289));
#37141=CARTESIAN_POINT('Ctrl Pts',(27.0973320272578,-3.36603820131256,-2.41794573022264));
#37142=CARTESIAN_POINT('Ctrl Pts',(27.1627804591086,-2.31638939064824,-3.43671615799411));
#37143=CARTESIAN_POINT('Ctrl Pts',(27.2282288909594,-1.07725517871138,-3.789014376074));
#37144=CARTESIAN_POINT('Ctrl Pts',(27.2936773228101,0.161879033225451,-4.14131259415387));
#37145=CARTESIAN_POINT('Ctrl Pts',(27.3591257546609,1.59049864643482,-3.82713860254219));
#37146=CARTESIAN_POINT('Ctrl Pts',(27.4245741865117,2.56750366718156,-2.98747957947988));
#37147=CARTESIAN_POINT('Ctrl Pts',(27.4900226183624,3.54450868792831,-2.14782055641755));
#37148=CARTESIAN_POINT('Ctrl Pts',(27.5554710502132,4.06989911621242,-0.782676501904576));
#37149=CARTESIAN_POINT('Ctrl Pts',(27.620919482064,3.90790720462131,0.49533994505792));
#37150=CARTESIAN_POINT('Ctrl Pts',(27.6863679139148,3.74591529303021,1.7733563920204));
#37151=CARTESIAN_POINT('Ctrl Pts',(27.7518163457656,2.8965410415639,2.9642452314324));
#37152=CARTESIAN_POINT('Ctrl Pts',(27.8172647776163,1.74093814691504,3.53358903245858));
#37153=CARTESIAN_POINT('Ctrl Pts',(27.8827132094671,0.585335252266155,4.10293283348478));
#37154=CARTESIAN_POINT('Ctrl Pts',(27.9481616413179,-0.876496285565295,
4.05073159612515));
#37155=CARTESIAN_POINT('Ctrl Pts',(28.0136100731687,-1.98854212366733,3.40041399637644));
#37156=CARTESIAN_POINT('Ctrl Pts',(28.0790585050194,-3.10058796176937,2.75009639662773));
#37157=CARTESIAN_POINT('Ctrl Pts',(28.1445069368702,-3.862848100142,1.50166243448994));
#37158=CARTESIAN_POINT('Ctrl Pts',(28.209955368721,-3.93327883257213,0.215345311481923));
#37159=CARTESIAN_POINT('Ctrl Pts',(28.2135824051357,-3.93718197927882,0.144059890058629));
#37160=CARTESIAN_POINT('Ctrl Pts',(28.2172094415504,-3.93896039300732,0.0726581226105382));
#37161=CARTESIAN_POINT('Ctrl Pts',(28.220836477965,-3.93866152695812,0.00124115044389661));
#37162=CARTESIAN_POINT('Origin',(23.75,0.,0.));
#37163=CARTESIAN_POINT('',(29.567,-3.933,-4.81653586104654E-16));
#37164=CARTESIAN_POINT('',(29.470836477965,-3.9278981228736,0.00143380487199485));
#37165=CARTESIAN_POINT('',(23.75,-3.933,-4.81653586104654E-16));
#37166=CARTESIAN_POINT('',(29.567,-3.56151197810526,1.66856867698419));
#37167=CARTESIAN_POINT('Origin',(29.567,0.,0.));
#37168=CARTESIAN_POINT('Ctrl Pts',(29.567,-3.56151197810523,1.66856867698424));
#37169=CARTESIAN_POINT('Ctrl Pts',(29.5015515681492,-3.01258675481066,2.84023382017821));
#37170=CARTESIAN_POINT('Ctrl Pts',(29.4361031362984,-1.84538537124581,3.71044748004995));
#37171=CARTESIAN_POINT('Ctrl Pts',(29.3706547044477,-0.572813470363568,
3.89689459583817));
#37172=CARTESIAN_POINT('Ctrl Pts',(29.3052062725969,0.699758430518651,4.08334171162639));
#37173=CARTESIAN_POINT('Ctrl Pts',(29.2397578407461,2.07770084871824,3.58602228333111));
#37174=CARTESIAN_POINT('Ctrl Pts',(29.1743094088954,2.93709163106757,2.62598383516187));
#37175=CARTESIAN_POINT('Ctrl Pts',(29.1088609770446,3.79648241341692,1.66594538699262));
#37176=CARTESIAN_POINT('Ctrl Pts',(29.0434125451938,4.13732155991598,0.243187918949396));
#37177=CARTESIAN_POINT('Ctrl Pts',(28.977964113343,3.80910353312742,-1.00277003521058));
#37178=CARTESIAN_POINT('Ctrl Pts',(28.9125156814922,3.48088550633886,-2.24872798937053));
#37179=CARTESIAN_POINT('Ctrl Pts',(28.8470672496415,2.48361030626269,-3.31788642964727));
#37180=CARTESIAN_POINT('Ctrl Pts',(28.7816188177907,1.26359152250731,-3.73099214383412));
#37181=CARTESIAN_POINT('Ctrl Pts',(28.7161703859399,0.0435727387519015,
-4.14409785802099));
#37182=CARTESIAN_POINT('Ctrl Pts',(28.6507219540891,-1.39918962868272,-3.90115084611797));
#37183=CARTESIAN_POINT('Ctrl Pts',(28.5852735222384,-2.41662917135091,-3.11089977775168));
#37184=CARTESIAN_POINT('Ctrl Pts',(28.5249035221706,-3.35512110344034,-2.38196776667424));
#37185=CARTESIAN_POINT('Ctrl Pts',(28.4645335221028,-3.93173472701253,-1.1873719006031));
#37186=CARTESIAN_POINT('Ctrl Pts',(28.404163522035,-3.93818417569795,0.00170700930730246));
#37187=CARTESIAN_POINT('Ctrl Pts',(28.220836477965,-3.93866152695812,0.00124115044389661));
#37188=CARTESIAN_POINT('Ctrl Pts',(28.2826578734011,-3.93356747382553,-1.21603278132397));
#37189=CARTESIAN_POINT('Ctrl Pts',(28.3444792688372,-3.32498523962417,-2.4377239649422));
#37190=CARTESIAN_POINT('Ctrl Pts',(28.4063006642733,-2.34789226689304,-3.16300368438513));
#37191=CARTESIAN_POINT('Ctrl Pts',(28.4717490961241,-1.31347364229616,-3.93083527336599));
#37192=CARTESIAN_POINT('Ctrl Pts',(28.5371975279749,0.133964933385241,-4.14229816744944));
#37193=CARTESIAN_POINT('Ctrl Pts',(28.6026459598256,1.34479136791605,-3.70252107236144));
#37194=CARTESIAN_POINT('Ctrl Pts',(28.6680943916764,2.55561780244685,-3.26274397727345));
#37195=CARTESIAN_POINT('Ctrl Pts',(28.7335428235272,3.52983209582705,-2.17172689301403));
#37196=CARTESIAN_POINT('Ctrl Pts',(28.798991255378,3.83042460753331,-0.919022093761055));
#37197=CARTESIAN_POINT('Ctrl Pts',(28.8644396872287,4.13101711923956,0.333682705491934));
#37198=CARTESIAN_POINT('Ctrl Pts',(28.9298881190795,3.75798784927184,1.7480752197385));
#37199=CARTESIAN_POINT('Ctrl Pts',(28.9953365509303,2.87839874358939,2.68935253297113));
#37200=CARTESIAN_POINT('Ctrl Pts',(29.0607849827811,1.99880963790694,3.63062984620376));
#37201=CARTESIAN_POINT('Ctrl Pts',(29.1262334146319,0.612660696509772,4.09879195842248));
#37202=CARTESIAN_POINT('Ctrl Pts',(29.1916818464826,-0.657352822470509,
3.88392269629536));
#37203=CARTESIAN_POINT('Ctrl Pts',(29.2571302783334,-1.92736634145081,3.66905343416824));
#37204=CARTESIAN_POINT('Ctrl Pts',(29.3225787101841,-3.0812444380142,2.77115279769526));
#37205=CARTESIAN_POINT('Ctrl Pts',(29.3880271420349,-3.60246465164686,1.59281990421752));
#37206=CARTESIAN_POINT('Ctrl Pts',(29.4156302540116,-3.8222911549651,1.095853760267));
#37207=CARTESIAN_POINT('Ctrl Pts',(29.4432333659883,-3.92958294012511,0.54900541954638));
#37208=CARTESIAN_POINT('Ctrl Pts',(29.470836477965,-3.9278981228736,0.00143380487199485));
#37209=CARTESIAN_POINT('Origin',(15.6892265507269,0.,0.));
#37210=CARTESIAN_POINT('',(28.8142265507269,-3.2269979792094,0.00139874504058523));
#37211=CARTESIAN_POINT('',(29.0607734492731,-3.2185694572822,0.00117487786690768));
#37212=CARTESIAN_POINT('',(15.6892265507269,-3.22275,-1.83004677902795E-13));
#37213=CARTESIAN_POINT('',(29.567,2.58354504679088,1.93441189848628));
#37214=CARTESIAN_POINT('Ctrl Pts',(28.8142265507269,-3.2269979792094,0.00139874504058531));
#37215=CARTESIAN_POINT('Ctrl Pts',(28.8745965507947,-3.22171321929302,-0.972947569964154));
#37216=CARTESIAN_POINT('Ctrl Pts',(29.0004149827133,-2.23699797382901,-3.01302555875835));
#37217=CARTESIAN_POINT('Ctrl Pts',(29.1916818464826,1.21792180611816,-3.59480011557272));
#37218=CARTESIAN_POINT('Ctrl Pts',(29.3822363295059,3.5971583139091,-1.04406909014969));
#37219=CARTESIAN_POINT('Ctrl Pts',(29.5073423806783,3.15601612891197,1.15992870617642));
#37220=CARTESIAN_POINT('Ctrl Pts',(29.567,2.58354504679088,1.93441189848628));
#37221=CARTESIAN_POINT('',(29.567,2.66526038810872,-1.81176836987473));
#37222=CARTESIAN_POINT('Origin',(29.567,0.,0.));
#37223=CARTESIAN_POINT('Ctrl Pts',(29.0607734492731,-3.2185694572822,0.00117487786690823));
#37224=CARTESIAN_POINT('Ctrl Pts',(29.0986187691472,-3.21667663602536,-0.613998780257283));
#37225=CARTESIAN_POINT('Ctrl Pts',(29.201912520872,-2.75336214083532,-2.29607392539308));
#37226=CARTESIAN_POINT('Ctrl Pts',(29.3706547044477,-0.0451685032330799,
-3.79409447712557));
#37227=CARTESIAN_POINT('Ctrl Pts',(29.5015515681492,2.06922537276306,-2.68858493359273));
#37228=CARTESIAN_POINT('Ctrl Pts',(29.567,2.6652603881087,-1.81176836987477));
#37229=CARTESIAN_POINT('Origin',(15.6892265507269,0.,0.));
#37230=CARTESIAN_POINT('',(27.5642265507269,-3.22109517432664,-0.0026659098327413));
#37231=CARTESIAN_POINT('',(27.8107734492731,-3.22738912687624,0.00101701438904953));
#37232=CARTESIAN_POINT('',(15.6892265507269,-3.22275,-1.83004677902795E-13));
#37233=CARTESIAN_POINT('Ctrl Pts',(27.5642265507269,-3.22109517432664,-0.00266590983274053));
#37234=CARTESIAN_POINT('Ctrl Pts',(27.5831241945059,-3.22357985231351,-0.309115529678735));
#37235=CARTESIAN_POINT('Ctrl Pts',(27.6674702701357,-3.04388313860946,-1.67404196095562));
#37236=CARTESIAN_POINT('Ctrl Pts',(27.8172647776164,-1.11763786140405,-3.62729345221592));
#37237=CARTESIAN_POINT('Ctrl Pts',(28.0136100731686,2.41032302518161,-2.93201452186437));
#37238=CARTESIAN_POINT('Ctrl Pts',(28.2099553687211,3.77496404659118,0.394752895225204));
#37239=CARTESIAN_POINT('Ctrl Pts',(28.4063006642733,1.75161877719691,3.36725853372798));
#37240=CARTESIAN_POINT('Ctrl Pts',(28.6026459598257,-1.84395765825054,3.31756249130118));
#37241=CARTESIAN_POINT('Ctrl Pts',(28.7386212553102,-3.18770250249994,1.22119202818211));
#37242=CARTESIAN_POINT('Ctrl Pts',(28.8091481189439,-3.22744254261332,0.0833624900826931));
#37243=CARTESIAN_POINT('Ctrl Pts',(28.8142265507269,-3.2269979792094,0.00139874504058531));
#37244=CARTESIAN_POINT('Ctrl Pts',(27.8107734492731,-3.22738912687624,0.00101701438904955));
#37245=CARTESIAN_POINT('Ctrl Pts',(27.8725948447092,-3.22321499523797,-0.996432658533559));
#37246=CARTESIAN_POINT('Ctrl Pts',(27.9998646719961,-2.19659766354631,-3.05730343752226));
#37247=CARTESIAN_POINT('Ctrl Pts',(28.1925829311337,1.2958220592028,-3.56752694153447));
#37248=CARTESIAN_POINT('Ctrl Pts',(28.388928226686,3.69067264195723,-0.885547301338346));
#37249=CARTESIAN_POINT('Ctrl Pts',(28.5852735222384,2.77367792053198,2.59136610467845));
#37250=CARTESIAN_POINT('Ctrl Pts',(28.7816188177907,-0.633806061838565,
3.7422199926669));
#37251=CARTESIAN_POINT('Ctrl Pts',(28.9401187934689,-2.92357971927845,1.96041199187571));
#37252=CARTESIAN_POINT('Ctrl Pts',(29.0331703372964,-3.21995001787142,0.449861992332215));
#37253=CARTESIAN_POINT('Ctrl Pts',(29.0607734492731,-3.2185694572822,0.00117487786690823));
#37254=CARTESIAN_POINT('Origin',(15.6892265507269,0.,0.));
#37255=CARTESIAN_POINT('',(26.3142265507269,-3.21963434354893,0.00223887197271718));
#37256=CARTESIAN_POINT('',(26.5607734492731,-3.22048443636447,-0.00253212360901173));
#37257=CARTESIAN_POINT('',(15.6892265507269,-3.22275,-1.83004677902795E-13));
#37258=CARTESIAN_POINT('Ctrl Pts',(26.3142265507269,-3.21963434354893,0.00223887197271691));
#37259=CARTESIAN_POINT('Ctrl Pts',(26.3571002700679,-3.21505606815715,-0.693813677238957));
#37260=CARTESIAN_POINT('Ctrl Pts',(26.4654224212598,-2.65391429960236,-2.45914715185642));
#37261=CARTESIAN_POINT('Ctrl Pts',(26.6391930043024,0.237686884393074,-3.7881193692251));
#37262=CARTESIAN_POINT('Ctrl Pts',(26.8355382998547,3.29161350856939,-1.88987422206122));
#37263=CARTESIAN_POINT('Ctrl Pts',(27.0318835954071,3.39129182252066,1.70454680934583));
#37264=CARTESIAN_POINT('Ctrl Pts',(27.2282288909593,0.447261799442319,3.76912497394121));
#37265=CARTESIAN_POINT('Ctrl Pts',(27.4056765427327,-2.57620177321888,2.57776097278147));
#37266=CARTESIAN_POINT('Ctrl Pts',(27.5176757626552,-3.21497463783302,0.752215041195907));
#37267=CARTESIAN_POINT('Ctrl Pts',(27.5642265507269,-3.22109517432664,-0.00266590983274053));
#37268=CARTESIAN_POINT('Ctrl Pts',(26.5607734492731,-3.22048443636446,-0.002532123609012));
#37269=CARTESIAN_POINT('Ctrl Pts',(26.5811224884204,-3.22298870685491,-0.332677235491898));
#37270=CARTESIAN_POINT('Ctrl Pts',(26.6669199594186,-3.02559276303903,-1.72174377610718));
#37271=CARTESIAN_POINT('Ctrl Pts',(26.8181658622674,-1.03798327082204,-3.65088212414849));
#37272=CARTESIAN_POINT('Ctrl Pts',(27.0145111578197,2.47390373029963,-2.87856768367053));
#37273=CARTESIAN_POINT('Ctrl Pts',(27.2108564533721,3.76543843873028,0.477281287863921));
#37274=CARTESIAN_POINT('Ctrl Pts',(27.4072017489244,1.67747438921608,3.40476947033153));
#37275=CARTESIAN_POINT('Ctrl Pts',(27.6035470444767,-1.91605542660869,3.27644640572374));
#37276=CARTESIAN_POINT('Ctrl Pts',(27.738070944593,-3.19988118387297,1.17378932561218));
#37277=CARTESIAN_POINT('Ctrl Pts',(27.8071464128584,-3.22763402150124,0.0595369856705937));
#37278=CARTESIAN_POINT('Ctrl Pts',(27.8107734492731,-3.22738912687624,0.00101701438904955));
#37279=CARTESIAN_POINT('Origin',(15.6892265507269,0.,0.));
#37280=CARTESIAN_POINT('',(25.0642265507269,-3.22774412020477,-0.000401821292809558));
#37281=CARTESIAN_POINT('',(25.3107734492731,-3.22017561685325,0.00244165668128279));
#37282=CARTESIAN_POINT('',(15.6892265507269,-3.22275,-1.83004677902795E-13));
#37283=CARTESIAN_POINT('Ctrl Pts',(25.0642265507269,-3.22774412020477,-0.000401821292809641));
#37284=CARTESIAN_POINT('Ctrl Pts',(25.0656279137792,-3.22778459631103,-0.0230053114811701));
#37285=CARTESIAN_POINT('Ctrl Pts',(25.1324777086823,-3.21741583386448,-1.10123077018649));
#37286=CARTESIAN_POINT('Ctrl Pts',(25.2647759354361,-2.02490994382068,-3.2103088390008));
#37287=CARTESIAN_POINT('Ctrl Pts',(25.4611212309884,1.56227329051694,-3.45913938637011));
#37288=CARTESIAN_POINT('Ctrl Pts',(25.6574665265407,3.74730462149625,-0.603366577456954));
#37289=CARTESIAN_POINT('Ctrl Pts',(25.8538118220931,2.56910214256522,2.79393222142319));
#37290=CARTESIAN_POINT('Ctrl Pts',(26.0501571176454,-0.914888612658763,
3.68365606078035));
#37291=CARTESIAN_POINT('Ctrl Pts',(26.2036286938567,-2.99629870821356,1.79491000424181));
#37292=CARTESIAN_POINT('Ctrl Pts',(26.2916518382172,-3.22204498700017,0.368738126798843));
#37293=CARTESIAN_POINT('Ctrl Pts',(26.3142265507269,-3.21963434354893,0.00223887197271691));
#37294=CARTESIAN_POINT('Ctrl Pts',(25.3107734492731,-3.22017561685325,0.00244165668128262));
#37295=CARTESIAN_POINT('Ctrl Pts',(25.3550985639825,-3.21495240151903,-0.716868791691903));
#37296=CARTESIAN_POINT('Ctrl Pts',(25.4648721105426,-2.62384997733627,-2.50606997404072));
#37297=CARTESIAN_POINT('Ctrl Pts',(25.6400940889534,0.320532234955617,-3.78201078961425));
#37298=CARTESIAN_POINT('Ctrl Pts',(25.8364393845058,3.33218487481924,-1.81738565586481));
#37299=CARTESIAN_POINT('Ctrl Pts',(26.0327846800581,3.353176683897,1.77835660933565));
#37300=CARTESIAN_POINT('Ctrl Pts',(26.2291299756105,0.364667642181413,3.7780106271763));
#37301=CARTESIAN_POINT('Ctrl Pts',(26.4051262320154,-2.60748720280079,2.53104817443241));
#37302=CARTESIAN_POINT('Ctrl Pts',(26.5156740565697,-3.21493424416785,0.729165522757876));
#37303=CARTESIAN_POINT('Ctrl Pts',(26.5607734492731,-3.22048443636446,-0.002532123609012));
#37304=CARTESIAN_POINT('Origin',(15.6892265507269,0.,0.));
#37305=CARTESIAN_POINT('',(23.8142265507269,-3.21875508197893,-0.00173903194394261));
#37306=CARTESIAN_POINT('',(24.0607734492731,-3.22754701096656,-0.000807333834090818));
#37307=CARTESIAN_POINT('',(15.6892265507269,-3.22275,-1.83004677902795E-13));
#37308=CARTESIAN_POINT('Ctrl Pts',(23.8142265507269,-3.21875508197893,-0.00173903194394299));
#37309=CARTESIAN_POINT('Ctrl Pts',(23.8396039893412,-3.22082245996468,-0.414024034281807));
#37310=CARTESIAN_POINT('Ctrl Pts',(23.9304298598063,-2.95721982843924,-1.88704958033111));
#37311=CARTESIAN_POINT('Ctrl Pts',(24.0867041621221,-0.758431521083658,
-3.71902201613955));
#37312=CARTESIAN_POINT('Ctrl Pts',(24.2830494576745,2.68485587331004,-2.68288875433691));
#37313=CARTESIAN_POINT('Ctrl Pts',(24.4793947532267,3.71846513208049,0.761157139313524));
#37314=CARTESIAN_POINT('Ctrl Pts',(24.6757400487791,1.41472424965457,3.52205883332719));
#37315=CARTESIAN_POINT('Ctrl Pts',(24.8706839812791,-2.13323749993867,3.12474262705387));
#37316=CARTESIAN_POINT('Ctrl Pts',(25.0001794819284,-3.22589422416346,1.03265473662003));
#37317=CARTESIAN_POINT('Ctrl Pts',(25.0642265507269,-3.22774412020477,-0.000401821292809641));
#37318=CARTESIAN_POINT('Ctrl Pts',(24.0607734492731,-3.22754701096656,-0.000807333834090818));
#37319=CARTESIAN_POINT('Ctrl Pts',(24.0636262076937,-3.22770425869004,-0.0468288853761836));
#37320=CARTESIAN_POINT('Ctrl Pts',(24.131927397965,-3.20613122516383,-1.14853352224944));
#37321=CARTESIAN_POINT('Ctrl Pts',(24.2656770200872,-1.95416830672108,-3.25385505757741));
#37322=CARTESIAN_POINT('Ctrl Pts',(24.4620223156395,1.63760182067,-3.42412131560862));
#37323=CARTESIAN_POINT('Ctrl Pts',(24.6583676111919,3.75961212255236,-0.521213199180538));
#37324=CARTESIAN_POINT('Ctrl Pts',(24.8547129067441,2.50734255139624,2.84948764361036));
#37325=CARTESIAN_POINT('Ctrl Pts',(25.0510582022965,-0.995285623997665,
3.66275211200675));
#37326=CARTESIAN_POINT('Ctrl Pts',(25.2030783831395,-3.01557416881359,1.74719555501021));
#37327=CARTESIAN_POINT('Ctrl Pts',(25.2896501321317,-3.22266476177089,0.345232032380632));
#37328=CARTESIAN_POINT('Ctrl Pts',(25.3107734492731,-3.22017561685325,0.00244165668128262));
#37329=CARTESIAN_POINT('Origin',(15.6892265507269,0.,0.));
#37330=CARTESIAN_POINT('',(22.5642265507269,-3.22236731757899,0.00278473722726826));
#37331=CARTESIAN_POINT('',(22.8107734492731,-3.21839779706106,-0.00143350544814236));
#37332=CARTESIAN_POINT('',(15.6892265507269,-3.22275,-1.83004677902795E-13));
#37333=CARTESIAN_POINT('Ctrl Pts',(22.5642265507269,-3.22236731757899,0.00278473722726828));
#37334=CARTESIAN_POINT('Ctrl Pts',(22.6135800649032,-3.2153580953679,-0.796740891757197));
#37335=CARTESIAN_POINT('Ctrl Pts',(22.7283820109303,-2.5134926350336,-2.66752532507124));
#37336=CARTESIAN_POINT('Ctrl Pts',(22.9086323888082,0.606112968189978,-3.74686138016046));
#37337=CARTESIAN_POINT('Ctrl Pts',(23.1049776843605,3.46028350989628,-1.55973752903206));
#37338=CARTESIAN_POINT('Ctrl Pts',(23.3013229799128,3.2088238385529,2.02726236612665));
#37339=CARTESIAN_POINT('Ctrl Pts',(23.4976682754651,0.0774208817006576,
3.79477919467037));
#37340=CARTESIAN_POINT('Ctrl Pts',(23.6686361324032,-2.709756129895,2.36820545374654));
#37341=CARTESIAN_POINT('Ctrl Pts',(23.7741555574904,-3.21549069070038,0.649259273727197));
#37342=CARTESIAN_POINT('Ctrl Pts',(23.8142265507269,-3.21875508197893,-0.00173903194394299));
#37343=CARTESIAN_POINT('Ctrl Pts',(22.8107734492731,-3.21839779706106,-0.00143350544814225));
#37344=CARTESIAN_POINT('Ctrl Pts',(22.8376022832557,-3.22018694967564,-0.437419828459572));
#37345=CARTESIAN_POINT('Ctrl Pts',(22.9298795490891,-2.93600293487459,-1.93475253165454));
#37346=CARTESIAN_POINT('Ctrl Pts',(23.0876052467732,-0.676859980052826,
-3.73472985306225));
#37347=CARTESIAN_POINT('Ctrl Pts',(23.2839505423255,2.7429275988463,-2.62348903081641));
#37348=CARTESIAN_POINT('Ctrl Pts',(23.4802958378779,3.70091723594858,0.842352729023196));
#37349=CARTESIAN_POINT('Ctrl Pts',(23.6766411334301,1.33730609950109,3.55217664308397));
#37350=CARTESIAN_POINT('Ctrl Pts',(23.870133670562,-2.17476694705372,3.080844659123));
#37351=CARTESIAN_POINT('Ctrl Pts',(23.9981777758429,-3.2240966567144,1.00900478004714));
#37352=CARTESIAN_POINT('Ctrl Pts',(24.0607734492731,-3.22754701096656,-0.000807333834090818));
#37353=CARTESIAN_POINT('Origin',(15.6892265507269,0.,0.));
#37354=CARTESIAN_POINT('',(21.3142265507269,-3.22607546549254,-0.00200277449169663));
#37355=CARTESIAN_POINT('',(21.5607734492731,-3.22305249003289,0.00276936624546656));
#37356=CARTESIAN_POINT('',(15.6892265507269,-3.22275,-1.83004677902795E-13));
#37357=CARTESIAN_POINT('Ctrl Pts',(21.3142265507269,-3.22607546549254,-0.00200277449169652));
#37358=CARTESIAN_POINT('Ctrl Pts',(21.3221077086144,-3.2270099175131,-0.129297585349694));
#37359=CARTESIAN_POINT('Ctrl Pts',(21.3954372983528,-3.16284144025928,-1.31275209178423));
#37360=CARTESIAN_POINT('Ctrl Pts',(21.5342153199419,-1.70206088753426,-3.39254056088757));
#37361=CARTESIAN_POINT('Ctrl Pts',(21.7305606154942,1.89228634899218,-3.29022729579853));
#37362=CARTESIAN_POINT('Ctrl Pts',(21.9269059110465,3.78829252219229,-0.234910438249147));
#37363=CARTESIAN_POINT('Ctrl Pts',(22.1232512065989,2.28427793986952,3.03124023631671));
#37364=CARTESIAN_POINT('Ctrl Pts',(22.3195965021511,-1.26989309433504,3.57683025625195));
#37365=CARTESIAN_POINT('Ctrl Pts',(22.4665882835272,-3.07743188805749,1.58197501572629));
#37366=CARTESIAN_POINT('Ctrl Pts',(22.5481316330524,-3.22465312956892,0.26352197938507));
#37367=CARTESIAN_POINT('Ctrl Pts',(22.5642265507269,-3.22236731757899,0.00278473722726828));
#37368=CARTESIAN_POINT('Ctrl Pts',(21.5607734492731,-3.22305249003289,0.0027693662454667));
#37369=CARTESIAN_POINT('Ctrl Pts',(21.6115783588177,-3.21572847361237,-0.81982052848557));
#37370=CARTESIAN_POINT('Ctrl Pts',(21.7278317002131,-2.47981631979778,-2.713754880308));
#37371=CARTESIAN_POINT('Ctrl Pts',(21.9095334734593,0.687967117255592,-3.7326997973555));
#37372=CARTESIAN_POINT('Ctrl Pts',(22.1058787690116,3.4935896922385,-1.48363660295612));
#37373=CARTESIAN_POINT('Ctrl Pts',(22.3022240645639,3.16368950509114,2.09700148223756));
#37374=CARTESIAN_POINT('Ctrl Pts',(22.4985693601162,-0.0056455659831341,
3.79556512770198));
#37375=CARTESIAN_POINT('Ctrl Pts',(22.668085821686,-2.73754467296897,2.32096163862923));
#37376=CARTESIAN_POINT('Ctrl Pts',(22.7721538514049,-3.21582234579305,0.626160540631221));
#37377=CARTESIAN_POINT('Ctrl Pts',(22.8107734492731,-3.21839779706106,-0.00143350544814225));
#37378=CARTESIAN_POINT('Origin',(15.6892265507269,0.,0.));
#37379=CARTESIAN_POINT('',(20.0642265507269,-3.21774602634612,-0.000218779794079732));
#37380=CARTESIAN_POINT('',(20.3107734492731,-3.22548804594158,-0.00225964513658777));
#37381=CARTESIAN_POINT('',(15.6892265507269,-3.22275,-1.83004677902795E-13));
#37382=CARTESIAN_POINT('Ctrl Pts',(20.0642265507269,-3.21774602634612,-0.000218779794079575));
#37383=CARTESIAN_POINT('Ctrl Pts',(20.0960837841765,-3.21806969513006,-0.518183692896789));
#37384=CARTESIAN_POINT('Ctrl Pts',(20.1933894494768,-2.85716533250164,-2.09984699965927));
#37385=CARTESIAN_POINT('Ctrl Pts',(20.3561435466279,-0.391994200717362,
-3.77526967626554));
#37386=CARTESIAN_POINT('Ctrl Pts',(20.5524888421802,2.93378458769563,-2.4081644931002));
#37387=CARTESIAN_POINT('Ctrl Pts',(20.7488341377326,3.62647114324965,1.12029158418925));
#37388=CARTESIAN_POINT('Ctrl Pts',(20.9451794332849,1.06437219164148,3.64327488510088));
#37389=CARTESIAN_POINT('Ctrl Pts',(21.1336435709497,-2.31182328174945,2.92637254547445));
#37390=CARTESIAN_POINT('Ctrl Pts',(21.2566592767637,-3.21924983704549,0.927811772471571));
#37391=CARTESIAN_POINT('Ctrl Pts',(21.3142265507269,-3.22607546549254,-0.00200277449169652));
#37392=CARTESIAN_POINT('Ctrl Pts',(20.3107734492731,-3.22548804594158,-0.00225964513658772));
#37393=CARTESIAN_POINT('Ctrl Pts',(20.320106002529,-3.22669615753964,-0.153069114623829));
#37394=CARTESIAN_POINT('Ctrl Pts',(20.3948869876356,-3.14910495911347,-1.36024458870627));
#37395=CARTESIAN_POINT('Ctrl Pts',(20.5351164045929,-1.62740828908083,-3.42897735581699));
#37396=CARTESIAN_POINT('Ctrl Pts',(20.7314617001453,1.96383919998109,-3.24802756047599));
#37397=CARTESIAN_POINT('Ctrl Pts',(20.9278069956976,3.79252667009079,-0.151948165376663));
#37398=CARTESIAN_POINT('Ctrl Pts',(21.12415229125,2.21739307147785,3.08050548935726));
#37399=CARTESIAN_POINT('Ctrl Pts',(21.3204975868023,-1.34786724289322,3.5481827119883));
#37400=CARTESIAN_POINT('Ctrl Pts',(21.46603797281,-3.09390410280276,1.53433044604769));
#37401=CARTESIAN_POINT('Ctrl Pts',(21.5461299269669,-3.22516349463433,0.239864827693846));
#37402=CARTESIAN_POINT('Ctrl Pts',(21.5607734492731,-3.22305249003289,0.0027693662454667));
#37403=CARTESIAN_POINT('Origin',(15.6892265507269,0.,0.));
#37404=CARTESIAN_POINT('',(18.8142265507269,-3.22532168306538,0.00249477058570468));
#37405=CARTESIAN_POINT('',(19.0607734492731,-3.21773234909139,0.000164702477305489));
#37406=CARTESIAN_POINT('',(15.6892265507269,-3.22275,-1.83004677902795E-13));
#37407=CARTESIAN_POINT('Ctrl Pts',(18.8142265507269,-3.22532168306538,0.00249477058570481));
#37408=CARTESIAN_POINT('Ctrl Pts',(18.8700598597385,-3.21799059361425,-0.899808200435379));
#37409=CARTESIAN_POINT('Ctrl Pts',(18.9913416006008,-2.35673079795164,-2.87262221235205));
#37410=CARTESIAN_POINT('Ctrl Pts',(19.178071773314,0.968794511424788,-3.66969878371352));
#37411=CARTESIAN_POINT('Ctrl Pts',(19.3744170688663,3.59592225045646,-1.21480199941451));
#37412=CARTESIAN_POINT('Ctrl Pts',(19.5707623644186,2.99575257360889,2.33067906227099));
#37413=CARTESIAN_POINT('Ctrl Pts',(19.7671076599709,-0.293163078231386,
3.78420913942485));
#37414=CARTESIAN_POINT('Ctrl Pts',(19.9315957220737,-2.8280080972332,2.15667308312832));
#37415=CARTESIAN_POINT('Ctrl Pts',(20.0306353523257,-3.2174047405168,0.545938569005431));
#37416=CARTESIAN_POINT('Ctrl Pts',(20.0642265507269,-3.21774602634612,-0.000218779794079575));
#37417=CARTESIAN_POINT('Ctrl Pts',(19.0607734492731,-3.21773234909139,0.000164702477305698));
#37418=CARTESIAN_POINT('Ctrl Pts',(19.094082078091,-3.21750794441159,-0.541409146678799));
#37419=CARTESIAN_POINT('Ctrl Pts',(19.1928391387596,-2.8328436003506,-2.14744201793394));
#37420=CARTESIAN_POINT('Ctrl Pts',(19.357044631279,-0.309271563708209,-3.78292723677877));
#37421=CARTESIAN_POINT('Ctrl Pts',(19.5533899268313,2.98578041436392,-2.34339172240098));
#37422=CARTESIAN_POINT('Ctrl Pts',(19.7497352223837,3.60108775863409,1.19939252423599));
#37423=CARTESIAN_POINT('Ctrl Pts',(19.946080517936,0.984384060858174,3.66569394308102));
#37424=CARTESIAN_POINT('Ctrl Pts',(20.1330932602325,-2.34943880221939,2.88116800122945));
#37425=CARTESIAN_POINT('Ctrl Pts',(20.2546575706782,-3.21822376982043,0.904545346885408));
#37426=CARTESIAN_POINT('Ctrl Pts',(20.3107734492731,-3.22548804594158,-0.00225964513658772));
#37427=CARTESIAN_POINT('Origin',(1.07322330470336,0.,-2.95337249083895E-16));
#37428=CARTESIAN_POINT('',(1.5,10.,-1.22464679914735E-15));
#37429=CARTESIAN_POINT('',(1.5,-10.,-1.22464679914735E-15));
#37430=CARTESIAN_POINT('Origin',(1.5,0.,0.));
#37431=CARTESIAN_POINT('Origin',(1.5,0.,0.));
#37432=CARTESIAN_POINT('',(0.646446609406726,9.64644660940673,1.18134899633558E-15));
#37433=CARTESIAN_POINT('',(1.07322330470336,9.82322330470336,1.20299789774147E-15));
#37434=CARTESIAN_POINT('',(0.646446609406727,-9.64644660940673,-1.18134899633558E-15));
#37435=CARTESIAN_POINT('Origin',(0.646446609406726,0.,-5.90674498167789E-16));
#37436=CARTESIAN_POINT('Origin',(0.646446609406726,0.,-5.90674498167789E-16));
#37437=CARTESIAN_POINT('Origin',(0.499999999999998,0.,0.));
#37438=CARTESIAN_POINT('',(0.353553390593272,-9.35355339059327,-1.14547992204439E-15));
#37439=CARTESIAN_POINT('',(0.499999999999998,-9.5,-1.16341445918999E-15));
#37440=CARTESIAN_POINT('',(0.353553390593273,9.35355339059327,-1.14547992204439E-15));
#37441=CARTESIAN_POINT('Origin',(0.353553390593273,0.,-5.72739961022196E-16));
#37442=CARTESIAN_POINT('Origin',(0.353553390593273,0.,-5.72739961022196E-16));
#37443=CARTESIAN_POINT('Origin',(8.5,0.,0.));
#37444=CARTESIAN_POINT('',(16.,-10.,-1.22464679914735E-15));
#37445=CARTESIAN_POINT('Origin',(16.,0.,0.));
#37446=CARTESIAN_POINT('',(8.5,-10.,-1.22464679914735E-15));
#37447=CARTESIAN_POINT('Origin',(0.176776695296637,0.,-2.86369980511098E-16));
#37448=CARTESIAN_POINT('',(0.,8.5,1.04094977927525E-15));
#37449=CARTESIAN_POINT('',(0.176776695296637,8.92677669529664,1.09321485065982E-15));
#37450=CARTESIAN_POINT('Origin',(0.,0.,0.));
#37451=CARTESIAN_POINT('Origin',(0.,9.,0.));
#37452=CARTESIAN_POINT('Origin',(29.567,5.160062080289E-16,2.1385152528819E-16));
#37453=CARTESIAN_POINT('Ctrl Pts',(29.567,2.58354504679086,1.93441189848631));
#37454=CARTESIAN_POINT('Ctrl Pts',(29.567,2.5357479655558,2.01606960699232));
#37455=CARTESIAN_POINT('Ctrl Pts',(29.567,2.48426441181918,2.09531344700358));
#37456=CARTESIAN_POINT('Ctrl Pts',(29.567,2.42916068607862,2.17185484687615));
#37457=CARTESIAN_POINT('Ctrl Pts',(29.567,2.3689342927271,2.25551184818501));
#37458=CARTESIAN_POINT('Ctrl Pts',(29.567,2.3043843778012,2.33594190953952));
#37459=CARTESIAN_POINT('Ctrl Pts',(29.567,2.23590045951489,2.41306308144303));
#37460=CARTESIAN_POINT('Ctrl Pts',(29.567,2.19338902603406,2.4609360953035));
#37461=CARTESIAN_POINT('Ctrl Pts',(29.567,2.14936068361547,2.50753370779899));
#37462=CARTESIAN_POINT('Ctrl Pts',(29.567,2.10389981603521,2.55283175212573));
#37463=CARTESIAN_POINT('Ctrl Pts',(29.567,2.08961950353059,2.56706091807141));
#37464=CARTESIAN_POINT('Ctrl Pts',(29.567,2.07519779339987,2.58116182233106));
#37465=CARTESIAN_POINT('Ctrl Pts',(29.567,2.06063718025006,2.59513363350206));
#37466=CARTESIAN_POINT('Ctrl Pts',(29.567,2.04725437029449,2.60797526947665));
#37467=CARTESIAN_POINT('Ctrl Pts',(29.567,2.03376144273307,2.62070091822984));
#37468=CARTESIAN_POINT('Ctrl Pts',(29.567,2.02016096074622,2.63330999588553));
#37469=CARTESIAN_POINT('Ctrl Pts',(29.567,1.94243338502426,2.70537163599613));
#37470=CARTESIAN_POINT('Ctrl Pts',(29.567,1.86119439665059,2.77362993398164));
#37471=CARTESIAN_POINT('Ctrl Pts',(29.567,1.7768536571144,2.8380012403174));
#37472=CARTESIAN_POINT('Ctrl Pts',(29.567,1.6954072541691,2.90016350475531));
#37473=CARTESIAN_POINT('Ctrl Pts',(29.567,1.61106755085086,2.95870120222006));
#37474=CARTESIAN_POINT('Ctrl Pts',(29.567,1.52416618420263,3.01351548305743));
#37475=CARTESIAN_POINT('Ctrl Pts',(29.567,1.48476950634889,3.03836550150048));
#37476=CARTESIAN_POINT('Ctrl Pts',(29.567,1.4448458926919,3.0624499158597));
#37477=CARTESIAN_POINT('Ctrl Pts',(29.567,1.40442422564169,3.08575765411971));
#37478=CARTESIAN_POINT('Ctrl Pts',(29.567,1.3882956126443,3.09505765379002));
#37479=CARTESIAN_POINT('Ctrl Pts',(29.567,1.37208617296854,3.10423482964628));
#37480=CARTESIAN_POINT('Ctrl Pts',(29.567,1.35580246527857,3.11328577356711));
#37481=CARTESIAN_POINT('Ctrl Pts',(29.567,1.25886714739215,3.16716515674211));
#37482=CARTESIAN_POINT('Ctrl Pts',(29.567,1.15956514623483,3.21642936845675));
#37483=CARTESIAN_POINT('Ctrl Pts',(29.567,1.05833049025747,3.26099255600975));
#37484=CARTESIAN_POINT('Ctrl Pts',(29.567,0.955355806808139,3.30632169836185));
#37485=CARTESIAN_POINT('Ctrl Pts',(29.567,0.85038079758029,3.34678738341505));
#37486=CARTESIAN_POINT('Ctrl Pts',(29.567,0.743820340173551,3.3822652553553));
#37487=CARTESIAN_POINT('Ctrl Pts',(29.567,0.637179374181623,3.41776993154682));
#37488=CARTESIAN_POINT('Ctrl Pts',(29.567,0.528949752068905,3.44827974859085));
#37489=CARTESIAN_POINT('Ctrl Pts',(29.567,0.419516975660503,3.47362849800319));
#37490=CARTESIAN_POINT('Ctrl Pts',(29.567,0.342210256475242,3.49153564352972));
#37491=CARTESIAN_POINT('Ctrl Pts',(29.567,0.264302453480718,3.50686633363735));
#37492=CARTESIAN_POINT('Ctrl Pts',(29.567,0.185923742235531,3.51954741773577));
#37493=CARTESIAN_POINT('Ctrl Pts',(29.567,0.162525512979304,3.5233330746857));
#37494=CARTESIAN_POINT('Ctrl Pts',(29.567,0.139085294911744,3.52688251402397));
#37495=CARTESIAN_POINT('Ctrl Pts',(29.567,0.115606504489892,3.53019355998364));
#37496=CARTESIAN_POINT('Ctrl Pts',(29.567,0.0954384156821029,3.5330377213634));
#37497=CARTESIAN_POINT('Ctrl Pts',(29.567,0.0752384615584927,3.53570630508463));
#37498=CARTESIAN_POINT('Ctrl Pts',(29.567,0.0550345809701694,3.53819496903935));
#37499=CARTESIAN_POINT('Ctrl Pts',(29.567,-0.0599756574808101,3.552361645268));
#37500=CARTESIAN_POINT('Ctrl Pts',(29.567,-0.175272224620941,3.5607264093425));
#37501=CARTESIAN_POINT('Ctrl Pts',(29.567,-0.290425098911766,3.56316203636081));
#37502=CARTESIAN_POINT('Ctrl Pts',(29.567,-0.36815124373659,3.56480604133706));
#37503=CARTESIAN_POINT('Ctrl Pts',(29.567,-0.445812651568658,3.56374789754405));
#37504=CARTESIAN_POINT('Ctrl Pts',(29.567,-0.523283233678614,3.55993654290422));
#37505=CARTESIAN_POINT('Ctrl Pts',(29.567,-0.63435909064238,3.55447189463025));
#37506=CARTESIAN_POINT('Ctrl Pts',(29.567,-0.74504273400306,3.54335004573931));
#37507=CARTESIAN_POINT('Ctrl Pts',(29.567,-0.85505603383999,3.52683910178606));
#37508=CARTESIAN_POINT('Ctrl Pts',(29.567,-0.967076221847354,3.51002696135791));
#37509=CARTESIAN_POINT('Ctrl Pts',(29.567,-1.07840207048601,3.48762718741913));
#37510=CARTESIAN_POINT('Ctrl Pts',(29.567,-1.18874066520512,3.45986878136783));
#37511=CARTESIAN_POINT('Ctrl Pts',(29.567,-1.21464526759529,3.45335183710572));
#37512=CARTESIAN_POINT('Ctrl Pts',(29.567,-1.24049543083138,3.44653930625182));
#37513=CARTESIAN_POINT('Ctrl Pts',(29.567,-1.26628730485178,3.43943374373268));
#37514=CARTESIAN_POINT('Ctrl Pts',(29.567,-1.28464244035827,3.43437697419413));
#37515=CARTESIAN_POINT('Ctrl Pts',(29.567,-1.30296950645519,3.42917127609625));
#37516=CARTESIAN_POINT('Ctrl Pts',(29.567,-1.32124694883733,3.42382369155869));
#37517=CARTESIAN_POINT('Ctrl Pts',(29.567,-1.43060976561301,3.39182649546605));
#37518=CARTESIAN_POINT('Ctrl Pts',(29.567,-1.53835947619341,3.35470979815077));
#37519=CARTESIAN_POINT('Ctrl Pts',(29.567,-1.64421117916582,3.31278265355743));
#37520=CARTESIAN_POINT('Ctrl Pts',(29.567,-1.7534671731585,3.26950709228456));
#37521=CARTESIAN_POINT('Ctrl Pts',(29.567,-1.86070180847822,3.22110664138685));
#37522=CARTESIAN_POINT('Ctrl Pts',(29.567,-1.96560378724298,3.16786574642619));
#37523=CARTESIAN_POINT('Ctrl Pts',(29.567,-2.07149822315375,3.11412114975002));
#37524=CARTESIAN_POINT('Ctrl Pts',(29.567,-2.17501644885382,3.05544380388699));
#37525=CARTESIAN_POINT('Ctrl Pts',(29.567,-2.27582884554067,2.9920735879525));
#37526=CARTESIAN_POINT('Ctrl Pts',(29.567,-2.34151280990235,2.95078494546578));
#37527=CARTESIAN_POINT('Ctrl Pts',(29.567,-2.40604789877361,2.90750305324507));
#37528=CARTESIAN_POINT('Ctrl Pts',(29.567,-2.46933834269369,2.86228329757719));
#37529=CARTESIAN_POINT('Ctrl Pts',(29.567,-2.49060749325209,2.84708691512286));
#37530=CARTESIAN_POINT('Ctrl Pts',(29.567,-2.51173604271137,2.83167161394492));
#37531=CARTESIAN_POINT('Ctrl Pts',(29.567,-2.53272022923281,2.81603929283293));
#37532=CARTESIAN_POINT('Ctrl Pts',(29.567,-2.545674982638,2.80638855583869));
#37533=CARTESIAN_POINT('Ctrl Pts',(29.567,-2.55857471352845,2.79665510390201));
#37534=CARTESIAN_POINT('Ctrl Pts',(29.567,-2.57141852281522,2.78683936514258));
#37535=CARTESIAN_POINT('Ctrl Pts',(29.567,-2.58480907193538,2.77660578653097));
#37536=CARTESIAN_POINT('Ctrl Pts',(29.567,-2.59813128992878,2.76628852165279));
#37537=CARTESIAN_POINT('Ctrl Pts',(29.567,-2.61138252346487,2.75588981439117));
#37538=CARTESIAN_POINT('Ctrl Pts',(29.567,-2.70776223489835,2.68025727781063));
#37539=CARTESIAN_POINT('Ctrl Pts',(29.567,-2.80041912899082,2.60029670152484));
#37540=CARTESIAN_POINT('Ctrl Pts',(29.567,-2.88902699235769,2.51630659159321));
#37541=CARTESIAN_POINT('Ctrl Pts',(29.567,-2.9778000606268,2.43215988632824));
#37542=CARTESIAN_POINT('Ctrl Pts',(29.567,-3.0625098043098,2.34396820492412));
#37543=CARTESIAN_POINT('Ctrl Pts',(29.567,-3.14281079119611,2.25198224343805));
#37544=CARTESIAN_POINT('Ctrl Pts',(29.567,-3.2216186616731,2.16170666875852));
#37545=CARTESIAN_POINT('Ctrl Pts',(29.567,-3.29618089668985,2.06777608333632));
#37546=CARTESIAN_POINT('Ctrl Pts',(29.567,-3.36614317640108,1.97038692453017));
#37547=CARTESIAN_POINT('Ctrl Pts',(29.567,-3.43597914568637,1.87317359284375));
#37548=CARTESIAN_POINT('Ctrl Pts',(29.567,-3.50123252391352,1.7725137716817));
#37549=CARTESIAN_POINT('Ctrl Pts',(29.567,-3.56151197810524,1.66856867698424));
#37550=CARTESIAN_POINT('',(29.567,-3.48663465726742,-1.83204761571504));
#37551=CARTESIAN_POINT('Origin',(29.567,0.,0.));
#37552=CARTESIAN_POINT('Ctrl Pts',(29.567,-3.48672441430165,-1.8321351845655));
#37553=CARTESIAN_POINT('Ctrl Pts',(29.567,-3.42554918772991,-1.92852802099295));
#37554=CARTESIAN_POINT('Ctrl Pts',(29.567,-3.36004658914194,-2.02190377063076));
#37555=CARTESIAN_POINT('Ctrl Pts',(29.567,-3.29021431614292,-2.11191494002337));
#37556=CARTESIAN_POINT('Ctrl Pts',(29.567,-3.21555245835795,-2.20815126228005));
#37557=CARTESIAN_POINT('Ctrl Pts',(29.567,-3.13594084671758,-2.30054222096486));
#37558=CARTESIAN_POINT('Ctrl Pts',(29.567,-3.05179321734777,-2.3889096735599));
#37559=CARTESIAN_POINT('Ctrl Pts',(29.567,-3.00396143039123,-2.43914012209508));
#37560=CARTESIAN_POINT('Ctrl Pts',(29.567,-2.95466342451523,-2.48806976487008));
#37561=CARTESIAN_POINT('Ctrl Pts',(29.567,-2.90397163769525,-2.53565937397679));
#37562=CARTESIAN_POINT('Ctrl Pts',(29.567,-2.88322820540287,-2.55513337353872));
#37563=CARTESIAN_POINT('Ctrl Pts',(29.567,-2.86225136074878,-2.57438292681157));
#37564=CARTESIAN_POINT('Ctrl Pts',(29.567,-2.84104598347864,-2.59340510346618));
#37565=CARTESIAN_POINT('Ctrl Pts',(29.567,-2.82615821911944,-2.60676009734462));
#37566=CARTESIAN_POINT('Ctrl Pts',(29.567,-2.81116146340808,-2.619999679795));
#37567=CARTESIAN_POINT('Ctrl Pts',(29.567,-2.79606334508375,-2.63311809249039));
#37568=CARTESIAN_POINT('Ctrl Pts',(29.567,-2.70210212906268,-2.71475886272721));
#37569=CARTESIAN_POINT('Ctrl Pts',(29.567,-2.60415037276475,-2.79177128477282));
#37570=CARTESIAN_POINT('Ctrl Pts',(29.567,-2.50265605670507,-2.86397207182206));
#37571=CARTESIAN_POINT('Ctrl Pts',(29.567,-2.41384853015285,-2.92714776049014));
#37572=CARTESIAN_POINT('Ctrl Pts',(29.567,-2.32232774488169,-2.98663895631543));
#37573=CARTESIAN_POINT('Ctrl Pts',(29.567,-2.22838012565767,-3.04228906112937));
#37574=CARTESIAN_POINT('Ctrl Pts',(29.567,-2.18727804224717,-3.06663598198547));
#37575=CARTESIAN_POINT('Ctrl Pts',(29.567,-2.14571133542366,-3.09024726946961));
#37576=CARTESIAN_POINT('Ctrl Pts',(29.567,-2.10370364166454,-3.11310776922122));
#37577=CARTESIAN_POINT('Ctrl Pts',(29.567,-2.07785961441306,-3.12717203520905));
#37578=CARTESIAN_POINT('Ctrl Pts',(29.567,-2.051848672141,-3.14095210526973));
#37579=CARTESIAN_POINT('Ctrl Pts',(29.567,-2.02567630908807,-3.15444420661779));
#37580=CARTESIAN_POINT('Ctrl Pts',(29.567,-2.01068994039449,-3.16216982179608));
#37581=CARTESIAN_POINT('Ctrl Pts',(29.567,-1.99565392079183,-3.16979928816491));
#37582=CARTESIAN_POINT('Ctrl Pts',(29.567,-1.98057677496915,-3.17732840555982));
#37583=CARTESIAN_POINT('Ctrl Pts',(29.567,-1.87426334421613,-3.23041844728323));
#37584=CARTESIAN_POINT('Ctrl Pts',(29.567,-1.76579720789928,-3.2785796607992));
#37585=CARTESIAN_POINT('Ctrl Pts',(29.567,-1.65556247533349,-3.32165304965814));
#37586=CARTESIAN_POINT('Ctrl Pts',(29.567,-1.54607261710998,-3.36443538449582));
#37587=CARTESIAN_POINT('Ctrl Pts',(29.567,-1.43483710785183,-3.40219862409269));
#37588=CARTESIAN_POINT('Ctrl Pts',(29.567,-1.32222161270656,-3.43473703889271));
#37589=CARTESIAN_POINT('Ctrl Pts',(29.567,-1.21291663581304,-3.46631893331391));
#37590=CARTESIAN_POINT('Ctrl Pts',(29.567,-1.10231087406112,-3.49297866087499));
#37591=CARTESIAN_POINT('Ctrl Pts',(29.567,-0.990740369207159,-3.51447981885924));
#37592=CARTESIAN_POINT('Ctrl Pts',(29.567,-0.912857639994659,-3.52948888301319));
#37593=CARTESIAN_POINT('Ctrl Pts',(29.567,-0.834504833305636,-3.54198326314598));
#37594=CARTESIAN_POINT('Ctrl Pts',(29.567,-0.755799562093794,-3.5518679234343));
#37595=CARTESIAN_POINT('Ctrl Pts',(29.567,-0.724508003371303,-3.55579785624695));
#37596=CARTESIAN_POINT('Ctrl Pts',(29.567,-0.693160773230039,-3.55931513603026));
#37597=CARTESIAN_POINT('Ctrl Pts',(29.567,-0.661765455434889,-3.56241323914284));
#37598=CARTESIAN_POINT('Ctrl Pts',(29.567,-0.647183191863934,-3.56385222302102));
#37599=CARTESIAN_POINT('Ctrl Pts',(29.567,-0.632593320301258,-3.56520046326365));
#37600=CARTESIAN_POINT('Ctrl Pts',(29.567,-0.618005027399725,-3.56645676814378));
#37601=CARTESIAN_POINT('Ctrl Pts',(29.567,-0.506478628425292,-3.57606112420112));
#37602=CARTESIAN_POINT('Ctrl Pts',(29.567,-0.394900320726398,-3.58031092949672));
#37603=CARTESIAN_POINT('Ctrl Pts',(29.567,-0.283594313965176,-3.57902452852789));
#37604=CARTESIAN_POINT('Ctrl Pts',(29.567,-0.204277660100752,-3.57810783927324));
#37605=CARTESIAN_POINT('Ctrl Pts',(29.567,-0.125099203195263,-3.57437885322994));
#37606=CARTESIAN_POINT('Ctrl Pts',(29.567,-0.0461785851566451,-3.56775577379342));
#37607=CARTESIAN_POINT('Ctrl Pts',(29.567,0.0667712410172652,-3.55827693683443));
#37608=CARTESIAN_POINT('Ctrl Pts',(29.567,0.179194191414866,-3.54287182561656));
#37609=CARTESIAN_POINT('Ctrl Pts',(29.567,0.290735528015621,-3.52176041427356));
#37610=CARTESIAN_POINT('Ctrl Pts',(29.567,0.402570362004908,-3.5005934527257));
#37611=CARTESIAN_POINT('Ctrl Pts',(29.567,0.513519714278932,-3.47368954980131));
#37612=CARTESIAN_POINT('Ctrl Pts',(29.567,0.623196982310405,-3.44122735838397));
#37613=CARTESIAN_POINT('Ctrl Pts',(29.567,0.644440381543399,-3.43493975380889));
#37614=CARTESIAN_POINT('Ctrl Pts',(29.567,0.665635949821038,-3.42844351105179));
#37615=CARTESIAN_POINT('Ctrl Pts',(29.567,0.68678071400004,-3.42173977031026));
#37616=CARTESIAN_POINT('Ctrl Pts',(29.567,0.701774797365526,-3.41698604278281));
#37617=CARTESIAN_POINT('Ctrl Pts',(29.567,0.716742743793056,-3.41212809827565));
#37618=CARTESIAN_POINT('Ctrl Pts',(29.567,0.731670869876243,-3.40717073211752));
#37619=CARTESIAN_POINT('Ctrl Pts',(29.567,0.837287664306418,-3.37209726612978));
#37620=CARTESIAN_POINT('Ctrl Pts',(29.567,0.941079596991946,-3.33199907124987));
#37621=CARTESIAN_POINT('Ctrl Pts',(29.567,1.04272763424727,-3.28712163559775));
#37622=CARTESIAN_POINT('Ctrl Pts',(29.567,1.14450824131698,-3.24218567059793));
#37623=CARTESIAN_POINT('Ctrl Pts',(29.567,1.24414009253349,-3.1924573863102));
#37624=CARTESIAN_POINT('Ctrl Pts',(29.567,1.34127481549702,-3.13813913114634));
#37625=CARTESIAN_POINT('Ctrl Pts',(29.567,1.43724513419497,-3.08447201705832));
#37626=CARTESIAN_POINT('Ctrl Pts',(29.567,1.53077844315963,-3.02632368118162));
#37627=CARTESIAN_POINT('Ctrl Pts',(29.567,1.62150146855142,-2.96385561176368));
#37628=CARTESIAN_POINT('Ctrl Pts',(29.567,1.67545923088545,-2.92670256016997));
#37629=CARTESIAN_POINT('Ctrl Pts',(29.567,1.72842215433334,-2.88802088952323));
#37630=CARTESIAN_POINT('Ctrl Pts',(29.567,1.78030401089113,-2.84784018551755));
#37631=CARTESIAN_POINT('Ctrl Pts',(29.567,1.80469325436339,-2.82895155974546));
#37632=CARTESIAN_POINT('Ctrl Pts',(29.567,1.82884350756324,-2.80973162653502));
#37633=CARTESIAN_POINT('Ctrl Pts',(29.567,1.85274531535973,-2.79018325799309));
#37634=CARTESIAN_POINT('Ctrl Pts',(29.567,1.86456475510265,-2.78051659319429));
#37635=CARTESIAN_POINT('Ctrl Pts',(29.567,1.87631970395782,-2.77077262327817));
#37636=CARTESIAN_POINT('Ctrl Pts',(29.567,1.888003223487,-2.76095691114132));
#37637=CARTESIAN_POINT('Ctrl Pts',(29.567,1.97034400621842,-2.6917796894663));
#37638=CARTESIAN_POINT('Ctrl Pts',(29.567,2.04923212840135,-2.6189668217664));
#37639=CARTESIAN_POINT('Ctrl Pts',(29.567,2.12435271290082,-2.5427036465071));
#37640=CARTESIAN_POINT('Ctrl Pts',(29.567,2.19843508436252,-2.46749447559807));
#37641=CARTESIAN_POINT('Ctrl Pts',(29.567,2.26885383595672,-2.38892910395374));
#37642=CARTESIAN_POINT('Ctrl Pts',(29.567,2.33526556130163,-2.30715770560389));
#37643=CARTESIAN_POINT('Ctrl Pts',(29.567,2.3996396811376,-2.22789516921909));
#37644=CARTESIAN_POINT('Ctrl Pts',(29.567,2.46024915986653,-2.1456197660656));
#37645=CARTESIAN_POINT('Ctrl Pts',(29.567,2.51673667007826,-2.06045066893125));
#37646=CARTESIAN_POINT('Ctrl Pts',(29.567,2.57002707334798,-1.98010201282313));
#37647=CARTESIAN_POINT('Ctrl Pts',(29.567,2.6196488723445,-1.89717750925258));
#37648=CARTESIAN_POINT('Ctrl Pts',(29.567,2.6652603881087,-1.81176836987477));
#37649=CARTESIAN_POINT('Ctrl Pts',(17.5899369713081,-1.43290239521316,2.88667772504871));
#37650=CARTESIAN_POINT('Ctrl Pts',(17.6553854031588,-2.38256076808023,2.41528192450347));
#37651=CARTESIAN_POINT('Ctrl Pts',(17.7862822668604,-3.76505809554499,0.470670407196005));
#37652=CARTESIAN_POINT('Ctrl Pts',(17.9826275624127,-2.4662325973019,-2.88811363748521));
#37653=CARTESIAN_POINT('Ctrl Pts',(18.1789728579651,1.04930180499054,-3.6466643018069));
#37654=CARTESIAN_POINT('Ctrl Pts',(18.3753181535174,3.62142716015887,-1.1363036219263));
#37655=CARTESIAN_POINT('Ctrl Pts',(18.5716634490697,2.94414196278733,2.39593313727195));
#37656=CARTESIAN_POINT('Ctrl Pts',(18.768008744622,-0.375967469233134,3.77675880022508));
#37657=CARTESIAN_POINT('Ctrl Pts',(18.9643540401744,-3.35842001198963,1.76845082226179));
#37658=CARTESIAN_POINT('Ctrl Pts',(19.1606993357267,-3.32678023397126,-1.82732987070656));
#37659=CARTESIAN_POINT('Ctrl Pts',(19.357044631279,-0.309271563708209,-3.78292723677877));
#37660=CARTESIAN_POINT('Ctrl Pts',(19.5533899268313,2.98578041436392,-2.34339172240098));
#37661=CARTESIAN_POINT('Ctrl Pts',(19.7497352223837,3.60108775863409,1.19939252423599));
#37662=CARTESIAN_POINT('Ctrl Pts',(19.946080517936,0.984384060858174,3.66569394308102));
#37663=CARTESIAN_POINT('Ctrl Pts',(20.1424258134883,-2.5158075695727,2.84201756664935));
#37664=CARTESIAN_POINT('Ctrl Pts',(20.3387711090406,-3.75804527596442,-0.53239577264931));
#37665=CARTESIAN_POINT('Ctrl Pts',(20.5351164045929,-1.62740828908083,-3.42897735581699));
#37666=CARTESIAN_POINT('Ctrl Pts',(20.7314617001453,1.96383919998109,-3.24802756047599));
#37667=CARTESIAN_POINT('Ctrl Pts',(20.9278069956976,3.79252667009079,-0.151948165376663));
#37668=CARTESIAN_POINT('Ctrl Pts',(21.12415229125,2.21739307147785,3.08050548935726));
#37669=CARTESIAN_POINT('Ctrl Pts',(21.3204975868023,-1.34786724289322,3.5481827119883));
#37670=CARTESIAN_POINT('Ctrl Pts',(21.5168428823546,-3.70340671003476,0.831339441187419));
#37671=CARTESIAN_POINT('Ctrl Pts',(21.7131881779069,-2.73511106234691,-2.63163712022799));
#37672=CARTESIAN_POINT('Ctrl Pts',(21.9095334734593,0.687967117255592,-3.7326997973555));
#37673=CARTESIAN_POINT('Ctrl Pts',(22.1058787690116,3.4935896922385,-1.48363660295612));
#37674=CARTESIAN_POINT('Ctrl Pts',(22.3022240645639,3.16368950509114,2.09700148223756));
#37675=CARTESIAN_POINT('Ctrl Pts',(22.4985693601162,-0.0056455659831341,
3.79556512770198));
#37676=CARTESIAN_POINT('Ctrl Pts',(22.6949146556686,-3.16991370025882,2.08758081040675));
#37677=CARTESIAN_POINT('Ctrl Pts',(22.8912599512209,-3.48916068737138,-1.49402282593584));
#37678=CARTESIAN_POINT('Ctrl Pts',(23.0876052467732,-0.676859980052826,
-3.73472985306225));
#37679=CARTESIAN_POINT('Ctrl Pts',(23.2839505423255,2.7429275988463,-2.62348903081641));
#37680=CARTESIAN_POINT('Ctrl Pts',(23.4802958378779,3.70091723594858,0.842352729023196));
#37681=CARTESIAN_POINT('Ctrl Pts',(23.6766411334301,1.33730609950109,3.55217664308397));
#37682=CARTESIAN_POINT('Ctrl Pts',(23.8729864289826,-2.22654721778548,3.07389557309588));
#37683=CARTESIAN_POINT('Ctrl Pts',(24.0693317245348,-3.79205783001057,-0.163229659703893));
#37684=CARTESIAN_POINT('Ctrl Pts',(24.2656770200872,-1.95416830672108,-3.25385505757741));
#37685=CARTESIAN_POINT('Ctrl Pts',(24.4620223156395,1.63760182067,-3.42412131560862));
#37686=CARTESIAN_POINT('Ctrl Pts',(24.6583676111919,3.75961212255236,-0.521213199180538));
#37687=CARTESIAN_POINT('Ctrl Pts',(24.8547129067441,2.50734255139624,2.84948764361036));
#37688=CARTESIAN_POINT('Ctrl Pts',(25.0510582022965,-0.995285623997665,
3.66275211200675));
#37689=CARTESIAN_POINT('Ctrl Pts',(25.2474034978488,-3.6046375484147,1.18866928796936));
#37690=CARTESIAN_POINT('Ctrl Pts',(25.4437487934011,-2.97880042259369,-2.35225306850473));
#37691=CARTESIAN_POINT('Ctrl Pts',(25.6400940889534,0.320532234955617,-3.78201078961425));
#37692=CARTESIAN_POINT('Ctrl Pts',(25.8364393845058,3.33218487481924,-1.81738565586481));
#37693=CARTESIAN_POINT('Ctrl Pts',(26.0327846800581,3.353176683897,1.77835660933565));
#37694=CARTESIAN_POINT('Ctrl Pts',(26.2291299756105,0.364667642181413,3.7780106271763));
#37695=CARTESIAN_POINT('Ctrl Pts',(26.4254752711627,-2.95113369010615,2.38687188179727));
#37696=CARTESIAN_POINT('Ctrl Pts',(26.6218205667151,-3.61826984944021,-1.14650195931218));
#37697=CARTESIAN_POINT('Ctrl Pts',(26.8181658622674,-1.03798327082204,-3.65088212414849));
#37698=CARTESIAN_POINT('Ctrl Pts',(27.0145111578197,2.47390373029963,-2.87856768367053));
#37699=CARTESIAN_POINT('Ctrl Pts',(27.2108564533721,3.76543843873028,0.477281287863921));
#37700=CARTESIAN_POINT('Ctrl Pts',(27.4072017489244,1.67747438921608,3.40476947033153));
#37701=CARTESIAN_POINT('Ctrl Pts',(27.6035470444767,-1.91605542660869,3.27644640572374));
#37702=CARTESIAN_POINT('Ctrl Pts',(27.799892340029,-3.78987225417569,0.207498616647036));
#37703=CARTESIAN_POINT('Ctrl Pts',(27.9962376355814,-2.26232643032977,-3.04770082261197));
#37704=CARTESIAN_POINT('Ctrl Pts',(28.1925829311337,1.2958220592028,-3.56752694153447));
#37705=CARTESIAN_POINT('Ctrl Pts',(28.388928226686,3.69067264195723,-0.885547301338346));
#37706=CARTESIAN_POINT('Ctrl Pts',(28.5852735222384,2.77367792053198,2.59136610467845));
#37707=CARTESIAN_POINT('Ctrl Pts',(28.7816188177907,-0.633806061838565,
3.7422199926669));
#37708=CARTESIAN_POINT('Ctrl Pts',(28.977964113343,-3.47031303033562,1.53496654019299));
#37709=CARTESIAN_POINT('Ctrl Pts',(29.1743094088953,-3.19637271856563,-2.05102536576998));
#37710=CARTESIAN_POINT('Ctrl Pts',(29.3706547044477,-0.0451685032330799,
-3.79409447712557));
#37711=CARTESIAN_POINT('Ctrl Pts',(29.5015515681492,2.06922537276306,-2.68858493359273));
#37712=CARTESIAN_POINT('Ctrl Pts',(29.567,2.6652603881087,-1.81176836987477));
#37713=CARTESIAN_POINT('Ctrl Pts',(17.7266246475387,-1.53816642191913,3.09873914818277));
#37714=CARTESIAN_POINT('Ctrl Pts',(17.7920730793895,-2.55758869821535,2.59271361967877));
#37715=CARTESIAN_POINT('Ctrl Pts',(17.922969943091,-4.04164718998927,0.505246846232138));
#37716=CARTESIAN_POINT('Ctrl Pts',(18.1193152386434,-2.64740723616972,-3.10028054576993));
#37717=CARTESIAN_POINT('Ctrl Pts',(18.3156605341957,1.12638572472724,-3.91455593890342));
#37718=CARTESIAN_POINT('Ctrl Pts',(18.512005829748,3.88746482369703,-1.21977887830396));
#37719=CARTESIAN_POINT('Ctrl Pts',(18.7083511253004,3.1604248298077,2.57194342980134));
#37720=CARTESIAN_POINT('Ctrl Pts',(18.9046964208527,-0.403586831064142,
4.05420745306918));
#37721=CARTESIAN_POINT('Ctrl Pts',(19.101041716405,-3.60513661670255,1.89836494286392));
#37722=CARTESIAN_POINT('Ctrl Pts',(19.2973870119573,-3.57117251397831,-1.96156937016811));
#37723=CARTESIAN_POINT('Ctrl Pts',(19.4937323075097,-0.331991303901513,
-4.06082903595878));
#37724=CARTESIAN_POINT('Ctrl Pts',(19.690077603062,3.20512212970039,-2.51554221197617));
#37725=CARTESIAN_POINT('Ctrl Pts',(19.8864228986143,3.8656312469148,1.28750242420118));
#37726=CARTESIAN_POINT('Ctrl Pts',(20.0827681941666,1.0566989864367,3.93498353768948));
#37727=CARTESIAN_POINT('Ctrl Pts',(20.279113489719,-2.70062409027591,3.05079816052237));
#37728=CARTESIAN_POINT('Ctrl Pts',(20.4754587852713,-4.0341191939179,-0.571506686984792));
#37729=CARTESIAN_POINT('Ctrl Pts',(20.6718040808236,-1.74696112825232,-3.680877251555));
#37730=CARTESIAN_POINT('Ctrl Pts',(20.8681493763759,2.10810696217036,-3.48663450328654));
#37731=CARTESIAN_POINT('Ctrl Pts',(21.0644946719283,4.07113366385201,-0.163110597508529));
#37732=CARTESIAN_POINT('Ctrl Pts',(21.2608399674806,2.38028743488564,3.30680590813169));
#37733=CARTESIAN_POINT('Ctrl Pts',(21.4571852630329,-1.44688440828145,3.80883968415904));
#37734=CARTESIAN_POINT('Ctrl Pts',(21.6535305585853,-3.97546676390202,0.892411386793245));
#37735=CARTESIAN_POINT('Ctrl Pts',(21.8498758541376,-2.93603807933882,-2.82496272358349));
#37736=CARTESIAN_POINT('Ctrl Pts',(22.0462211496899,0.738506630097174,-4.00691178308939));
#37737=CARTESIAN_POINT('Ctrl Pts',(22.2425664452422,3.75023614624128,-1.59262767137592));
#37738=CARTESIAN_POINT('Ctrl Pts',(22.4389117407945,3.39610079679244,2.25105162603391));
#37739=CARTESIAN_POINT('Ctrl Pts',(22.6352570363469,-0.00606030114610197,
4.07439533295633));
#37740=CARTESIAN_POINT('Ctrl Pts',(22.8316023318992,-3.40278223444119,2.24093889181667));
#37741=CARTESIAN_POINT('Ctrl Pts',(23.0279476274515,-3.74548177735205,-1.60377688816228));
#37742=CARTESIAN_POINT('Ctrl Pts',(23.2242929230039,-0.726583539211172,
-4.00909097096232));
#37743=CARTESIAN_POINT('Ctrl Pts',(23.4206382185562,2.94442883506593,-2.81621605836923));
#37744=CARTESIAN_POINT('Ctrl Pts',(23.6169835141085,3.97279440780828,0.904233733940176));
#37745=CARTESIAN_POINT('Ctrl Pts',(23.8133288096608,1.43554742106091,3.81312701784159));
#37746=CARTESIAN_POINT('Ctrl Pts',(24.0096741052132,-2.39011406405363,3.29971041350562));
#37747=CARTESIAN_POINT('Ctrl Pts',(24.2060194007655,-4.07063038179243,-0.175220854160445));
#37748=CARTESIAN_POINT('Ctrl Pts',(24.4023646963179,-2.09772562473093,-3.49289010059391));
#37749=CARTESIAN_POINT('Ctrl Pts',(24.5987099918701,1.7579034981329,-3.6756644764093));
#37750=CARTESIAN_POINT('Ctrl Pts',(24.7950552874225,4.03580114435494,-0.55950261812586));
#37751=CARTESIAN_POINT('Ctrl Pts',(24.9914005829747,2.69153721404245,3.058817005064));
#37752=CARTESIAN_POINT('Ctrl Pts',(25.1877458785272,-1.06840140135594,3.93182559351093));
#37753=CARTESIAN_POINT('Ctrl Pts',(25.3840911740794,-3.86944181172621,1.27599143642233));
#37754=CARTESIAN_POINT('Ctrl Pts',(25.5804364696318,-3.19762937303946,-2.52505453122087));
#37755=CARTESIAN_POINT('Ctrl Pts',(25.7767817651841,0.344079207766316,-4.05984526465612));
#37756=CARTESIAN_POINT('Ctrl Pts',(25.9731270607364,3.5769741911216,-1.95089463236812));
#37757=CARTESIAN_POINT('Ctrl Pts',(26.1694723562888,3.59950810268922,1.9089984299113));
#37758=CARTESIAN_POINT('Ctrl Pts',(26.3658176518411,0.391456894927206,4.05555124186375));
#37759=CARTESIAN_POINT('Ctrl Pts',(26.5621629473934,-3.16793018413535,2.56221651542245));
#37760=CARTESIAN_POINT('Ctrl Pts',(26.7585082429457,-3.88407557028575,-1.23072640702519));
#37761=CARTESIAN_POINT('Ctrl Pts',(26.9548535384981,-1.11423570720934,-3.91908361135418));
#37762=CARTESIAN_POINT('Ctrl Pts',(27.1511988340504,2.65564190674782,-3.09003332609052));
#37763=CARTESIAN_POINT('Ctrl Pts',(27.3475441296027,4.04205547398569,0.512343376112075));
#37764=CARTESIAN_POINT('Ctrl Pts',(27.543889425155,1.80070518950991,3.65489100383582));
#37765=CARTESIAN_POINT('Ctrl Pts',(27.7402347207074,-2.05681289220471,3.51714105673767));
#37766=CARTESIAN_POINT('Ctrl Pts',(27.9365800162597,-4.06828424895533,0.222741901882079));
#37767=CARTESIAN_POINT('Ctrl Pts',(28.132925311812,-2.42852169287902,-3.27159134150216));
#37768=CARTESIAN_POINT('Ctrl Pts',(28.3292706073644,1.39101587582407,-3.82960498153395));
#37769=CARTESIAN_POINT('Ctrl Pts',(28.5256159029166,3.96179722437391,-0.950601470477096));
#37770=CARTESIAN_POINT('Ctrl Pts',(28.721961198469,2.9774381401227,2.78173331444731));
#37771=CARTESIAN_POINT('Ctrl Pts',(28.9183064940213,-0.680366789521514,
4.01713135199167));
#37772=CARTESIAN_POINT('Ctrl Pts',(29.1146517895737,-3.72524953174961,1.64772841386942));
#37773=CARTESIAN_POINT('Ctrl Pts',(29.310997085126,-3.43118498793819,-2.20169800725505));
#37774=CARTESIAN_POINT('Ctrl Pts',(29.5073423806783,-0.0484866765758729,
-4.07281664529234));
#37775=CARTESIAN_POINT('Ctrl Pts',(29.6382392443799,2.22123502507913,-2.88609404321281));
#37776=CARTESIAN_POINT('Ctrl Pts',(29.7036876762306,2.86105602751129,-1.94486468872292));
#37777=CARTESIAN_POINT('Ctrl Pts',(17.8633123237694,-1.6434304486251,3.31080057131684));
#37778=CARTESIAN_POINT('Ctrl Pts',(17.9287607556201,-2.73261662835048,2.77014531485408));
#37779=CARTESIAN_POINT('Ctrl Pts',(18.0596576193217,-4.31823628443353,0.539823285268273));
#37780=CARTESIAN_POINT('Ctrl Pts',(18.256002914874,-2.82858187503754,-3.31244745405465));
#37781=CARTESIAN_POINT('Ctrl Pts',(18.4523482104263,1.20346964446395,-4.18244757599994));
#37782=CARTESIAN_POINT('Ctrl Pts',(18.6486935059787,4.15350248723519,-1.30325413468162));
#37783=CARTESIAN_POINT('Ctrl Pts',(18.845038801531,3.37670769682809,2.74795372233073));
#37784=CARTESIAN_POINT('Ctrl Pts',(19.0413840970833,-0.431206192895155,
4.33165610591327));
#37785=CARTESIAN_POINT('Ctrl Pts',(19.2377293926357,-3.85185322141545,2.02827906346606));
#37786=CARTESIAN_POINT('Ctrl Pts',(19.434074688188,-3.81556479398536,-2.09580886962967));
#37787=CARTESIAN_POINT('Ctrl Pts',(19.6304199837403,-0.354711044094816,
-4.33873083513878));
#37788=CARTESIAN_POINT('Ctrl Pts',(19.8267652792926,3.42446384503687,-2.68769270155138));
#37789=CARTESIAN_POINT('Ctrl Pts',(20.023110574845,4.1301747351955,1.37561232416638));
#37790=CARTESIAN_POINT('Ctrl Pts',(20.2194558703973,1.12901391201524,4.20427313229795));
#37791=CARTESIAN_POINT('Ctrl Pts',(20.4158011659496,-2.88544061097913,3.25957875439539));
#37792=CARTESIAN_POINT('Ctrl Pts',(20.6121464615019,-4.31019311187138,-0.610617601320272));
#37793=CARTESIAN_POINT('Ctrl Pts',(20.8084917570543,-1.86651396742382,-3.932777147293));
#37794=CARTESIAN_POINT('Ctrl Pts',(21.0048370526066,2.25237472435964,-3.7252414460971));
#37795=CARTESIAN_POINT('Ctrl Pts',(21.2011823481589,4.34974065761324,-0.174273029640397));
#37796=CARTESIAN_POINT('Ctrl Pts',(21.3975276437112,2.54318179829341,3.53310632690612));
#37797=CARTESIAN_POINT('Ctrl Pts',(21.5938729392636,-1.54590157366968,4.06949665632978));
#37798=CARTESIAN_POINT('Ctrl Pts',(21.7902182348159,-4.24752681776928,0.953483332399067));
#37799=CARTESIAN_POINT('Ctrl Pts',(21.9865635303682,-3.13696509633072,-3.01828832693899));
#37800=CARTESIAN_POINT('Ctrl Pts',(22.1829088259205,0.789046142938758,-4.28112376882329));
#37801=CARTESIAN_POINT('Ctrl Pts',(22.3792541214728,4.00688260024406,-1.70161873979572));
#37802=CARTESIAN_POINT('Ctrl Pts',(22.5755994170252,3.62851208849374,2.40510176983027));
#37803=CARTESIAN_POINT('Ctrl Pts',(22.7719447125775,-0.00647503630907179,
4.35322553821067));
#37804=CARTESIAN_POINT('Ctrl Pts',(22.9682900081298,-3.63565076862356,2.3942969732266));
#37805=CARTESIAN_POINT('Ctrl Pts',(23.1646353036822,-4.00180286733272,-1.71353095038872));
#37806=CARTESIAN_POINT('Ctrl Pts',(23.3609805992345,-0.776307098369514,
-4.2834520888624));
#37807=CARTESIAN_POINT('Ctrl Pts',(23.5573258947868,3.14593007128556,-3.00894308592204));
#37808=CARTESIAN_POINT('Ctrl Pts',(23.7536711903391,4.24467157966798,0.966114738857153));
#37809=CARTESIAN_POINT('Ctrl Pts',(23.9500164858915,1.53378874262074,4.0740773925992));
#37810=CARTESIAN_POINT('Ctrl Pts',(24.1463617814438,-2.55368091032178,3.52552525391535));
#37811=CARTESIAN_POINT('Ctrl Pts',(24.3427070769961,-4.3492029335743,-0.18721204861699));
#37812=CARTESIAN_POINT('Ctrl Pts',(24.5390523725485,-2.24128294274079,-3.73192514361042));
#37813=CARTESIAN_POINT('Ctrl Pts',(24.7353976681008,1.87820517559581,-3.92720763720996));
#37814=CARTESIAN_POINT('Ctrl Pts',(24.9317429636531,4.31199016615752,-0.597792037071187));
#37815=CARTESIAN_POINT('Ctrl Pts',(25.1280882592054,2.87573187668868,3.26814636651764));
#37816=CARTESIAN_POINT('Ctrl Pts',(25.3244335547578,-1.14151717871423,4.20089907501512));
#37817=CARTESIAN_POINT('Ctrl Pts',(25.5207788503101,-4.13424607503771,1.36331358487529));
#37818=CARTESIAN_POINT('Ctrl Pts',(25.7171241458625,-3.41645832348522,-2.69785599393702));
#37819=CARTESIAN_POINT('Ctrl Pts',(25.9134694414147,0.36762618057702,-4.33767973969799));
#37820=CARTESIAN_POINT('Ctrl Pts',(26.1098147369671,3.82176350742396,-2.08440360887143));
#37821=CARTESIAN_POINT('Ctrl Pts',(26.3061600325194,3.84583952148144,2.03964025048695));
#37822=CARTESIAN_POINT('Ctrl Pts',(26.5025053280717,0.418246147672995,4.3330918565512));
#37823=CARTESIAN_POINT('Ctrl Pts',(26.6988506236241,-3.38472667816454,2.73756114904763));
#37824=CARTESIAN_POINT('Ctrl Pts',(26.8951959191764,-4.1498812911313,-1.3149508547382));
#37825=CARTESIAN_POINT('Ctrl Pts',(27.0915412147287,-1.19048814359663,-4.18728509855987));
#37826=CARTESIAN_POINT('Ctrl Pts',(27.287886510281,2.83738008319601,-3.30149896851051));
#37827=CARTESIAN_POINT('Ctrl Pts',(27.4842318058334,4.31867250924111,0.547405464360225));
#37828=CARTESIAN_POINT('Ctrl Pts',(27.6805771013857,1.92393598980375,3.90501253734012));
#37829=CARTESIAN_POINT('Ctrl Pts',(27.876922396938,-2.19757035780072,3.75783570775159));
#37830=CARTESIAN_POINT('Ctrl Pts',(28.0732676924903,-4.34669624373498,0.237985187117125));
#37831=CARTESIAN_POINT('Ctrl Pts',(28.2696129880427,-2.59471695542828,-3.49548186039235));
#37832=CARTESIAN_POINT('Ctrl Pts',(28.465958283595,1.48620969244535,-4.09168302153342));
#37833=CARTESIAN_POINT('Ctrl Pts',(28.6623035791473,4.23292180679059,-1.01565563961584));
#37834=CARTESIAN_POINT('Ctrl Pts',(28.8586488746997,3.18119835971342,2.97210052421617));
#37835=CARTESIAN_POINT('Ctrl Pts',(29.054994170252,-0.726927517204469,4.29204271131644));
#37836=CARTESIAN_POINT('Ctrl Pts',(29.2513394658043,-3.9801860331636,1.76049028754586));
#37837=CARTESIAN_POINT('Ctrl Pts',(29.4476847613566,-3.66599725731076,-2.35237064874011));
#37838=CARTESIAN_POINT('Ctrl Pts',(29.644030056909,-0.0518048499186609,
-4.35153881345912));
#37839=CARTESIAN_POINT('Ctrl Pts',(29.7749269206105,2.3732446773952,-3.08360315283289));
#37840=CARTESIAN_POINT('Ctrl Pts',(29.8403753524613,3.05685166691388,-2.07796100757108));
#37841=CARTESIAN_POINT('Ctrl Pts',(18.,-1.74869447533108,3.5228619944509));
#37842=CARTESIAN_POINT('Ctrl Pts',(18.0654484318508,-2.9076445584856,2.94757701002939));
#37843=CARTESIAN_POINT('Ctrl Pts',(18.1963452955523,-4.59482537887781,0.574399724304409));
#37844=CARTESIAN_POINT('Ctrl Pts',(18.3926905911047,-3.00975651390536,-3.52461436233937));
#37845=CARTESIAN_POINT('Ctrl Pts',(18.589035886657,1.28055356420065,-4.45033921309645));
#37846=CARTESIAN_POINT('Ctrl Pts',(18.7853811822093,4.41954015077335,-1.38672939105928));
#37847=CARTESIAN_POINT('Ctrl Pts',(18.9817264777616,3.59299056384847,2.92396401486012));
#37848=CARTESIAN_POINT('Ctrl Pts',(19.178071773314,-0.458825554726167,4.60910475875735));
#37849=CARTESIAN_POINT('Ctrl Pts',(19.3744170688663,-4.09856982612836,2.15819318406819));
#37850=CARTESIAN_POINT('Ctrl Pts',(19.5707623644186,-4.05995707399241,-2.23004836909123));
#37851=CARTESIAN_POINT('Ctrl Pts',(19.7671076599709,-0.37743078428812,-4.61663263431879));
#37852=CARTESIAN_POINT('Ctrl Pts',(19.9634529555233,3.64380556037334,-2.85984319112657));
#37853=CARTESIAN_POINT('Ctrl Pts',(20.1597982510756,4.39471822347621,1.46372222413157));
#37854=CARTESIAN_POINT('Ctrl Pts',(20.3561435466279,1.20132883759377,4.47356272690641));
#37855=CARTESIAN_POINT('Ctrl Pts',(20.5524888421803,-3.07025713168235,3.4683593482684));
#37856=CARTESIAN_POINT('Ctrl Pts',(20.7488341377326,-4.58626702982487,-0.649728515655752));
#37857=CARTESIAN_POINT('Ctrl Pts',(20.9451794332849,-1.98606680659531,-4.18467704303101));
#37858=CARTESIAN_POINT('Ctrl Pts',(21.1415247288372,2.39664248654891,-3.96384838890765));
#37859=CARTESIAN_POINT('Ctrl Pts',(21.3378700243896,4.62834765137447,-0.185435461772265));
#37860=CARTESIAN_POINT('Ctrl Pts',(21.5342153199419,2.70607616170119,3.75940674568056));
#37861=CARTESIAN_POINT('Ctrl Pts',(21.7305606154942,-1.64491873905791,4.33015362850052));
#37862=CARTESIAN_POINT('Ctrl Pts',(21.9269059110466,-4.51958687163654,1.01455527800489));
#37863=CARTESIAN_POINT('Ctrl Pts',(22.1232512065988,-3.33789211332263,-3.21161393029448));
#37864=CARTESIAN_POINT('Ctrl Pts',(22.3195965021512,0.83958565578034,-4.5553357545572));
#37865=CARTESIAN_POINT('Ctrl Pts',(22.5159417977035,4.26352905424683,-1.81060980821551));
#37866=CARTESIAN_POINT('Ctrl Pts',(22.7122870932558,3.86092338019503,2.55915191362662));
#37867=CARTESIAN_POINT('Ctrl Pts',(22.9086323888082,-0.00688977147203868,
4.63205574346503));
#37868=CARTESIAN_POINT('Ctrl Pts',(23.1049776843605,-3.86851930280594,2.54765505463652));
#37869=CARTESIAN_POINT('Ctrl Pts',(23.3013229799128,-4.25812395731338,-1.82328501261516));
#37870=CARTESIAN_POINT('Ctrl Pts',(23.4976682754651,-0.826030657527862,
-4.55781320676248));
#37871=CARTESIAN_POINT('Ctrl Pts',(23.6940135710175,3.3474313075052,-3.20167011347485));
#37872=CARTESIAN_POINT('Ctrl Pts',(23.8903588665698,4.51654875152767,1.02799574377413));
#37873=CARTESIAN_POINT('Ctrl Pts',(24.0867041621221,1.63203006418057,4.33502776735682));
#37874=CARTESIAN_POINT('Ctrl Pts',(24.2830494576745,-2.71724775658992,3.75134009432509));
#37875=CARTESIAN_POINT('Ctrl Pts',(24.4793947532267,-4.62777548535616,-0.199203243073542));
#37876=CARTESIAN_POINT('Ctrl Pts',(24.6757400487791,-2.38484026075065,-3.97096018662691));
#37877=CARTESIAN_POINT('Ctrl Pts',(24.8720853443314,1.99850685305871,-4.17875079801063));
#37878=CARTESIAN_POINT('Ctrl Pts',(25.0684306398838,4.58817918796009,-0.636081456016511));
#37879=CARTESIAN_POINT('Ctrl Pts',(25.2647759354361,3.05992653933489,3.47747572797129));
#37880=CARTESIAN_POINT('Ctrl Pts',(25.4611212309884,-1.2146329560725,4.4699725565193));
#37881=CARTESIAN_POINT('Ctrl Pts',(25.6574665265407,-4.39905033834923,1.45063573332825));
#37882=CARTESIAN_POINT('Ctrl Pts',(25.8538118220931,-3.63528727393098,-2.87065745665316));
#37883=CARTESIAN_POINT('Ctrl Pts',(26.0501571176454,0.391173153387717,-4.61551421473986));
#37884=CARTESIAN_POINT('Ctrl Pts',(26.2465024131977,4.06655282372633,-2.21791258537474));
#37885=CARTESIAN_POINT('Ctrl Pts',(26.44284770875,4.09217094027366,2.1702820710626));
#37886=CARTESIAN_POINT('Ctrl Pts',(26.6391930043024,0.445035400418794,4.61063247123866));
#37887=CARTESIAN_POINT('Ctrl Pts',(26.8355382998547,-3.60152317219375,2.9129057826728));
#37888=CARTESIAN_POINT('Ctrl Pts',(27.031883595407,-4.41568701197684,-1.39917530245121));
#37889=CARTESIAN_POINT('Ctrl Pts',(27.2282288909594,-1.26674057998394,-4.45548658576556));
#37890=CARTESIAN_POINT('Ctrl Pts',(27.4245741865117,3.0191182596442,-3.51296461093051));
#37891=CARTESIAN_POINT('Ctrl Pts',(27.620919482064,4.59528954449653,0.582467552608381));
#37892=CARTESIAN_POINT('Ctrl Pts',(27.8172647776163,2.04716679009758,4.15513407084441));
#37893=CARTESIAN_POINT('Ctrl Pts',(28.0136100731686,-2.33832782339674,3.99853035876552));
#37894=CARTESIAN_POINT('Ctrl Pts',(28.209955368721,-4.62510823851462,0.253228472352165));
#37895=CARTESIAN_POINT('Ctrl Pts',(28.4063006642733,-2.76091221797754,-3.71937237928253));
#37896=CARTESIAN_POINT('Ctrl Pts',(28.6026459598257,1.58140350906662,-4.35376106153289));
#37897=CARTESIAN_POINT('Ctrl Pts',(28.798991255378,4.50404638920727,-1.08070980875459));
#37898=CARTESIAN_POINT('Ctrl Pts',(28.9953365509303,3.38495857930413,3.16246773398503));
#37899=CARTESIAN_POINT('Ctrl Pts',(29.1916818464826,-0.773488244887422,
4.56695407064121));
#37900=CARTESIAN_POINT('Ctrl Pts',(29.3880271420349,-4.23512253457759,1.8732521612223));
#37901=CARTESIAN_POINT('Ctrl Pts',(29.5843724375873,-3.90080952668333,-2.50304329022518));
#37902=CARTESIAN_POINT('Ctrl Pts',(29.7807177331396,-0.0551230232614539,
-4.6302609816259));
#37903=CARTESIAN_POINT('Ctrl Pts',(29.9116145968412,2.52525432971127,-3.28111226245297));
#37904=CARTESIAN_POINT('Ctrl Pts',(29.9770630286919,3.25264730631648,-2.21105732641923));
#37905=CARTESIAN_POINT('Ctrl Pts',(29.470836477965,-3.9278981228736,0.00143380487199485));
#37906=CARTESIAN_POINT('Ctrl Pts',(29.50289098531,-3.92594160481835,-0.634441539882881));
#37907=CARTESIAN_POINT('Ctrl Pts',(29.534945492655,-3.77702635946811,-1.27129224464512));
#37908=CARTESIAN_POINT('Ctrl Pts',(29.567,-3.48672441430162,-1.83213518456555));
#37909=CARTESIAN_POINT('',(18.,-1.871586531739,-2.6236008493506));
#37910=CARTESIAN_POINT('Ctrl Pts',(18.,-1.87548423476387,-2.62663505508783));
#37911=CARTESIAN_POINT('Ctrl Pts',(18.,-1.95820209882815,-2.5806971131868));
#37912=CARTESIAN_POINT('Ctrl Pts',(18.,-2.03859008372278,-2.53101906286817));
#37913=CARTESIAN_POINT('Ctrl Pts',(18.,-2.11635819108058,-2.47766066360094));
#37914=CARTESIAN_POINT('Ctrl Pts',(18.,-2.20135601840208,-2.41934179535073));
#37915=CARTESIAN_POINT('Ctrl Pts',(18.,-2.28322550321657,-2.35662754124991));
#37916=CARTESIAN_POINT('Ctrl Pts',(18.,-2.3618759087473,-2.28990546259509));
#37917=CARTESIAN_POINT('Ctrl Pts',(18.,-2.4106981454921,-2.24848773438112));
#37918=CARTESIAN_POINT('Ctrl Pts',(18.,-2.45827961310671,-2.20552464637135));
#37919=CARTESIAN_POINT('Ctrl Pts',(18.,-2.50459424286804,-2.16110001301956));
#37920=CARTESIAN_POINT('Ctrl Pts',(18.,-2.51914286810609,-2.14714508462428));
#37921=CARTESIAN_POINT('Ctrl Pts',(18.,-2.53356646013624,-2.13304589193832));
#37922=CARTESIAN_POINT('Ctrl Pts',(18.,-2.54786413133718,-2.11880491015565));
#37923=CARTESIAN_POINT('Ctrl Pts',(18.,-2.5610050207126,-2.10571612362718));
#37924=CARTESIAN_POINT('Ctrl Pts',(18.,-2.57403244485455,-2.09251462753296));
#37925=CARTESIAN_POINT('Ctrl Pts',(18.,-2.58694576270026,-2.07920297048157));
#37926=CARTESIAN_POINT('Ctrl Pts',(18.,-2.66074697646445,-2.00312519873119));
#37927=CARTESIAN_POINT('Ctrl Pts',(18.,-2.73082522813611,-1.92345089854155));
#37928=CARTESIAN_POINT('Ctrl Pts',(18.,-2.79708762582428,-1.8405877306472));
#37929=CARTESIAN_POINT('Ctrl Pts',(18.,-2.86107601659434,-1.76056827839887));
#37930=CARTESIAN_POINT('Ctrl Pts',(18.,-2.92150620456706,-1.67757429735906));
#37931=CARTESIAN_POINT('Ctrl Pts',(18.,-2.97827186634913,-1.5919350994066));
#37932=CARTESIAN_POINT('Ctrl Pts',(18.,-3.0040065994896,-1.55311053828141));
#37933=CARTESIAN_POINT('Ctrl Pts',(18.,-3.0289878389067,-1.51374185880171));
#37934=CARTESIAN_POINT('Ctrl Pts',(18.,-3.05320386225338,-1.47385768533847));
#37935=CARTESIAN_POINT('Ctrl Pts',(18.,-3.06286630348485,-1.45794349180484));
#37936=CARTESIAN_POINT('Ctrl Pts',(18.,-3.07240777935416,-1.44194571330402));
#37937=CARTESIAN_POINT('Ctrl Pts',(18.,-3.08182473371469,-1.42587083068939));
#37938=CARTESIAN_POINT('Ctrl Pts',(18.,-3.13788269968003,-1.33017904032833));
#37939=CARTESIAN_POINT('Ctrl Pts',(18.,-3.1893801972824,-1.23201678777164));
#37940=CARTESIAN_POINT('Ctrl Pts',(18.,-3.23622158101597,-1.13181604397664));
#37941=CARTESIAN_POINT('Ctrl Pts',(18.,-3.2838680580919,-1.02989308479643));
#37942=CARTESIAN_POINT('Ctrl Pts',(18.,-3.32669756400407,-0.925860308419108));
#37943=CARTESIAN_POINT('Ctrl Pts',(18.,-3.36457639323085,-0.820129668363867));
#37944=CARTESIAN_POINT('Ctrl Pts',(18.,-3.40248383253285,-0.714319169410486));
#37945=CARTESIAN_POINT('Ctrl Pts',(18.,-3.43543362560168,-0.60680744101958));
#37946=CARTESIAN_POINT('Ctrl Pts',(18.,-3.46325088941741,-0.497976121629401));
#37947=CARTESIAN_POINT('Ctrl Pts',(18.,-3.48290184612153,-0.421094385181289));
#37948=CARTESIAN_POINT('Ctrl Pts',(18.,-3.49999061070311,-0.343553440328808));
#37949=CARTESIAN_POINT('Ctrl Pts',(18.,-3.51444110805291,-0.265481772395751));
#37950=CARTESIAN_POINT('Ctrl Pts',(18.,-3.51875517528347,-0.242174171549102));
#37951=CARTESIAN_POINT('Ctrl Pts',(18.,-3.5228340150811,-0.218819245089493));
#37952=CARTESIAN_POINT('Ctrl Pts',(18.,-3.52667537469033,-0.195420359771128));
#37953=CARTESIAN_POINT('Ctrl Pts',(18.,-3.52997474417659,-0.175322900515618));
#37954=CARTESIAN_POINT('Ctrl Pts',(18.,-3.53309932126695,-0.155189617330016));
#37955=CARTESIAN_POINT('Ctrl Pts',(18.,-3.53604413380429,-0.135048340030048));
#37956=CARTESIAN_POINT('Ctrl Pts',(18.,-3.55280836711581,-0.0203880458457306));
#37957=CARTESIAN_POINT('Ctrl Pts',(18.,-3.56377865807533,0.0946897512260063));
#37958=CARTESIAN_POINT('Ctrl Pts',(18.,-3.56881809050027,0.209758022820131));
#37959=CARTESIAN_POINT('Ctrl Pts',(18.,-3.57221961033072,0.287426890001854));
#37960=CARTESIAN_POINT('Ctrl Pts',(18.,-3.57291822578798,0.365092165535591));
#37961=CARTESIAN_POINT('Ctrl Pts',(18.,-3.57086003709278,0.442628950421449));
#37962=CARTESIAN_POINT('Ctrl Pts',(18.,-3.56790903708174,0.55380002700326));
#37963=CARTESIAN_POINT('Ctrl Pts',(18.,-3.55929342003541,0.664706972490521));
#37964=CARTESIAN_POINT('Ctrl Pts',(18.,-3.54527493044651,0.775065658256069));
#37965=CARTESIAN_POINT('Ctrl Pts',(18.,-3.53100071169589,0.887437537669873));
#37966=CARTESIAN_POINT('Ctrl Pts',(18.,-3.5111245897341,0.99924165895933));
#37967=CARTESIAN_POINT('Ctrl Pts',(18.,-3.48586888045152,1.1101799969906));
#37968=CARTESIAN_POINT('Ctrl Pts',(18.,-3.47993938872303,1.13622590805053));
#37969=CARTESIAN_POINT('Ctrl Pts',(18.,-3.47371314341635,1.16222407852405));
#37970=CARTESIAN_POINT('Ctrl Pts',(18.,-3.4671926118425,1.18817060124356));
#37971=CARTESIAN_POINT('Ctrl Pts',(18.,-3.46255239536067,1.20663496737776));
#37972=CARTESIAN_POINT('Ctrl Pts',(18.,-3.45776266140388,1.22507464083751));
#37973=CARTESIAN_POINT('Ctrl Pts',(18.,-3.45282996231712,1.24346791507144));
#37974=CARTESIAN_POINT('Ctrl Pts',(18.,-3.42331447864212,1.35352660217804));
#37975=CARTESIAN_POINT('Ctrl Pts',(18.,-3.38864432210052,1.46208840194843));
#37976=CARTESIAN_POINT('Ctrl Pts',(18.,-3.34912202183174,1.56886148963333));
#37977=CARTESIAN_POINT('Ctrl Pts',(18.,-3.30832864479712,1.67906850677204));
#37978=CARTESIAN_POINT('Ctrl Pts',(18.,-3.26236597176655,1.78737060465608));
#37979=CARTESIAN_POINT('Ctrl Pts',(18.,-3.21151133264799,1.8934501250158));
#37980=CARTESIAN_POINT('Ctrl Pts',(18.,-3.16017558190922,2.00053321340384));
#37981=CARTESIAN_POINT('Ctrl Pts',(18.,-3.10385460122732,2.10535227079503));
#37982=CARTESIAN_POINT('Ctrl Pts',(18.,-3.04278075082353,2.20757233088601));
#37983=CARTESIAN_POINT('Ctrl Pts',(18.,-3.0029883232406,2.27417340993702));
#37984=CARTESIAN_POINT('Ctrl Pts',(18.,-2.96117717331697,2.33967099054269));
#37985=CARTESIAN_POINT('Ctrl Pts',(18.,-2.91740050634391,2.40396807347353));
#37986=CARTESIAN_POINT('Ctrl Pts',(18.,-2.90268894811113,2.4255757093476));
#37987=CARTESIAN_POINT('Ctrl Pts',(18.,-2.88775534320413,2.4470477289152));
#37988=CARTESIAN_POINT('Ctrl Pts',(18.,-2.87260150486414,2.46838032818946));
#37989=CARTESIAN_POINT('Ctrl Pts',(18.,-2.86324620498797,2.48155011784085));
#37990=CARTESIAN_POINT('Ctrl Pts',(18.,-2.85380696612941,2.49466676929328));
#37991=CARTESIAN_POINT('Ctrl Pts',(18.,-2.84428419596223,2.50772937397784));
#37992=CARTESIAN_POINT('Ctrl Pts',(18.,-2.83435634685015,2.52134763484544));
#37993=CARTESIAN_POINT('Ctrl Pts',(18.,-2.8243432924092,2.53489947693834));
#37994=CARTESIAN_POINT('Ctrl Pts',(18.,-2.81424721466029,2.54838219855492));
#37995=CARTESIAN_POINT('Ctrl Pts',(18.,-2.74081393044342,2.64644805671393));
#37996=CARTESIAN_POINT('Ctrl Pts',(18.,-2.66296950811265,2.74088992939784));
#37997=CARTESIAN_POINT('Ctrl Pts',(18.,-2.58100499690223,2.83137492858441));
#37998=CARTESIAN_POINT('Ctrl Pts',(18.,-2.49888770204909,2.92202859378974));
#37999=CARTESIAN_POINT('Ctrl Pts',(18.,-2.41263455998783,3.0087114479034));
#38000=CARTESIAN_POINT('Ctrl Pts',(18.,-2.32248838717186,3.09107247079346));
#38001=CARTESIAN_POINT('Ctrl Pts',(18.,-2.23401847417333,3.17190199801509));
#38002=CARTESIAN_POINT('Ctrl Pts',(18.,-2.14179846071257,3.24856963213308));
#38003=CARTESIAN_POINT('Ctrl Pts',(18.,-2.04601671705284,3.32071669612736));
#38004=CARTESIAN_POINT('Ctrl Pts',(18.,-1.95040779378605,3.3927335841249));
#38005=CARTESIAN_POINT('Ctrl Pts',(18.,-1.85124960611979,3.4602469787051));
#38006=CARTESIAN_POINT('Ctrl Pts',(18.,-1.74869447533108,3.5228619944509));
#38007=CARTESIAN_POINT('Ctrl Pts',(18.,-1.87548423476386,-2.62663505508783));
#38008=CARTESIAN_POINT('Ctrl Pts',(18.0596576193217,-1.08825137675884,-3.18144260266452));
#38009=CARTESIAN_POINT('Ctrl Pts',(18.1847636704941,1.12516150761905,-3.57262622497546));
#38010=CARTESIAN_POINT('Ctrl Pts',(18.3753181535174,3.62142716015887,-1.1363036219263));
#38011=CARTESIAN_POINT('Ctrl Pts',(18.5716634490697,2.94414196278733,2.39593313727195));
#38012=CARTESIAN_POINT('Ctrl Pts',(18.768008744622,-0.375967469233134,3.77675880022508));
#38013=CARTESIAN_POINT('Ctrl Pts',(18.9310454113565,-2.85246745308514,2.10914645645945));
#38014=CARTESIAN_POINT('Ctrl Pts',(19.0286336462402,-3.21794887923582,0.522734302530077));
#38015=CARTESIAN_POINT('Ctrl Pts',(19.0607734492731,-3.21773234909139,0.000164702477305698));
#38016=CARTESIAN_POINT('Origin',(15.6892265507269,0.,0.));
#38017=CARTESIAN_POINT('',(18.,1.87158653173903,-2.62360084935058));
#38018=CARTESIAN_POINT('Origin',(18.,0.,0.));
#38019=CARTESIAN_POINT('Ctrl Pts',(18.,1.87158653173903,-2.62360084935058));
#38020=CARTESIAN_POINT('Ctrl Pts',(18.0654484318508,2.73469795288145,-2.00788687304197));
#38021=CARTESIAN_POINT('Ctrl Pts',(18.1963452955523,3.79210558070424,0.130964326648123));
#38022=CARTESIAN_POINT('Ctrl Pts',(18.3926905911047,1.97820456802146,3.24194700629428));
#38023=CARTESIAN_POINT('Ctrl Pts',(18.589035886657,-1.6130627898401,3.43470578559991));
#38024=CARTESIAN_POINT('Ctrl Pts',(18.7295478731977,-3.14634040634608,1.36959129364314));
#38025=CARTESIAN_POINT('Ctrl Pts',(18.8046114278877,-3.22658417899954,0.157881475370533));
#38026=CARTESIAN_POINT('Ctrl Pts',(18.8142265507269,-3.22532168306538,0.00249477058570481));
#38027=CARTESIAN_POINT('Ctrl Pts',(17.5899369713081,2.28405859260864,-3.20180657528381));
#38028=CARTESIAN_POINT('Ctrl Pts',(17.6553854031588,3.3373879601839,-2.45039766400564));
#38029=CARTESIAN_POINT('Ctrl Pts',(17.7862822668604,4.6278337596493,0.159827072129988));
#38030=CARTESIAN_POINT('Ctrl Pts',(17.9826275624127,2.41417378513026,3.95642776379034));
#38031=CARTESIAN_POINT('Ctrl Pts',(18.178972857965,-1.96855975562516,4.19166794035048));
#38032=CARTESIAN_POINT('Ctrl Pts',(18.3753181535174,-4.58328013121786,0.669998490589778));
#38033=CARTESIAN_POINT('Ctrl Pts',(18.5716634490697,-3.0850987443137,-3.45562037537898));
#38034=CARTESIAN_POINT('Ctrl Pts',(18.768008744622,1.18230356479204,-4.47845017961223));
#38035=CARTESIAN_POINT('Ctrl Pts',(18.9643540401743,4.38841430798082,-1.48252773677679));
#38036=CARTESIAN_POINT('Ctrl Pts',(19.1606993357267,3.65597544705728,2.84432883466346));
#38037=CARTESIAN_POINT('Ctrl Pts',(19.357044631279,-0.35777220904007,4.61819705076657));
#38038=CARTESIAN_POINT('Ctrl Pts',(19.5533899268313,-4.05039424390049,2.24729253433311));
#38039=CARTESIAN_POINT('Ctrl Pts',(19.7497352223837,-4.10776879369746,-2.14062178900008));
#38040=CARTESIAN_POINT('Ctrl Pts',(19.946080517936,-0.478384358520377,-4.60728745225425));
#38041=CARTESIAN_POINT('Ctrl Pts',(20.1424258134883,3.58035056501647,-2.93889099413954));
#38042=CARTESIAN_POINT('Ctrl Pts',(20.3387711090406,4.42569575871567,1.36718851931307));
#38043=CARTESIAN_POINT('Ctrl Pts',(20.535116404593,1.2989452578469,4.44620281532906));
#38044=CARTESIAN_POINT('Ctrl Pts',(20.7314617001453,-2.99361787167454,3.53471869813215));
#38045=CARTESIAN_POINT('Ctrl Pts',(20.9278069956976,-4.59938688433903,-0.549202649241384));
#38046=CARTESIAN_POINT('Ctrl Pts',(21.1241522912499,-2.07717181620429,-4.14021007709899));
#38047=CARTESIAN_POINT('Ctrl Pts',(21.3204975868023,2.30932036632879,-4.01534836843555));
#38048=CARTESIAN_POINT('Ctrl Pts',(21.5168428823546,4.62318035521908,-0.28668148433296));
#38049=CARTESIAN_POINT('Ctrl Pts',(21.7131881779069,2.78770153983615,3.69928410501389));
#38050=CARTESIAN_POINT('Ctrl Pts',(21.9095334734592,-1.54976015515307,4.36511469950787));
#38051=CARTESIAN_POINT('Ctrl Pts',(22.1058787690116,-4.49630057640805,1.11322233560676));
#38052=CARTESIAN_POINT('Ctrl Pts',(22.3022240645639,-3.40737775223363,-3.13779535441328));
#38053=CARTESIAN_POINT('Ctrl Pts',(22.4985693601163,0.739691972350024,-4.57261835642576));
#38054=CARTESIAN_POINT('Ctrl Pts',(22.6949146556685,4.22288264507703,-1.90348233703615));
#38055=CARTESIAN_POINT('Ctrl Pts',(22.891259951221,3.9160047031351,2.47404325063253));
#38056=CARTESIAN_POINT('Ctrl Pts',(23.0876052467732,0.0944833846028492,
4.63109660154791));
#38057=CARTESIAN_POINT('Ctrl Pts',(23.2839505423256,-3.8118374751247,2.63170627257853));
#38058=CARTESIAN_POINT('Ctrl Pts',(23.4802958378779,-4.29700582080243,-1.72966002961468));
#38059=CARTESIAN_POINT('Ctrl Pts',(23.6766411334302,-0.925579449979732,
-4.53864357752752));
#38060=CARTESIAN_POINT('Ctrl Pts',(23.8729864289826,3.27656136831225,-3.2741607232355));
#38061=CARTESIAN_POINT('Ctrl Pts',(24.0693317245348,4.53796396384225,0.928905757170099));
#38062=CARTESIAN_POINT('Ctrl Pts',(24.2656770200872,1.72651011524057,4.29827240446072));
#38063=CARTESIAN_POINT('Ctrl Pts',(24.4620223156395,-2.63449941555764,3.80990756724199));
#38064=CARTESIAN_POINT('Ctrl Pts',(24.6583676111919,-4.63102610742726,-0.0978776777820504));
#38065=CARTESIAN_POINT('Ctrl Pts',(24.8547129067441,-2.47117238664086,-3.91781697736097));
#38066=CARTESIAN_POINT('Ctrl Pts',(25.0510582022965,1.90657694565293,-4.22148637238187));
#38067=CARTESIAN_POINT('Ctrl Pts',(25.2474034978488,4.57315928208664,-0.736340314681052));
#38068=CARTESIAN_POINT('Ctrl Pts',(25.4437487934011,3.1352970992814,3.40967665095255));
#38069=CARTESIAN_POINT('Ctrl Pts',(25.6400940889535,-1.11651754358445,4.49548344955368));
#38070=CARTESIAN_POINT('Ctrl Pts',(25.8364393845058,-4.36624943602384,1.54656035661739));
#38071=CARTESIAN_POINT('Ctrl Pts',(26.0327846800581,-3.69723983944396,-2.79041212120608));
#38072=CARTESIAN_POINT('Ctrl Pts',(26.2291299756104,0.290069821214124,-4.62296904170733));
#38073=CARTESIAN_POINT('Ctrl Pts',(26.4254752711628,4.01704008353218,-2.30637663962979));
#38074=CARTESIAN_POINT('Ctrl Pts',(26.6218205667151,4.13868613388374,2.08020560116578));
#38075=CARTESIAN_POINT('Ctrl Pts',(26.8181658622674,0.545832179724393,4.59978854162153));
#38076=CARTESIAN_POINT('Ctrl Pts',(27.0145111578198,-3.5369133624434,2.99102562851232));
#38077=CARTESIAN_POINT('Ctrl Pts',(27.2108564533721,-4.44524670958994,-1.30220234720116));
#38078=CARTESIAN_POINT('Ctrl Pts',(27.4072017489244,-1.36394995233954,-4.42669929332562));
#38079=CARTESIAN_POINT('Ctrl Pts',(27.6035470444767,2.94152523715434,-3.57819040089757));
#38080=CARTESIAN_POINT('Ctrl Pts',(27.799892340029,4.60691446598188,0.481751031547769));
#38081=CARTESIAN_POINT('Ctrl Pts',(27.9962376355814,2.13765158660013,4.1093562371118));
#38082=CARTESIAN_POINT('Ctrl Pts',(28.1925829311337,-2.25034069347583,4.04870786697312));
#38083=CARTESIAN_POINT('Ctrl Pts',(28.388928226686,-4.61830214982256,0.354461540273715));
#38084=CARTESIAN_POINT('Ctrl Pts',(28.5852735222383,-2.84195199611733,-3.65820383421496));
#38085=CARTESIAN_POINT('Ctrl Pts',(28.7816188177907,1.48633510618651,-4.387044869924));
#38086=CARTESIAN_POINT('Ctrl Pts',(28.977964113343,4.47816070641504,-1.17956954909381));
#38087=CARTESIAN_POINT('Ctrl Pts',(29.1743094088954,3.45564326691785,3.08870285503582));
#38088=CARTESIAN_POINT('Ctrl Pts',(29.3706547044476,-0.678183987680962,
4.58066113992167));
#38089=CARTESIAN_POINT('Ctrl Pts',(29.5015515681492,-3.01258675481066,2.84023382017821));
#38090=CARTESIAN_POINT('Ctrl Pts',(29.567,-3.56151197810524,1.66856867698424));
#38091=CARTESIAN_POINT('Ctrl Pts',(17.7266246475387,2.1465679056521,-3.00907133330607));
#38092=CARTESIAN_POINT('Ctrl Pts',(17.7920730793895,3.13649129108308,-2.30289406701775));
#38093=CARTESIAN_POINT('Ctrl Pts',(17.9229699430911,4.34925770000094,0.150206156969366));
#38094=CARTESIAN_POINT('Ctrl Pts',(18.1193152386434,2.26885071276066,3.71826751129165));
#38095=CARTESIAN_POINT('Ctrl Pts',(18.3156605341957,-1.85006076703014,3.93934722210029));
#38096=CARTESIAN_POINT('Ctrl Pts',(18.512005829748,-4.30738601195373,0.629667409316655));
#38097=CARTESIAN_POINT('Ctrl Pts',(18.7083511253003,-2.899388821172,-3.24760661390658));
#38098=CARTESIAN_POINT('Ctrl Pts',(18.9046964208527,1.11113388033629,-4.20886638097933));
#38099=CARTESIAN_POINT('Ctrl Pts',(19.101041716405,4.12425028880603,-1.3932858243227));
#38100=CARTESIAN_POINT('Ctrl Pts',(19.2973870119573,3.43590115590782,2.67311224386597));
#38101=CARTESIAN_POINT('Ctrl Pts',(19.4937323075096,-0.336235832103842,
4.34020108031933));
#38102=CARTESIAN_POINT('Ctrl Pts',(19.690077603062,-3.80657760590318,2.11201500890636));
#38103=CARTESIAN_POINT('Ctrl Pts',(19.8864228986143,-3.86049844996293,-2.01176539221754));
#38104=CARTESIAN_POINT('Ctrl Pts',(20.0827681941666,-0.449587639252706,
-4.32994819359135));
#38105=CARTESIAN_POINT('Ctrl Pts',(20.2791134897189,3.36482857257619,-2.76198216045975));
#38106=CARTESIAN_POINT('Ctrl Pts',(20.4754587852713,4.15928755356033,1.28488954093846));
#38107=CARTESIAN_POINT('Ctrl Pts',(20.6718040808236,1.22075423577842,4.17856017191967));
#38108=CARTESIAN_POINT('Ctrl Pts',(20.868149376376,-2.81341471095273,3.32194355148002));
#38109=CARTESIAN_POINT('Ctrl Pts',(21.0644946719282,-4.32252320651873,-0.516142967774858));
#38110=CARTESIAN_POINT('Ctrl Pts',(21.2608399674806,-1.95213483998095,-3.89098690502851));
#38111=CARTESIAN_POINT('Ctrl Pts',(21.4571852630329,2.17030902721659,-3.77364134422321));
#38112=CARTESIAN_POINT('Ctrl Pts',(21.6535305585852,4.34488441087682,-0.269424468971688));
#38113=CARTESIAN_POINT('Ctrl Pts',(21.8498758541376,2.6198936731806,3.47660281544816));
#38114=CARTESIAN_POINT('Ctrl Pts',(22.0462211496899,-1.45647113488039,4.10235321842256));
#38115=CARTESIAN_POINT('Ctrl Pts',(22.2425664452422,-4.22564225922916,1.04621104957702));
#38116=CARTESIAN_POINT('Ctrl Pts',(22.4389117407945,-3.20226799305709,-2.94891331776001));
#38117=CARTESIAN_POINT('Ctrl Pts',(22.6352570363469,0.695165637630007,-4.29736603100399));
#38118=CARTESIAN_POINT('Ctrl Pts',(22.8316023318991,3.96868293335011,-1.78890073436812));
#38119=CARTESIAN_POINT('Ctrl Pts',(23.0279476274516,3.68027774827436,2.32511628913057));
#38120=CARTESIAN_POINT('Ctrl Pts',(23.2242929230038,0.0887958836354571,
4.35232413258873));
#38121=CARTESIAN_POINT('Ctrl Pts',(23.4206382185562,-3.58238094773194,2.47328866260319));
#38122=CARTESIAN_POINT('Ctrl Pts',(23.6169835141085,-4.03834420674827,-1.62554179620221));
#38123=CARTESIAN_POINT('Ctrl Pts',(23.8133288096608,-0.869863473681043,
-4.2654363903982));
#38124=CARTESIAN_POINT('Ctrl Pts',(24.0096741052132,3.07932620331151,-3.07707006693597));
#38125=CARTESIAN_POINT('Ctrl Pts',(24.2060194007655,4.26479768658833,0.872989551217906));
#38126=CARTESIAN_POINT('Ctrl Pts',(24.4023646963178,1.62258149337857,4.03953454741621));
#38127=CARTESIAN_POINT('Ctrl Pts',(24.5987099918701,-2.47591367016399,3.5805672121582));
#38128=CARTESIAN_POINT('Ctrl Pts',(24.7950552874225,-4.3522578819166,-0.091985854691575));
#38129=CARTESIAN_POINT('Ctrl Pts',(24.9914005829748,-2.32241823903413,-3.68198093124091));
#38130=CARTESIAN_POINT('Ctrl Pts',(25.1877458785272,1.7918090606076,-3.96737071037795));
#38131=CARTESIAN_POINT('Ctrl Pts',(25.3840911740794,4.29787439522318,-0.692015735606349));
#38132=CARTESIAN_POINT('Ctrl Pts',(25.5804364696318,2.94656544704267,3.20442850777609));
#38133=CARTESIAN_POINT('Ctrl Pts',(25.7767817651841,-1.04930789994255,4.22487431996257));
#38134=CARTESIAN_POINT('Ctrl Pts',(25.9731270607364,-4.10341964858966,1.45346395071116));
#38135=CARTESIAN_POINT('Ctrl Pts',(26.1694723562888,-3.4746816060373,-2.62244108899263));
#38136=CARTESIAN_POINT('Ctrl Pts',(26.3658176518411,0.272608842273773,-4.34468581754659));
#38137=CARTESIAN_POINT('Ctrl Pts',(26.5621629473934,3.77523122521125,-2.16754250044026));
#38138=CARTESIAN_POINT('Ctrl Pts',(26.7585082429457,3.88955469676272,1.95498600389246));
#38139=CARTESIAN_POINT('Ctrl Pts',(26.9548535384981,0.512975386297035,4.32290068572809));
#38140=CARTESIAN_POINT('Ctrl Pts',(27.1511988340504,-3.32400610626277,2.81097850988778));
#38141=CARTESIAN_POINT('Ctrl Pts',(27.3475441296027,-4.1776616197106,-1.22381526210078));
#38142=CARTESIAN_POINT('Ctrl Pts',(27.543889425155,-1.28184592202771,-4.16023067962239));
#38143=CARTESIAN_POINT('Ctrl Pts',(27.7402347207074,2.76445783316343,-3.36279844121984));
#38144=CARTESIAN_POINT('Ctrl Pts',(27.9365800162597,4.32959765951831,0.452751652773583));
#38145=CARTESIAN_POINT('Ctrl Pts',(28.132925311812,2.00897398346573,3.86199033598386));
#38146=CARTESIAN_POINT('Ctrl Pts',(28.3292706073643,-2.11487968173407,3.80499274174914));
#38147=CARTESIAN_POINT('Ctrl Pts',(28.5256159029167,-4.34029985285574,0.333124451623868));
#38148=CARTESIAN_POINT('Ctrl Pts',(28.721961198469,-2.67087848096839,-3.43799540356397));
#38149=CARTESIAN_POINT('Ctrl Pts',(28.9183064940213,1.39686400616373,-4.12296328514024));
#38150=CARTESIAN_POINT('Ctrl Pts',(29.1146517895736,4.20859433284684,-1.10856444084362));
#38151=CARTESIAN_POINT('Ctrl Pts',(29.310997085126,3.24762812747141,2.90277597964053));
#38152=CARTESIAN_POINT('Ctrl Pts',(29.5073423806783,-0.637360174031477,
4.3049246728796));
#38153=CARTESIAN_POINT('Ctrl Pts',(29.6382392443799,-2.83124174738595,2.6692637319689));
#38154=CARTESIAN_POINT('Ctrl Pts',(29.7036876762306,-3.34712398908505,1.56812788515203));
#38155=CARTESIAN_POINT('Ctrl Pts',(17.8633123237694,2.00907721869556,-2.81633609132832));
#38156=CARTESIAN_POINT('Ctrl Pts',(17.9287607556201,2.93559462198226,-2.15539047002986));
#38157=CARTESIAN_POINT('Ctrl Pts',(18.0596576193217,4.07068164035259,0.140585241808746));
#38158=CARTESIAN_POINT('Ctrl Pts',(18.256002914874,2.12352764039106,3.48010725879296));
#38159=CARTESIAN_POINT('Ctrl Pts',(18.4523482104263,-1.73156177843512,3.6870265038501));
#38160=CARTESIAN_POINT('Ctrl Pts',(18.6486935059787,-4.0314918926896,0.589336328043536));
#38161=CARTESIAN_POINT('Ctrl Pts',(18.845038801531,-2.7136788980303,-3.03959285243419));
#38162=CARTESIAN_POINT('Ctrl Pts',(19.0413840970833,1.03996419588054,-3.93928258234643));
#38163=CARTESIAN_POINT('Ctrl Pts',(19.2377293926356,3.86008626963124,-1.3040439118686));
#38164=CARTESIAN_POINT('Ctrl Pts',(19.434074688188,3.21582686475836,2.50189565306848));
#38165=CARTESIAN_POINT('Ctrl Pts',(19.6304199837403,-0.314699455167615,
4.06220510987209));
#38166=CARTESIAN_POINT('Ctrl Pts',(19.8267652792926,-3.56276096790587,1.97673748347961));
#38167=CARTESIAN_POINT('Ctrl Pts',(20.0231105748449,-3.61322810622841,-1.882908995435));
#38168=CARTESIAN_POINT('Ctrl Pts',(20.2194558703973,-0.420790919985035,
-4.05260893492845));
#38169=CARTESIAN_POINT('Ctrl Pts',(20.4158011659496,3.14930658013591,-2.58507332677998));
#38170=CARTESIAN_POINT('Ctrl Pts',(20.6121464615019,3.89287934840499,1.20259056256386));
#38171=CARTESIAN_POINT('Ctrl Pts',(20.8084917570543,1.14256321370995,3.91091752851028));
#38172=CARTESIAN_POINT('Ctrl Pts',(21.0048370526065,-2.63321155023091,3.10916840482789));
#38173=CARTESIAN_POINT('Ctrl Pts',(21.2011823481589,-4.04565952869842,-0.483083286308333));
#38174=CARTESIAN_POINT('Ctrl Pts',(21.3975276437112,-1.8270978637576,-3.64176373295804));
#38175=CARTESIAN_POINT('Ctrl Pts',(21.5938729392636,2.03129768810438,-3.53193432001087));
#38176=CARTESIAN_POINT('Ctrl Pts',(21.7902182348159,4.06658846653455,-0.252167453610417));
#38177=CARTESIAN_POINT('Ctrl Pts',(21.9865635303682,2.45208580652506,3.25392152588244));
#38178=CARTESIAN_POINT('Ctrl Pts',(22.1829088259205,-1.36318211460772,3.83959173733726));
#38179=CARTESIAN_POINT('Ctrl Pts',(22.3792541214729,-3.95498394205026,0.979199763547288));
#38180=CARTESIAN_POINT('Ctrl Pts',(22.5755994170252,-2.99715823388054,-2.76003128110674));
#38181=CARTESIAN_POINT('Ctrl Pts',(22.7719447125776,0.650639302909993,-4.02211370558222));
#38182=CARTESIAN_POINT('Ctrl Pts',(22.9682900081298,3.71448322162319,-1.67431913170009));
#38183=CARTESIAN_POINT('Ctrl Pts',(23.1646353036822,3.44455079341363,2.17618932762861));
#38184=CARTESIAN_POINT('Ctrl Pts',(23.3609805992344,0.0831083826680549,
4.07355166362955));
#38185=CARTESIAN_POINT('Ctrl Pts',(23.5573258947869,-3.35292442033917,2.31487105262785));
#38186=CARTESIAN_POINT('Ctrl Pts',(23.7536711903391,-3.77968259269412,-1.52142356278974));
#38187=CARTESIAN_POINT('Ctrl Pts',(23.9500164858915,-0.814147497382348,
-3.99222920326887));
#38188=CARTESIAN_POINT('Ctrl Pts',(24.1463617814438,2.88209103831078,-2.87997941063644));
#38189=CARTESIAN_POINT('Ctrl Pts',(24.3427070769961,3.99163140933442,0.817073345265716));
#38190=CARTESIAN_POINT('Ctrl Pts',(24.5390523725485,1.51865287151657,3.7807966903717));
#38191=CARTESIAN_POINT('Ctrl Pts',(24.7353976681007,-2.31732792477034,3.3512268570744));
#38192=CARTESIAN_POINT('Ctrl Pts',(24.9317429636531,-4.07348965640595,-0.0860940316010964));
#38193=CARTESIAN_POINT('Ctrl Pts',(25.1280882592054,-2.17366409142741,-3.44614488512086));
#38194=CARTESIAN_POINT('Ctrl Pts',(25.3244335547578,1.67704117556227,-3.71325504837403));
#38195=CARTESIAN_POINT('Ctrl Pts',(25.5207788503101,4.02258950835972,-0.647691156531652));
#38196=CARTESIAN_POINT('Ctrl Pts',(25.7171241458624,2.75783379480394,2.99918036459964));
#38197=CARTESIAN_POINT('Ctrl Pts',(25.9134694414148,-0.982098256300655,
3.95426519037146));
#38198=CARTESIAN_POINT('Ctrl Pts',(26.1098147369671,-3.84058986115548,1.36036754480492));
#38199=CARTESIAN_POINT('Ctrl Pts',(26.3061600325194,-3.25212337263064,-2.45447005677918));
#38200=CARTESIAN_POINT('Ctrl Pts',(26.5025053280717,0.255147863333422,-4.06640259338584));
#38201=CARTESIAN_POINT('Ctrl Pts',(26.6988506236241,3.53342236689032,-2.02870836125074));
#38202=CARTESIAN_POINT('Ctrl Pts',(26.8951959191764,3.64042325964169,1.82976640661915));
#38203=CARTESIAN_POINT('Ctrl Pts',(27.0915412147287,0.480118592869677,4.04601282983465));
#38204=CARTESIAN_POINT('Ctrl Pts',(27.2878865102811,-3.11109885008213,2.63093139126324));
#38205=CARTESIAN_POINT('Ctrl Pts',(27.4842318058334,-3.91007652983126,-1.14542817700039));
#38206=CARTESIAN_POINT('Ctrl Pts',(27.6805771013857,-1.19974189171588,-3.89376206591915));
#38207=CARTESIAN_POINT('Ctrl Pts',(27.876922396938,2.58739042917252,-3.14740648154211));
#38208=CARTESIAN_POINT('Ctrl Pts',(28.0732676924904,4.05228085305474,0.423752273999395));
#38209=CARTESIAN_POINT('Ctrl Pts',(28.2696129880427,1.88029638033132,3.61462443485592));
#38210=CARTESIAN_POINT('Ctrl Pts',(28.465958283595,-1.97941866999231,3.56127761652517));
#38211=CARTESIAN_POINT('Ctrl Pts',(28.6623035791473,-4.06229755588892,0.311787362974019));
#38212=CARTESIAN_POINT('Ctrl Pts',(28.8586488746997,-2.49980496581944,-3.21778697291297));
#38213=CARTESIAN_POINT('Ctrl Pts',(29.0549941702519,1.30739290614095,-3.85888170035648));
#38214=CARTESIAN_POINT('Ctrl Pts',(29.2513394658043,3.93902795927863,-1.03755933259342));
#38215=CARTESIAN_POINT('Ctrl Pts',(29.4476847613566,3.03961298802498,2.71684910424524));
#38216=CARTESIAN_POINT('Ctrl Pts',(29.644030056909,-0.596536360381995,4.02918820583754));
#38217=CARTESIAN_POINT('Ctrl Pts',(29.7749269206105,-2.64989673996124,2.49829364375959));
#38218=CARTESIAN_POINT('Ctrl Pts',(29.8403753524613,-3.13273600006486,1.46768709331983));
#38219=CARTESIAN_POINT('Ctrl Pts',(18.,1.87158653173903,-2.62360084935058));
#38220=CARTESIAN_POINT('Ctrl Pts',(18.0654484318508,2.73469795288145,-2.00788687304197));
#38221=CARTESIAN_POINT('Ctrl Pts',(18.1963452955523,3.79210558070424,0.130964326648123));
#38222=CARTESIAN_POINT('Ctrl Pts',(18.3926905911047,1.97820456802146,3.24194700629428));
#38223=CARTESIAN_POINT('Ctrl Pts',(18.589035886657,-1.6130627898401,3.43470578559991));
#38224=CARTESIAN_POINT('Ctrl Pts',(18.7853811822093,-3.75559777342547,0.549005246770418));
#38225=CARTESIAN_POINT('Ctrl Pts',(18.9817264777616,-2.5279689748886,-2.83157909096179));
#38226=CARTESIAN_POINT('Ctrl Pts',(19.178071773314,0.968794511424788,-3.66969878371352));
#38227=CARTESIAN_POINT('Ctrl Pts',(19.3744170688663,3.59592225045646,-1.21480199941451));
#38228=CARTESIAN_POINT('Ctrl Pts',(19.5707623644186,2.99575257360889,2.33067906227099));
#38229=CARTESIAN_POINT('Ctrl Pts',(19.7671076599709,-0.293163078231386,
3.78420913942485));
#38230=CARTESIAN_POINT('Ctrl Pts',(19.9634529555233,-3.31894432990856,1.84145995805286));
#38231=CARTESIAN_POINT('Ctrl Pts',(20.1597982510756,-3.36595776249388,-1.75405259865246));
#38232=CARTESIAN_POINT('Ctrl Pts',(20.3561435466279,-0.391994200717362,
-3.77526967626554));
#38233=CARTESIAN_POINT('Ctrl Pts',(20.5524888421802,2.93378458769563,-2.4081644931002));
#38234=CARTESIAN_POINT('Ctrl Pts',(20.7488341377326,3.62647114324965,1.12029158418925));
#38235=CARTESIAN_POINT('Ctrl Pts',(20.9451794332849,1.06437219164148,3.64327488510088));
#38236=CARTESIAN_POINT('Ctrl Pts',(21.1415247288372,-2.45300838950909,2.89639325817577));
#38237=CARTESIAN_POINT('Ctrl Pts',(21.3378700243895,-3.76879585087811,-0.450023604841809));
#38238=CARTESIAN_POINT('Ctrl Pts',(21.5342153199419,-1.70206088753426,-3.39254056088757));
#38239=CARTESIAN_POINT('Ctrl Pts',(21.7305606154942,1.89228634899218,-3.29022729579853));
#38240=CARTESIAN_POINT('Ctrl Pts',(21.9269059110465,3.78829252219229,-0.234910438249147));
#38241=CARTESIAN_POINT('Ctrl Pts',(22.1232512065989,2.28427793986952,3.03124023631671));
#38242=CARTESIAN_POINT('Ctrl Pts',(22.3195965021511,-1.26989309433504,3.57683025625195));
#38243=CARTESIAN_POINT('Ctrl Pts',(22.5159417977035,-3.68432562487137,0.912188477517553));
#38244=CARTESIAN_POINT('Ctrl Pts',(22.7122870932558,-2.792048474704,-2.57114924445347));
#38245=CARTESIAN_POINT('Ctrl Pts',(22.9086323888082,0.606112968189978,-3.74686138016046));
#38246=CARTESIAN_POINT('Ctrl Pts',(23.1049776843605,3.46028350989628,-1.55973752903206));
#38247=CARTESIAN_POINT('Ctrl Pts',(23.3013229799128,3.2088238385529,2.02726236612665));
#38248=CARTESIAN_POINT('Ctrl Pts',(23.4976682754651,0.0774208817006576,
3.79477919467037));
#38249=CARTESIAN_POINT('Ctrl Pts',(23.6940135710175,-3.1234678929464,2.15645344265251));
#38250=CARTESIAN_POINT('Ctrl Pts',(23.8903588665698,-3.52102097863996,-1.41730532937728));
#38251=CARTESIAN_POINT('Ctrl Pts',(24.0867041621221,-0.758431521083658,
-3.71902201613955));
#38252=CARTESIAN_POINT('Ctrl Pts',(24.2830494576745,2.68485587331004,-2.68288875433691));
#38253=CARTESIAN_POINT('Ctrl Pts',(24.4793947532267,3.71846513208049,0.761157139313524));
#38254=CARTESIAN_POINT('Ctrl Pts',(24.6757400487791,1.41472424965457,3.52205883332719));
#38255=CARTESIAN_POINT('Ctrl Pts',(24.8720853443314,-2.15874217937669,3.12188650199061));
#38256=CARTESIAN_POINT('Ctrl Pts',(25.0684306398838,-3.79472143089529,-0.0802022085106187));
#38257=CARTESIAN_POINT('Ctrl Pts',(25.2647759354361,-2.02490994382068,-3.2103088390008));
#38258=CARTESIAN_POINT('Ctrl Pts',(25.4611212309884,1.56227329051694,-3.45913938637011));
#38259=CARTESIAN_POINT('Ctrl Pts',(25.6574665265407,3.74730462149625,-0.603366577456954));
#38260=CARTESIAN_POINT('Ctrl Pts',(25.8538118220931,2.56910214256522,2.79393222142319));
#38261=CARTESIAN_POINT('Ctrl Pts',(26.0501571176454,-0.914888612658763,
3.68365606078035));
#38262=CARTESIAN_POINT('Ctrl Pts',(26.2465024131977,-3.5777600737213,1.26727113889869));
#38263=CARTESIAN_POINT('Ctrl Pts',(26.44284770875,-3.02956513922398,-2.28649902456573));
#38264=CARTESIAN_POINT('Ctrl Pts',(26.6391930043024,0.237686884393074,-3.7881193692251));
#38265=CARTESIAN_POINT('Ctrl Pts',(26.8355382998547,3.29161350856939,-1.88987422206122));
#38266=CARTESIAN_POINT('Ctrl Pts',(27.0318835954071,3.39129182252066,1.70454680934583));
#38267=CARTESIAN_POINT('Ctrl Pts',(27.2282288909593,0.447261799442319,3.76912497394121));
#38268=CARTESIAN_POINT('Ctrl Pts',(27.4245741865117,-2.89819159390149,2.45088427263869));
#38269=CARTESIAN_POINT('Ctrl Pts',(27.620919482064,-3.64249143995193,-1.0670410919));
#38270=CARTESIAN_POINT('Ctrl Pts',(27.8172647776164,-1.11763786140405,-3.62729345221592));
#38271=CARTESIAN_POINT('Ctrl Pts',(28.0136100731686,2.41032302518161,-2.93201452186437));
#38272=CARTESIAN_POINT('Ctrl Pts',(28.2099553687211,3.77496404659118,0.394752895225204));
#38273=CARTESIAN_POINT('Ctrl Pts',(28.4063006642733,1.75161877719691,3.36725853372798));
#38274=CARTESIAN_POINT('Ctrl Pts',(28.6026459598257,-1.84395765825054,3.31756249130118));
#38275=CARTESIAN_POINT('Ctrl Pts',(28.798991255378,-3.78429525892211,0.290450274324173));
#38276=CARTESIAN_POINT('Ctrl Pts',(28.9953365509303,-2.32873145067049,-2.99757854226198));
#38277=CARTESIAN_POINT('Ctrl Pts',(29.1916818464826,1.21792180611816,-3.59480011557272));
#38278=CARTESIAN_POINT('Ctrl Pts',(29.388027142035,3.66946158571043,-0.966554224343232));
#38279=CARTESIAN_POINT('Ctrl Pts',(29.5843724375873,2.83159784857854,2.53092222884994));
#38280=CARTESIAN_POINT('Ctrl Pts',(29.7807177331396,-0.555712546732512,
3.75345173879546));
#38281=CARTESIAN_POINT('Ctrl Pts',(29.9116145968412,-2.46855173253653,2.32732355555027));
#38282=CARTESIAN_POINT('Ctrl Pts',(29.9770630286919,-2.91834801104467,1.36724630148763));
#38283=CARTESIAN_POINT('Ctrl Pts',(18.,1.75280451302835,3.52727163111204));
#38284=CARTESIAN_POINT('Ctrl Pts',(18.,1.85055634181796,3.46829220042325));
#38285=CARTESIAN_POINT('Ctrl Pts',(18.,1.9453897415748,3.40491824723834));
#38286=CARTESIAN_POINT('Ctrl Pts',(18.,2.03695736150634,3.33713960726484));
#38287=CARTESIAN_POINT('Ctrl Pts',(18.,2.13485777676419,3.26467341229354));
#38288=CARTESIAN_POINT('Ctrl Pts',(18.,2.22902577851624,3.18717173263842));
#38289=CARTESIAN_POINT('Ctrl Pts',(18.,2.31927390895822,3.10504417467128));
#38290=CARTESIAN_POINT('Ctrl Pts',(18.,2.37057338638084,3.05836065020293));
#38291=CARTESIAN_POINT('Ctrl Pts',(18.,2.42060555689673,3.01018185463388));
#38292=CARTESIAN_POINT('Ctrl Pts',(18.,2.46932956368599,2.96057932112694));
#38293=CARTESIAN_POINT('Ctrl Pts',(18.,2.48926772386374,2.94028166246842));
#38294=CARTESIAN_POINT('Ctrl Pts',(18.,2.50898677586689,2.91974557487581));
#38295=CARTESIAN_POINT('Ctrl Pts',(18.,2.52848367972817,2.89897587060429));
#38296=CARTESIAN_POINT('Ctrl Pts',(18.,2.54217196878492,2.88439398018136));
#38297=CARTESIAN_POINT('Ctrl Pts',(18.,2.55574734184337,2.86970051594287));
#38298=CARTESIAN_POINT('Ctrl Pts',(18.,2.56920386940907,2.85490297454373));
#38299=CARTESIAN_POINT('Ctrl Pts',(18.,2.65294903624156,2.76281216083778));
#38300=CARTESIAN_POINT('Ctrl Pts',(18.,2.73215730305588,2.66662713037754));
#38301=CARTESIAN_POINT('Ctrl Pts',(18.,2.80663529425947,2.56679160942941));
#38302=CARTESIAN_POINT('Ctrl Pts',(18.,2.87180353656261,2.4794355285998));
#38303=CARTESIAN_POINT('Ctrl Pts',(18.,2.9333495992658,2.38928354160773));
#38304=CARTESIAN_POINT('Ctrl Pts',(18.,2.99111044370871,2.29661846198891));
#38305=CARTESIAN_POINT('Ctrl Pts',(18.,3.01638081315248,2.25607748965567));
#38306=CARTESIAN_POINT('Ctrl Pts',(18.,3.04092624626456,2.21505537388696));
#38307=CARTESIAN_POINT('Ctrl Pts',(18.,3.06473105776385,2.17357540269015));
#38308=CARTESIAN_POINT('Ctrl Pts',(18.,3.07937622571154,2.14805614391925));
#38309=CARTESIAN_POINT('Ctrl Pts',(18.,3.09374104789547,2.12236358627869));
#38310=CARTESIAN_POINT('Ctrl Pts',(18.,3.10782162822979,2.09650313728402));
#38311=CARTESIAN_POINT('Ctrl Pts',(18.,3.11588415285192,2.08169547298267));
#38312=CARTESIAN_POINT('Ctrl Pts',(18.,3.12385167846963,2.06683599660815));
#38313=CARTESIAN_POINT('Ctrl Pts',(18.,3.1317198130323,2.05193313593188));
#38314=CARTESIAN_POINT('Ctrl Pts',(18.,3.18720095944412,1.94684751639281));
#38315=CARTESIAN_POINT('Ctrl Pts',(18.,3.23780322769338,1.83949826444516));
#38316=CARTESIAN_POINT('Ctrl Pts',(18.,3.28335897157006,1.73026580000651));
#38317=CARTESIAN_POINT('Ctrl Pts',(18.,3.32860687522003,1.62177146744223));
#38318=CARTESIAN_POINT('Ctrl Pts',(18.,3.36887645015951,1.51141841716963));
#38319=CARTESIAN_POINT('Ctrl Pts',(18.,3.40395374640598,1.3995675723142));
#38320=CARTESIAN_POINT('Ctrl Pts',(18.,3.43799986603056,1.29100483654054));
#38321=CARTESIAN_POINT('Ctrl Pts',(18.,3.46715450249439,1.18103033348445));
#38322=CARTESIAN_POINT('Ctrl Pts',(18.,3.49117371118248,1.06997467581908));
#38323=CARTESIAN_POINT('Ctrl Pts',(18.,3.50794056569238,0.992451137106512));
#38324=CARTESIAN_POINT('Ctrl Pts',(18.,3.52220399937057,0.914400770171061));
#38325=CARTESIAN_POINT('Ctrl Pts',(18.,3.53386633916247,0.835939010635201));
#38326=CARTESIAN_POINT('Ctrl Pts',(18.,3.53850288921364,0.804745280930666));
#38327=CARTESIAN_POINT('Ctrl Pts',(18.,3.54272817554279,0.773486566216751));
#38328=CARTESIAN_POINT('Ctrl Pts',(18.,3.54653550521384,0.74217030018733));
#38329=CARTESIAN_POINT('Ctrl Pts',(18.,3.548303818075,0.727625471982788));
#38330=CARTESIAN_POINT('Ctrl Pts',(18.,3.54998159728476,0.713070984488063));
#38331=CARTESIAN_POINT('Ctrl Pts',(18.,3.55156744344722,0.698515996963189));
#38332=CARTESIAN_POINT('Ctrl Pts',(18.,3.56369208352232,0.587235351201648));
#38333=CARTESIAN_POINT('Ctrl Pts',(18.,3.57046471402958,0.47578171671144));
#38334=CARTESIAN_POINT('Ctrl Pts',(18.,3.57169639188583,0.364475115519244));
#38335=CARTESIAN_POINT('Ctrl Pts',(18.,3.57257411457641,0.285155406244404));
#38336=CARTESIAN_POINT('Ctrl Pts',(18.,3.57063694555984,0.205910265097998));
#38337=CARTESIAN_POINT('Ctrl Pts',(18.,3.56580039408165,0.126857466521517));
#38338=CARTESIAN_POINT('Ctrl Pts',(18.,3.55887863429577,0.0137222120711326));
#38339=CARTESIAN_POINT('Ctrl Pts',(18.,3.54602018773888,-0.0990203100151426));
#38340=CARTESIAN_POINT('Ctrl Pts',(18.,3.52743695201649,-0.211010483416101));
#38341=CARTESIAN_POINT('Ctrl Pts',(18.,3.508804805596,-0.323295412673502));
#38342=CARTESIAN_POINT('Ctrl Pts',(18.,3.4844171411277,-0.434824818175472));
#38343=CARTESIAN_POINT('Ctrl Pts',(18.,3.45444382525478,-0.545208161076649));
#38344=CARTESIAN_POINT('Ctrl Pts',(18.,3.44863818325821,-0.56658871750177));
#38345=CARTESIAN_POINT('Ctrl Pts',(18.,3.44262286633546,-0.587926171790228));
#38346=CARTESIAN_POINT('Ctrl Pts',(18.,3.43639894723186,-0.609217525642749));
#38347=CARTESIAN_POINT('Ctrl Pts',(18.,3.4319855878944,-0.624315150429954));
#38348=CARTESIAN_POINT('Ctrl Pts',(18.,3.42746744875845,-0.639389001662136));
#38349=CARTESIAN_POINT('Ctrl Pts',(18.,3.42284901423685,-0.654425291755363));
#38350=CARTESIAN_POINT('Ctrl Pts',(18.,3.39017323849704,-0.760808188545976));
#38351=CARTESIAN_POINT('Ctrl Pts',(18.,3.35243274001992,-0.865480322917389));
#38352=CARTESIAN_POINT('Ctrl Pts',(18.,3.30986573133022,-0.968117196308756));
#38353=CARTESIAN_POINT('Ctrl Pts',(18.,3.26724317972447,-1.07088799386855));
#38354=CARTESIAN_POINT('Ctrl Pts',(18.,3.21978092670367,-1.17161896447357));
#38355=CARTESIAN_POINT('Ctrl Pts',(18.,3.16767339295151,-1.26995725336641));
#38356=CARTESIAN_POINT('Ctrl Pts',(18.,3.11619046641229,-1.36711677212509));
#38357=CARTESIAN_POINT('Ctrl Pts',(18.,3.06017233448318,-1.46194124984198));
#38358=CARTESIAN_POINT('Ctrl Pts',(18.,2.99977200511078,-1.55405385994265));
#38359=CARTESIAN_POINT('Ctrl Pts',(18.,2.96384880635417,-1.60883799166874));
#38360=CARTESIAN_POINT('Ctrl Pts',(18.,2.9263748812984,-1.6626621140883));
#38361=CARTESIAN_POINT('Ctrl Pts',(18.,2.88737785842231,-1.71543935342494));
#38362=CARTESIAN_POINT('Ctrl Pts',(18.,2.869045125242,-1.74025024860087));
#38363=CARTESIAN_POINT('Ctrl Pts',(18.,2.85037574463248,-1.7648296948276));
#38364=CARTESIAN_POINT('Ctrl Pts',(18.,2.83137237441651,-1.78916817371834));
#38365=CARTESIAN_POINT('Ctrl Pts',(18.,2.82197518346086,-1.80120358275932));
#38366=CARTESIAN_POINT('Ctrl Pts',(18.,2.81249924524833,-1.813176259781));
#38367=CARTESIAN_POINT('Ctrl Pts',(18.,2.80294996247512,-1.82507914472327));
#38368=CARTESIAN_POINT('Ctrl Pts',(18.,2.73565253998902,-1.90896329558436));
#38369=CARTESIAN_POINT('Ctrl Pts',(18.,2.66464231294219,-1.98947789681978));
#38370=CARTESIAN_POINT('Ctrl Pts',(18.,2.59009745348758,-2.06630396380742));
#38371=CARTESIAN_POINT('Ctrl Pts',(18.,2.51658282385074,-2.14206827408143));
#38372=CARTESIAN_POINT('Ctrl Pts',(18.,2.43962999231716,-2.21424581024087));
#38373=CARTESIAN_POINT('Ctrl Pts',(18.,2.35938133050909,-2.28248986040027));
#38374=CARTESIAN_POINT('Ctrl Pts',(18.,2.28159477252663,-2.34864011942115));
#38375=CARTESIAN_POINT('Ctrl Pts',(18.,2.20071097356059,-2.41109484295671));
#38376=CARTESIAN_POINT('Ctrl Pts',(18.,2.11684099713627,-2.46949410191337));
#38377=CARTESIAN_POINT('Ctrl Pts',(18.,2.03771972777132,-2.5245868024913));
#38378=CARTESIAN_POINT('Ctrl Pts',(18.,1.95594042011274,-2.57607026124645));
#38379=CARTESIAN_POINT('Ctrl Pts',(18.,1.87158653173906,-2.62360084935056));
#38380=CARTESIAN_POINT('Origin',(23.75,0.,0.));
#38381=CARTESIAN_POINT('Origin',(29.567,0.,0.));
#38382=CARTESIAN_POINT('Origin',(17.,0.,0.));
#38383=CARTESIAN_POINT('',(18.,-8.,-9.79717439317883E-16));
#38384=CARTESIAN_POINT('Origin',(18.,0.,0.));
#38385=CARTESIAN_POINT('',(17.,-9.,-1.10218211923262E-15));
#38386=CARTESIAN_POINT('Origin',(18.,4.,0.));
#38387=CARTESIAN_POINT('Origin',(29.75,0.,0.));
#38388=CARTESIAN_POINT('',(30.,-3.5,-4.28626379701574E-16));
#38389=CARTESIAN_POINT('Origin',(30.,0.,0.));
#38390=CARTESIAN_POINT('',(29.75,-3.75,-4.59242549680257E-16));
#38391=CARTESIAN_POINT('Origin',(30.,0.,0.));
#38392=CARTESIAN_POINT('',(0.,0.,0.));
#38393=CARTESIAN_POINT('Origin',(-27.25,0.,0.));
#38394=CARTESIAN_POINT('',(-54.162836477965,-3.93774042332204,0.0025401470004769));
#38395=CARTESIAN_POINT('',(-54.3461635220349,-3.93688521119116,0.00404501750981942));
#38396=CARTESIAN_POINT('',(-27.25,-3.933,-4.81653586104654E-16));
#38397=CARTESIAN_POINT('',(-54.567,1.75074534075625,3.52552341725016));
#38398=CARTESIAN_POINT('Ctrl Pts',(-54.162836477965,-3.93774042332204,0.0025401470004769));
#38399=CARTESIAN_POINT('Ctrl Pts',(-54.1696144592364,-3.93866195343843,
0.136067499180593));
#38400=CARTESIAN_POINT('Ctrl Pts',(-54.1763924405079,-3.93246070603142,
0.26950274978779));
#38401=CARTESIAN_POINT('Ctrl Pts',(-54.1831704217794,-3.91885498293026,
0.402171763676285));
#38402=CARTESIAN_POINT('Ctrl Pts',(-54.2493281390221,-3.78605385147857,
1.69711176958284));
#38403=CARTESIAN_POINT('Ctrl Pts',(-54.3154858562649,-2.94782161396214,
2.91905170927145));
#38404=CARTESIAN_POINT('Ctrl Pts',(-54.3816435735076,-1.78754908268422,
3.51017407453822));
#38405=CARTESIAN_POINT('Ctrl Pts',(-54.4434290490051,-0.70395682709477,
4.06223025086027));
#38406=CARTESIAN_POINT('Ctrl Pts',(-54.5052145245025,0.660516179498767,
4.06409281016428));
#38407=CARTESIAN_POINT('Ctrl Pts',(-54.567,1.75279620618131,3.52818484004948));
#38408=CARTESIAN_POINT('',(-54.567,-1.74869447533071,3.52286199445108));
#38409=CARTESIAN_POINT('Origin',(-54.567,0.,0.));
#38410=CARTESIAN_POINT('Ctrl Pts',(-54.567,-1.74869447533071,3.52286199445108));
#38411=CARTESIAN_POINT('Ctrl Pts',(-54.5008422827573,-2.92020446772555,
2.9413424643865));
#38412=CARTESIAN_POINT('Ctrl Pts',(-54.4346845655146,-3.76871594031363,
1.73455576822158));
#38413=CARTESIAN_POINT('Ctrl Pts',(-54.3685268482719,-3.91414328439161,
0.442962886141297));
#38414=CARTESIAN_POINT('Ctrl Pts',(-54.3610724061929,-3.93052957700137,
0.297430290241746));
#38415=CARTESIAN_POINT('Ctrl Pts',(-54.3536179641139,-3.93798946516557,
0.150820989173826));
#38416=CARTESIAN_POINT('Ctrl Pts',(-54.3461635220349,-3.93688521119116,
0.00404501750981942));
#38417=CARTESIAN_POINT('Origin',(-27.25,0.,0.));
#38418=CARTESIAN_POINT('',(-52.912836477965,-3.92758587675543,0.00202738283172854));
#38419=CARTESIAN_POINT('',(-53.0961635220349,-3.92737769983192,0.00186527213366315));
#38420=CARTESIAN_POINT('',(-27.25,-3.933,-4.81653586104654E-16));
#38421=CARTESIAN_POINT('Ctrl Pts',(-52.912836477965,-3.92758587675543,0.00202738283172854));
#38422=CARTESIAN_POINT('Ctrl Pts',(-52.9393348224469,-3.93003459305733,
0.527558129595977));
#38423=CARTESIAN_POINT('Ctrl Pts',(-52.9658331669288,-3.83198391398178,
1.05221170696794));
#38424=CARTESIAN_POINT('Ctrl Pts',(-52.9923315114107,-3.62911428541967,
1.53259749559324));
#38425=CARTESIAN_POINT('Ctrl Pts',(-53.0584892286534,-3.122615038543,2.73196401424622));
#38426=CARTESIAN_POINT('Ctrl Pts',(-53.1246469458961,-1.96273954373826,
3.65539262418095));
#38427=CARTESIAN_POINT('Ctrl Pts',(-53.1908046631387,-0.680367641251685,
3.88025158114632));
#38428=CARTESIAN_POINT('Ctrl Pts',(-53.2569623803814,0.602004261234901,
4.10511053811169));
#38429=CARTESIAN_POINT('Ctrl Pts',(-53.3231200976241,2.00687257140333,3.63139984210768));
#38430=CARTESIAN_POINT('Ctrl Pts',(-53.3892778148669,2.891205608505,2.67588403906754));
#38431=CARTESIAN_POINT('Ctrl Pts',(-53.4554355321096,3.77553864560666,1.7203682360274));
#38432=CARTESIAN_POINT('Ctrl Pts',(-53.5215932493523,4.13933640964158,0.283047325951132));
#38433=CARTESIAN_POINT('Ctrl Pts',(-53.587750966595,3.81610600351479,-0.978094706542245));
#38434=CARTESIAN_POINT('Ctrl Pts',(-53.6539086838378,3.492875597388,-2.23923673903563));
#38435=CARTESIAN_POINT('Ctrl Pts',(-53.7200664010804,2.48261702109949,-3.32419989394611));
#38436=CARTESIAN_POINT('Ctrl Pts',(-53.7862241183231,1.24769529796077,-3.73659569433847));
#38437=CARTESIAN_POINT('Ctrl Pts',(-53.8523818355659,0.0127735748220346,
-4.14899149473083));
#38438=CARTESIAN_POINT('Ctrl Pts',(-53.9185395528086,-1.44681129516692,
-3.88881994060506));
#38439=CARTESIAN_POINT('Ctrl Pts',(-53.9846972700513,-2.46291871746792,
-3.07476412747992));
#38440=CARTESIAN_POINT('Ctrl Pts',(-54.0440770060226,-3.37492404306438,
-2.34410984761879));
#38441=CARTESIAN_POINT('Ctrl Pts',(-54.1034567419937,-3.92966719136564,
-1.16725047351599));
#38442=CARTESIAN_POINT('Ctrl Pts',(-54.162836477965,-3.93774042332204,0.0025401470004769));
#38443=CARTESIAN_POINT('Ctrl Pts',(-54.3461635220349,-3.93688521119116,
0.00404501750981942));
#38444=CARTESIAN_POINT('Ctrl Pts',(-54.2874602468712,-3.92818927872256,
-1.15180677672198));
#38445=CARTESIAN_POINT('Ctrl Pts',(-54.2287569717075,-3.38839097382246,
-2.31799459148723));
#38446=CARTESIAN_POINT('Ctrl Pts',(-54.1700536965438,-2.49440531842674,
-3.0500924315163));
#38447=CARTESIAN_POINT('Ctrl Pts',(-54.1038959793011,-1.48689679281598,
-3.87515579909798));
#38448=CARTESIAN_POINT('Ctrl Pts',(-54.0377382620583,-0.0295365260265515,
-4.1488834662657));
#38449=CARTESIAN_POINT('Ctrl Pts',(-53.9715805448156,1.20964880738629,-3.74878655245096));
#38450=CARTESIAN_POINT('Ctrl Pts',(-53.9054228275729,2.44883414079913,-3.34868963863622));
#38451=CARTESIAN_POINT('Ctrl Pts',(-53.8392651103302,3.46984454083539,-2.27476814383901));
#38452=CARTESIAN_POINT('Ctrl Pts',(-53.7731073930875,3.80585975657112,-1.01715165494543));
#38453=CARTESIAN_POINT('Ctrl Pts',(-53.7069496758448,4.14187497230684,0.240464833948156));
#38454=CARTESIAN_POINT('Ctrl Pts',(-53.640791958602,3.79289500374203,1.68177631693811));
#38455=CARTESIAN_POINT('Ctrl Pts',(-53.5746342413593,2.91838761167926,2.64634772696721));
#38456=CARTESIAN_POINT('Ctrl Pts',(-53.5084765241166,2.04388021961649,3.61091913699631));
#38457=CARTESIAN_POINT('Ctrl Pts',(-53.442318806874,0.643845404055756,4.09875047406455));
#38458=CARTESIAN_POINT('Ctrl Pts',(-53.3761610896313,-0.640770562895464,
3.88694001100651));
#38459=CARTESIAN_POINT('Ctrl Pts',(-53.3100033723886,-1.92538652984669,
3.67512954794847));
#38460=CARTESIAN_POINT('Ctrl Pts',(-53.2438456551458,-3.0945836481884,2.76367728476414));
#38461=CARTESIAN_POINT('Ctrl Pts',(-53.1776879379031,-3.61328184600827,
1.56956290603595));
#38462=CARTESIAN_POINT('Ctrl Pts',(-53.1505131326137,-3.82634123072092,
1.0790709863075));
#38463=CARTESIAN_POINT('Ctrl Pts',(-53.1233383273243,-3.92964710016084,
0.540887733301384));
#38464=CARTESIAN_POINT('Ctrl Pts',(-53.0961635220349,-3.92737769983192,
0.00186527213366315));
#38465=CARTESIAN_POINT('Origin',(-27.25,0.,0.));
#38466=CARTESIAN_POINT('',(-51.662836477965,-3.93040782112997,-0.00335227714350295));
#38467=CARTESIAN_POINT('',(-51.8461635220349,-3.93077288487519,-0.00342755369346778));
#38468=CARTESIAN_POINT('',(-27.25,-3.933,-4.81653586104654E-16));
#38469=CARTESIAN_POINT('Ctrl Pts',(-51.662836477965,-3.93040782112997,-0.00335227714350295));
#38470=CARTESIAN_POINT('Ctrl Pts',(-51.7090551856573,-3.92298924677534,
0.911627821618423));
#38471=CARTESIAN_POINT('Ctrl Pts',(-51.7552738933496,-3.6045908394272,1.83126267808616));
#38472=CARTESIAN_POINT('Ctrl Pts',(-51.8014926010419,-3.02075944544342,
2.52870136511396));
#38473=CARTESIAN_POINT('Ctrl Pts',(-51.8676503182846,-2.185059915769,3.52701901081092));
#38474=CARTESIAN_POINT('Ctrl Pts',(-51.9338080355273,-0.805508898715437,
4.07007403534115));
#38475=CARTESIAN_POINT('Ctrl Pts',(-51.99996575277,0.486460775265182,3.90930586499069));
#38476=CARTESIAN_POINT('Ctrl Pts',(-52.0661234700127,1.7784304492458,3.74853769464024));
#38477=CARTESIAN_POINT('Ctrl Pts',(-52.1322811872554,2.98281878015347,2.88394632940911));
#38478=CARTESIAN_POINT('Ctrl Pts',(-52.1984389044981,3.54836614375573,1.71126187008268));
#38479=CARTESIAN_POINT('Ctrl Pts',(-52.2645966217408,4.113913507358,0.538577410756249));
#38480=CARTESIAN_POINT('Ctrl Pts',(-52.3307543389835,4.04061990365484,-0.942200142665483));
#38481=CARTESIAN_POINT('Ctrl Pts',(-52.3969120562262,3.36203289749339,-2.05330331430663));
#38482=CARTESIAN_POINT('Ctrl Pts',(-52.463069773469,2.68344589133195,-3.16440648594777));
#38483=CARTESIAN_POINT('Ctrl Pts',(-52.5292274907117,1.39956548271222,-3.90583527580832));
#38484=CARTESIAN_POINT('Ctrl Pts',(-52.5953852079544,0.098034511021366,
-3.93823530609415));
#38485=CARTESIAN_POINT('Ctrl Pts',(-52.6615429251971,-1.2034964606695,-3.97063533637998));
#38486=CARTESIAN_POINT('Ctrl Pts',(-52.7277006424398,-2.5226779954315,-3.29400660709107));
#38487=CARTESIAN_POINT('Ctrl Pts',(-52.7938583596825,-3.25570726333821,
-2.218040028761));
#38488=CARTESIAN_POINT('Ctrl Pts',(-52.8335177324433,-3.69513416910437,
-1.57303349911237));
#38489=CARTESIAN_POINT('Ctrl Pts',(-52.8731771052042,-3.92392094770037,
-0.784520614438989));
#38490=CARTESIAN_POINT('Ctrl Pts',(-52.912836477965,-3.92758587675543,0.00202738283172854));
#38491=CARTESIAN_POINT('Ctrl Pts',(-53.0961635220349,-3.92737769983192,
0.00186527213366315));
#38492=CARTESIAN_POINT('Ctrl Pts',(-53.0571806100816,-3.92412219046333,
-0.771375416098045));
#38493=CARTESIAN_POINT('Ctrl Pts',(-53.0181976981283,-3.70360763326856,
-1.54634307662655));
#38494=CARTESIAN_POINT('Ctrl Pts',(-52.979214786175,-3.27816841217882,-2.18472795751501));
#38495=CARTESIAN_POINT('Ctrl Pts',(-52.9130570689323,-2.55615750323147,
-3.26812794806574));
#38496=CARTESIAN_POINT('Ctrl Pts',(-52.8468993516896,-1.24393640803873,
-3.95815143489514));
#38497=CARTESIAN_POINT('Ctrl Pts',(-52.7807416344468,0.0578597559599706,
-3.93902318709568));
#38498=CARTESIAN_POINT('Ctrl Pts',(-52.7145839172041,1.35965591995867,-3.91989493929621));
#38499=CARTESIAN_POINT('Ctrl Pts',(-52.6484261999614,2.65102715276333,-3.19161495686788));
#38500=CARTESIAN_POINT('Ctrl Pts',(-52.5822684827187,3.34091148436537,-2.08749493259359));
#38501=CARTESIAN_POINT('Ctrl Pts',(-52.516110765476,4.03079581596742,-0.983374908319293));
#38502=CARTESIAN_POINT('Ctrl Pts',(-52.4499530482333,4.11919324636686,0.496585157800968));
#38503=CARTESIAN_POINT('Ctrl Pts',(-52.3837953309906,3.5656380921564,1.67497922474918));
#38504=CARTESIAN_POINT('Ctrl Pts',(-52.3176376137479,3.01208293794595,2.8533732916974));
#38505=CARTESIAN_POINT('Ctrl Pts',(-52.2514798965051,1.81657519912561,3.73020135947356));
#38506=CARTESIAN_POINT('Ctrl Pts',(-52.1853221792624,0.526312366823295,
3.90413913807549));
#38507=CARTESIAN_POINT('Ctrl Pts',(-52.1191644620197,-0.763950465479025,
4.07807691667742));
#38508=CARTESIAN_POINT('Ctrl Pts',(-52.0530067447771,-2.14896839126332,
3.54912440610509));
#38509=CARTESIAN_POINT('Ctrl Pts',(-51.9868490275344,-2.99480768303467,
2.55938384971904));
#38510=CARTESIAN_POINT('Ctrl Pts',(-51.9399538590345,-3.59437153989906,
1.85781716789794));
#38511=CARTESIAN_POINT('Ctrl Pts',(-51.8930586905347,-3.92302364013206,
0.924726291586686));
#38512=CARTESIAN_POINT('Ctrl Pts',(-51.8461635220349,-3.93077288487519,
-0.00342755369346778));
#38513=CARTESIAN_POINT('Origin',(-27.25,0.,0.));
#38514=CARTESIAN_POINT('',(-50.412836477965,-3.9394544622989,-8.04257353526072E-5));
#38515=CARTESIAN_POINT('',(-50.5961635220349,-3.93944735561455,0.000168331762536079));
#38516=CARTESIAN_POINT('',(-27.25,-3.933,-4.81653586104654E-16));
#38517=CARTESIAN_POINT('Ctrl Pts',(-50.412836477965,-3.9394544622989,-8.04257353526072E-5));
#38518=CARTESIAN_POINT('Ctrl Pts',(-50.4787755488677,-3.93906386773341,
1.29755258648731));
#38519=CARTESIAN_POINT('Ctrl Pts',(-50.5447146197704,-3.23516481471532,
2.59554871145119));
#38520=CARTESIAN_POINT('Ctrl Pts',(-50.6106536906731,-2.14723319787632,
3.30283324761193));
#38521=CARTESIAN_POINT('Ctrl Pts',(-50.6768114079158,-1.05569412550357,
4.01246305756969));
#38522=CARTESIAN_POINT('Ctrl Pts',(-50.7429691251586,0.422428548377894,
4.12745732105086));
#38523=CARTESIAN_POINT('Ctrl Pts',(-50.8091268424013,1.61058474395983,3.59518213874312));
#38524=CARTESIAN_POINT('Ctrl Pts',(-50.875284559644,2.79874093954177,3.06290695643538));
#38525=CARTESIAN_POINT('Ctrl Pts',(-50.9414422768866,3.69693065682417,1.88336232833872));
#38526=CARTESIAN_POINT('Ctrl Pts',(-51.0075999941293,3.89404435502893,0.596436447717042));
#38527=CARTESIAN_POINT('Ctrl Pts',(-51.073757711372,4.09115805323369,-0.690489432904646));
#38528=CARTESIAN_POINT('Ctrl Pts',(-51.1399154286147,3.58719573236078,-2.08479656605136));
#38529=CARTESIAN_POINT('Ctrl Pts',(-51.2060731458575,2.61282550158419,-2.94829795308546));
#38530=CARTESIAN_POINT('Ctrl Pts',(-51.2722308631002,1.63845527080759,-3.81179934011955));
#38531=CARTESIAN_POINT('Ctrl Pts',(-51.3383885803429,0.193677130127309,
-4.14449498104103));
#38532=CARTESIAN_POINT('Ctrl Pts',(-51.4045462975856,-1.0602209484054,-3.79410716689309));
#38533=CARTESIAN_POINT('Ctrl Pts',(-51.4707040148283,-2.3141190269381,-3.44371935274515));
#38534=CARTESIAN_POINT('Ctrl Pts',(-51.536861732071,-3.37713704332323,-2.41024808352779));
#38535=CARTESIAN_POINT('Ctrl Pts',(-51.6030194493137,-3.76272203036817,
-1.16672231548726));
#38536=CARTESIAN_POINT('Ctrl Pts',(-51.6229584588641,-3.87893194600034,
-0.791941062467227));
#38537=CARTESIAN_POINT('Ctrl Pts',(-51.6428974684146,-3.93360823568704,
-0.398079820136163));
#38538=CARTESIAN_POINT('Ctrl Pts',(-51.662836477965,-3.93040782112997,-0.00335227714350295));
#38539=CARTESIAN_POINT('Ctrl Pts',(-51.8461635220349,-3.93077288487519,
-0.00342755369346778));
#38540=CARTESIAN_POINT('Ctrl Pts',(-51.826900973292,-3.93395594635807,-0.384673836787234));
#38541=CARTESIAN_POINT('Ctrl Pts',(-51.8076384245491,-3.88299568796656,
-0.765087134926914));
#38542=CARTESIAN_POINT('Ctrl Pts',(-51.7883758758062,-3.77442753736563,
-1.1282797903303));
#38543=CARTESIAN_POINT('Ctrl Pts',(-51.7222181585635,-3.40154744216686,
-2.37567427179388));
#38544=CARTESIAN_POINT('Ctrl Pts',(-51.6560604413208,-2.34912659401091,
-3.41993463252129));
#38545=CARTESIAN_POINT('Ctrl Pts',(-51.5899027240781,-1.09886791146382,
-3.78309460396163));
#38546=CARTESIAN_POINT('Ctrl Pts',(-51.5237450068354,0.151390771083265,
-4.14625457540197));
#38547=CARTESIAN_POINT('Ctrl Pts',(-51.4575872895927,1.59948728802148,-3.82831415755525));
#38548=CARTESIAN_POINT('Ctrl Pts',(-51.3914295723499,2.58261501047815,-2.97479696275541));
#38549=CARTESIAN_POINT('Ctrl Pts',(-51.3252718551072,3.56574273293481,-2.12127976795557));
#38550=CARTESIAN_POINT('Ctrl Pts',(-51.2591141378645,4.08390166090993,-0.732185796202606));
#38551=CARTESIAN_POINT('Ctrl Pts',(-51.1929564206218,3.8999256686853,0.556683804504271));
#38552=CARTESIAN_POINT('Ctrl Pts',(-51.1267987033791,3.71594967646068,1.84555340521114));
#38553=CARTESIAN_POINT('Ctrl Pts',(-51.0606409861364,2.82983876403635,3.03419863487192));
#38554=CARTESIAN_POINT('Ctrl Pts',(-50.9944832688937,1.64717394726657,3.5785660089322));
#38555=CARTESIAN_POINT('Ctrl Pts',(-50.928325551651,0.464509130496774,4.12293338299248));
#38556=CARTESIAN_POINT('Ctrl Pts',(-50.8621678344082,-1.01470959061848,
4.02302290145225));
#38557=CARTESIAN_POINT('Ctrl Pts',(-50.7960101171655,-2.11343049329063,
3.32456440936727));
#38558=CARTESIAN_POINT('Ctrl Pts',(-50.7298523999228,-3.21215139596279,
2.6261059172823));
#38559=CARTESIAN_POINT('Ctrl Pts',(-50.6636946826802,-3.93037448019184,
1.32909941465258));
#38560=CARTESIAN_POINT('Ctrl Pts',(-50.5975369654374,-3.9393625454203,0.0271965219255519));
#38561=CARTESIAN_POINT('Ctrl Pts',(-50.5970791509699,-3.93942474324798,
0.0181872936082175));
#38562=CARTESIAN_POINT('Ctrl Pts',(-50.5966213365024,-3.93945297790921,
0.00917783081723566));
#38563=CARTESIAN_POINT('Ctrl Pts',(-50.5961635220349,-3.93944735561455,
0.000168331762536079));
#38564=CARTESIAN_POINT('Origin',(-27.25,0.,0.));
#38565=CARTESIAN_POINT('',(-49.1628364779651,-3.93064273659572,0.00340251455877419));
#38566=CARTESIAN_POINT('',(-49.3461635220349,-3.93028113905034,0.00332252600905021));
#38567=CARTESIAN_POINT('',(-27.25,-3.933,-4.81653586104654E-16));
#38568=CARTESIAN_POINT('Ctrl Pts',(-49.1628364779651,-3.93064273659572,
0.00340251455877419));
#38569=CARTESIAN_POINT('Ctrl Pts',(-49.1823381948354,-3.93383376403491,
0.3894146749438));
#38570=CARTESIAN_POINT('Ctrl Pts',(-49.2018399117058,-3.8815753953419,0.774581617987376));
#38571=CARTESIAN_POINT('Ctrl Pts',(-49.2213416285762,-3.77033377843617,
1.14188486973955));
#38572=CARTESIAN_POINT('Ctrl Pts',(-49.2874993458189,-3.39295718714497,
2.38792617129552));
#38573=CARTESIAN_POINT('Ctrl Pts',(-49.3536570630616,-2.3367771868834,3.42838478771917));
#38574=CARTESIAN_POINT('Ctrl Pts',(-49.4198147803043,-1.08521689172491,
3.78703342403622));
#38575=CARTESIAN_POINT('Ctrl Pts',(-49.485972497547,0.16634340343358,4.14568206035329));
#38576=CARTESIAN_POINT('Ctrl Pts',(-49.5521302147897,1.61328399348899,3.82252071656374));
#38577=CARTESIAN_POINT('Ctrl Pts',(-49.6182879320324,2.59332711739344,2.96546325525251));
#38578=CARTESIAN_POINT('Ctrl Pts',(-49.6844456492752,3.57337024129788,2.10840579394128));
#38579=CARTESIAN_POINT('Ctrl Pts',(-49.7506033665179,4.08651589905138,0.717452215108368));
#38580=CARTESIAN_POINT('Ctrl Pts',(-49.8167610837606,3.89789269385868,-0.570745480739336));
#38581=CARTESIAN_POINT('Ctrl Pts',(-49.8829188010033,3.70926948866598,-1.85894317658704));
#38582=CARTESIAN_POINT('Ctrl Pts',(-49.949076518246,2.81887742052708,-3.04438498944954));
#38583=CARTESIAN_POINT('Ctrl Pts',(-50.0152342354887,1.63425697154039,-3.58448350663335));
#38584=CARTESIAN_POINT('Ctrl Pts',(-50.0813919527314,0.449636522553694,
-4.12458202381717));
#38585=CARTESIAN_POINT('Ctrl Pts',(-50.1475496699741,-1.0292123072808,-4.0193372453223));
#38586=CARTESIAN_POINT('Ctrl Pts',(-50.2137073872168,-2.12540706800835,
-3.31692065747272));
#38587=CARTESIAN_POINT('Ctrl Pts',(-50.2798651044595,-3.22160182873591,
-2.61450406962314));
#38588=CARTESIAN_POINT('Ctrl Pts',(-50.3460228217023,-3.93514252035653,
-1.31491567241883));
#38589=CARTESIAN_POINT('Ctrl Pts',(-50.412180538945,-3.93943513073482,-0.0129887955995017));
#38590=CARTESIAN_POINT('Ctrl Pts',(-50.412399185285,-3.93944931749318,-0.00868602400368631));
#38591=CARTESIAN_POINT('Ctrl Pts',(-50.412617831625,-3.93945575746534,-0.00438322686574803));
#38592=CARTESIAN_POINT('Ctrl Pts',(-50.412836477965,-3.9394544622989,-8.04257353526072E-5));
#38593=CARTESIAN_POINT('Ctrl Pts',(-50.5961635220349,-3.93944735561455,
0.000168331762536079));
#38594=CARTESIAN_POINT('Ctrl Pts',(-50.5304636192597,-3.93864051302073,
-1.29276418554459));
#38595=CARTESIAN_POINT('Ctrl Pts',(-50.4647637164844,-3.24056791593096,
-2.58644353485226));
#38596=CARTESIAN_POINT('Ctrl Pts',(-50.3990638137092,-2.15913104008258,
-3.29506752887434));
#38597=CARTESIAN_POINT('Ctrl Pts',(-50.3329060964666,-1.07015842328851,
-4.00862940412288));
#38598=CARTESIAN_POINT('Ctrl Pts',(-50.2667483792239,0.407539856527492,
-4.12895387179563));
#38599=CARTESIAN_POINT('Ctrl Pts',(-50.2005906619812,1.59760797049748,-3.6009673256178));
#38600=CARTESIAN_POINT('Ctrl Pts',(-50.1344329447385,2.78767608446746,-3.07298077943997));
#38601=CARTESIAN_POINT('Ctrl Pts',(-50.0682752274957,3.69011403259143,-1.89668321941156));
#38602=CARTESIAN_POINT('Ctrl Pts',(-50.002117510253,3.89186782276165,-0.61047665653478));
#38603=CARTESIAN_POINT('Ctrl Pts',(-49.9359597930103,4.09362161293187,0.675729906342009));
#38604=CARTESIAN_POINT('Ctrl Pts',(-49.8698020757676,3.59469124514835,2.07184547206718));
#38605=CARTESIAN_POINT('Ctrl Pts',(-49.8036443585249,2.62344165083307,2.93885535494938));
#38606=CARTESIAN_POINT('Ctrl Pts',(-49.7374866412822,1.6521920565178,3.80586523783157));
#38607=CARTESIAN_POINT('Ctrl Pts',(-49.6713289240395,0.208623235670778,
4.14376943787079));
#38608=CARTESIAN_POINT('Ctrl Pts',(-49.6051712067968,-1.0465303404107,3.7979061527243));
#38609=CARTESIAN_POINT('Ctrl Pts',(-49.539013489554,-2.30168391649217,3.4520428675778));
#38610=CARTESIAN_POINT('Ctrl Pts',(-49.4728557723114,-3.3684222478081,2.42241209724558));
#38611=CARTESIAN_POINT('Ctrl Pts',(-49.4066980550687,-3.7584895766171,1.18028513462752));
#38612=CARTESIAN_POINT('Ctrl Pts',(-49.3865198773907,-3.87746054773126,
0.80143502318402));
#38613=CARTESIAN_POINT('Ctrl Pts',(-49.3663416997128,-3.93348373764373,
0.402817308623724));
#38614=CARTESIAN_POINT('Ctrl Pts',(-49.3461635220349,-3.93028113905034,
0.00332252600905021));
#38615=CARTESIAN_POINT('Origin',(-27.25,0.,0.));
#38616=CARTESIAN_POINT('',(-47.912836477965,-3.92745622955471,-0.00190287763193742));
#38617=CARTESIAN_POINT('',(-48.0961635220349,-3.92766141711679,-0.00208726053621665));
#38618=CARTESIAN_POINT('',(-27.25,-3.933,-4.81653586104654E-16));
#38619=CARTESIAN_POINT('Ctrl Pts',(-47.912836477965,-3.92745622955471,-0.00190287763193742));
#38620=CARTESIAN_POINT('Ctrl Pts',(-47.9520585580458,-3.92405313224557,
0.776035286917171));
#38621=CARTESIAN_POINT('Ctrl Pts',(-47.9912806381266,-3.70062824945331,
1.55577560236864));
#38622=CARTESIAN_POINT('Ctrl Pts',(-48.0305027182074,-3.2702621470808,2.19652073651571));
#38623=CARTESIAN_POINT('Ctrl Pts',(-48.0966604354501,-2.54434351010488,
3.27729552771056));
#38624=CARTESIAN_POINT('Ctrl Pts',(-48.1628181526928,-1.22965336798294,
3.96261308582911));
#38625=CARTESIAN_POINT('Ctrl Pts',(-48.2289758699355,0.0720627412551513,
3.93879738218449));
#38626=CARTESIAN_POINT('Ctrl Pts',(-48.2951335871782,1.37377885049323,3.91498167853987));
#38627=CARTESIAN_POINT('Ctrl Pts',(-48.3612913044209,2.66252092684747,3.1820327131321));
#38628=CARTESIAN_POINT('Ctrl Pts',(-48.4274490216636,3.34842009607204,2.07542783945553));
#38629=CARTESIAN_POINT('Ctrl Pts',(-48.4936067389064,4.03431926529661,0.96882296577896));
#38630=CARTESIAN_POINT('Ctrl Pts',(-48.5597644561491,4.11737552739151,-0.511437816166413));
#38631=CARTESIAN_POINT('Ctrl Pts',(-48.6259221733918,3.55957328193336,-1.68782579288106));
#38632=CARTESIAN_POINT('Ctrl Pts',(-48.6920798906345,3.00177103647522,-2.86421376959571));
#38633=CARTESIAN_POINT('Ctrl Pts',(-48.7582376078772,1.80311028346402,-3.73672894107964));
#38634=CARTESIAN_POINT('Ctrl Pts',(-48.8243953251199,0.512228862821446,
-3.90601324225985));
#38635=CARTESIAN_POINT('Ctrl Pts',(-48.8905530423626,-0.778652557821136,
-4.07529754344005));
#38636=CARTESIAN_POINT('Ctrl Pts',(-48.9567107596053,-2.16175464609509,
-3.54135097431652));
#38637=CARTESIAN_POINT('Ctrl Pts',(-49.022868476848,-3.00401909907165,-2.54856569641061));
#38638=CARTESIAN_POINT('Ctrl Pts',(-49.0695244772204,-3.59800408328001,
-1.84842983583234));
#38639=CARTESIAN_POINT('Ctrl Pts',(-49.1161804775927,-3.92300850734398,
-0.920094817411913));
#38640=CARTESIAN_POINT('Ctrl Pts',(-49.1628364779651,-3.93064273659572,
0.00340251455877419));
#38641=CARTESIAN_POINT('Ctrl Pts',(-49.3461635220349,-3.93028113905034,
0.00332252600905021));
#38642=CARTESIAN_POINT('Ctrl Pts',(-49.3001839824701,-3.92298345285264,
-0.906996852497206));
#38643=CARTESIAN_POINT('Ctrl Pts',(-49.2542044429053,-3.60816375734389,
-1.82187028992255));
#38644=CARTESIAN_POINT('Ctrl Pts',(-49.2082249033405,-3.02985964262966,
-2.51779019021933));
#38645=CARTESIAN_POINT('Ctrl Pts',(-49.1420671860978,-2.19776605353114,
-3.51911539754416));
#38646=CARTESIAN_POINT('Ctrl Pts',(-49.0759094688551,-0.820182549032034,
-4.06714265728989));
#38647=CARTESIAN_POINT('Ctrl Pts',(-49.0097517516124,0.472358473597488,
-3.9110349486057));
#38648=CARTESIAN_POINT('Ctrl Pts',(-48.9435940343697,1.76489949622702,-3.75492723992151));
#38649=CARTESIAN_POINT('Ctrl Pts',(-48.877436317127,2.97239803698697,-2.89468456280739));
#38650=CARTESIAN_POINT('Ctrl Pts',(-48.8112785998842,3.54217112073391,-1.72404775106041));
#38651=CARTESIAN_POINT('Ctrl Pts',(-48.7451208826415,4.11194420448085,-0.553410939313448));
#38652=CARTESIAN_POINT('Ctrl Pts',(-48.6789631653988,4.0439918312148,0.92762000706637));
#38653=CARTESIAN_POINT('Ctrl Pts',(-48.6128054481561,3.36941641521032,2.04116386342701));
#38654=CARTESIAN_POINT('Ctrl Pts',(-48.5466477309134,2.69484099920583,3.15470771978765));
#38655=CARTESIAN_POINT('Ctrl Pts',(-48.4804900136707,1.4136425404629,3.90076448612912));
#38656=CARTESIAN_POINT('Ctrl Pts',(-48.414332296428,0.112237131383173,3.93785725019289));
#38657=CARTESIAN_POINT('Ctrl Pts',(-48.3481745791853,-1.18916827769656,
3.97495001425665));
#38658=CARTESIAN_POINT('Ctrl Pts',(-48.2820168619426,-2.51078063711309,
3.30307877604271));
#38659=CARTESIAN_POINT('Ctrl Pts',(-48.2158591446998,-3.2476860475286,2.22976506233225));
#38660=CARTESIAN_POINT('Ctrl Pts',(-48.1759606038115,-3.69210057501947,
1.5824686791246));
#38661=CARTESIAN_POINT('Ctrl Pts',(-48.1360620629232,-3.92385243391373,
0.789164405514797));
#38662=CARTESIAN_POINT('Ctrl Pts',(-48.0961635220349,-3.92766141711679,
-0.00208726053621665));
#38663=CARTESIAN_POINT('Origin',(-27.25,0.,0.));
#38664=CARTESIAN_POINT('',(-46.662836477965,-3.93759335115904,-0.00239393627812612));
#38665=CARTESIAN_POINT('',(-46.8461635220349,-3.93789469888383,-0.00220862991458794));
#38666=CARTESIAN_POINT('',(-27.25,-3.933,-4.81653586104654E-16));
#38667=CARTESIAN_POINT('Ctrl Pts',(-46.662836477965,-3.93759335115904,-0.00239393627812612));
#38668=CARTESIAN_POINT('Ctrl Pts',(-46.7217789212562,-3.92926765874005,
1.15900568512445));
#38669=CARTESIAN_POINT('Ctrl Pts',(-46.7807213645474,-3.38362267933311,
2.32720491863261));
#38670=CARTESIAN_POINT('Ctrl Pts',(-46.8396638078386,-2.48311790104751,
3.05833996574477));
#38671=CARTESIAN_POINT('Ctrl Pts',(-46.9058215250814,-1.47238035487552,
3.87897485992643));
#38672=CARTESIAN_POINT('Ctrl Pts',(-46.9719792423241,-0.0145871910493715,
4.14899229780223));
#38673=CARTESIAN_POINT('Ctrl Pts',(-47.0381369595668,1.22301650841775,3.7448028621961));
#38674=CARTESIAN_POINT('Ctrl Pts',(-47.1042946768095,2.46062020788489,3.34061342658998));
#38675=CARTESIAN_POINT('Ctrl Pts',(-47.1704523940522,3.478034442993,2.26221711750192));
#38676=CARTESIAN_POINT('Ctrl Pts',(-47.2366101112949,3.80957954011521,1.00320565394629));
#38677=CARTESIAN_POINT('Ctrl Pts',(-47.3027678285376,4.14112463723742,-0.255805809609345));
#38678=CARTESIAN_POINT('Ctrl Pts',(-47.3689255457803,3.78680059637373,-1.69543242763256));
#38679=CARTESIAN_POINT('Ctrl Pts',(-47.435083263023,2.90878472742779,-2.65674411000701));
#38680=CARTESIAN_POINT('Ctrl Pts',(-47.5012409802657,2.03076885848187,-3.61805579238144));
#38681=CARTESIAN_POINT('Ctrl Pts',(-47.5673986975084,0.629061161453717,
-4.10105253910711));
#38682=CARTESIAN_POINT('Ctrl Pts',(-47.6335564147511,-0.6547641057507,-3.88466238203473));
#38683=CARTESIAN_POINT('Ctrl Pts',(-47.6997141319938,-1.93858937295514,
-3.66827222496235));
#38684=CARTESIAN_POINT('Ctrl Pts',(-47.7658718492365,-3.10453221033583,
-2.75249516409189));
#38685=CARTESIAN_POINT('Ctrl Pts',(-47.8320295664793,-3.61893006311123,
-1.55649062152109));
#38686=CARTESIAN_POINT('Ctrl Pts',(-47.8589652036412,-3.82836343682328,
-1.0695460027322));
#38687=CARTESIAN_POINT('Ctrl Pts',(-47.8859008408031,-3.92979329567044,
-0.536149406412223));
#38688=CARTESIAN_POINT('Ctrl Pts',(-47.912836477965,-3.92745622955471,-0.00190287763193742));
#38689=CARTESIAN_POINT('Ctrl Pts',(-48.0961635220349,-3.92766141711679,
-0.00208726053621665));
#38690=CARTESIAN_POINT('Ctrl Pts',(-48.0699043456805,-3.93016829479786,
-0.522848586061526));
#38691=CARTESIAN_POINT('Ctrl Pts',(-48.0436451693261,-3.83393947565168,
-1.04272080444973));
#38692=CARTESIAN_POINT('Ctrl Pts',(-48.0173859929717,-3.63461882298519,
-1.51949429354273));
#38693=CARTESIAN_POINT('Ctrl Pts',(-47.951228275729,-3.13244772661179,-2.72068374650028));
#38694=CARTESIAN_POINT('Ctrl Pts',(-47.8850705584863,-1.9759070724505,-3.6483064632084));
#38695=CARTESIAN_POINT('Ctrl Pts',(-47.8189128412436,-0.694355951203478,
-3.8777811580271));
#38696=CARTESIAN_POINT('Ctrl Pts',(-47.7527551240009,0.587195170043544,
-4.1072558528458));
#38697=CARTESIAN_POINT('Ctrl Pts',(-47.6865974067582,1.9937567583763,-3.6385825257751));
#38698=CARTESIAN_POINT('Ctrl Pts',(-47.6204396895155,2.88153288605031,-2.68627718657711));
#38699=CARTESIAN_POINT('Ctrl Pts',(-47.5542819722727,3.76930901372432,-1.73397184737912));
#38700=CARTESIAN_POINT('Ctrl Pts',(-47.48812425503,4.13829968073957,-0.298034496053816));
#38701=CARTESIAN_POINT('Ctrl Pts',(-47.4219665377873,3.81961453009384,0.964293387932535));
#38702=CARTESIAN_POINT('Ctrl Pts',(-47.3558088205446,3.50092937944811,2.22662127191887));
#38703=CARTESIAN_POINT('Ctrl Pts',(-47.2896511033019,2.49456841114145,3.31533968856626));
#38704=CARTESIAN_POINT('Ctrl Pts',(-47.2234933860592,1.26115211887257,3.73213239711288));
#38705=CARTESIAN_POINT('Ctrl Pts',(-47.1573356688165,0.0277358266036876,
4.14892510565949));
#38706=CARTESIAN_POINT('Ctrl Pts',(-47.0911779515738,-1.43273578962741,
3.89379210610531));
#38707=CARTESIAN_POINT('Ctrl Pts',(-47.0250202343311,-2.451791695979,3.08351007393255));
#38708=CARTESIAN_POINT('Ctrl Pts',(-46.9654013302323,-3.37012743796263,
2.35331367686203));
#38709=CARTESIAN_POINT('Ctrl Pts',(-46.9057824261336,-3.92999159195356,
1.17228340405631));
#38710=CARTESIAN_POINT('Ctrl Pts',(-46.8461635220349,-3.93789469888383,
-0.00220862991458794));
#38711=CARTESIAN_POINT('Origin',(-27.25,0.,0.));
#38712=CARTESIAN_POINT('',(-45.412836477965,-3.93474092475559,0.00340612917001049));
#38713=CARTESIAN_POINT('',(-45.5961635220349,-3.93433860385037,0.003473953574826));
#38714=CARTESIAN_POINT('',(-27.25,-3.933,-4.81653586104654E-16));
#38715=CARTESIAN_POINT('Ctrl Pts',(-45.412836477965,-3.93474092475559,0.00340612917001049));
#38716=CARTESIAN_POINT('Ctrl Pts',(-45.4253415672239,-3.93699281657843,
0.250270820522606));
#38717=CARTESIAN_POINT('Ctrl Pts',(-45.4378466564828,-3.91575262884963,
0.496749281650563));
#38718=CARTESIAN_POINT('Ctrl Pts',(-45.4503517457417,-3.86962127480358,
0.738477519063283));
#38719=CARTESIAN_POINT('Ctrl Pts',(-45.5165094629844,-3.62556503387504,
2.01733191580052));
#38720=CARTESIAN_POINT('Ctrl Pts',(-45.5826671802271,-2.68482986023644,
3.16323228596122));
#38721=CARTESIAN_POINT('Ctrl Pts',(-45.6488248974698,-1.47799872934894,
3.65168969281581));
#38722=CARTESIAN_POINT('Ctrl Pts',(-45.7149826147126,-0.271167598461425,
4.14014709967041));
#38723=CARTESIAN_POINT('Ctrl Pts',(-45.7811403319553,1.201759489675,3.97116154321891));
#38724=CARTESIAN_POINT('Ctrl Pts',(-45.847298049198,2.26661051936538,3.22207923708846));
#38725=CARTESIAN_POINT('Ctrl Pts',(-45.9134557664407,3.33146154905574,2.47299693095802));
#38726=CARTESIAN_POINT('Ctrl Pts',(-45.9796134836834,3.98823652030005,1.14381787514865));
#38727=CARTESIAN_POINT('Ctrl Pts',(-46.0457712009261,3.93632360391267,-0.157080685809306));
#38728=CARTESIAN_POINT('Ctrl Pts',(-46.1119289181688,3.88441068752528,-1.45797924676727));
#38729=CARTESIAN_POINT('Ctrl Pts',(-46.1780866354115,3.12380988350618,-2.73059731287383));
#38730=CARTESIAN_POINT('Ctrl Pts',(-46.2442443526542,2.00265504132755,-3.39244611482919));
#38731=CARTESIAN_POINT('Ctrl Pts',(-46.3104020698969,0.88150019914892,-4.05429491678456));
#38732=CARTESIAN_POINT('Ctrl Pts',(-46.3765597871397,-0.600208681189243,
-4.10537445458874));
#38733=CARTESIAN_POINT('Ctrl Pts',(-46.4427175043824,-1.76428007847962,
-3.52230516299402));
#38734=CARTESIAN_POINT('Ctrl Pts',(-46.5088752216251,-2.92835147576999,
-2.9392358713993));
#38735=CARTESIAN_POINT('Ctrl Pts',(-46.5750329388678,-3.77478539001258,
-1.72201775040568));
#38736=CARTESIAN_POINT('Ctrl Pts',(-46.6411906561105,-3.91616138287496,
-0.427782514665089));
#38737=CARTESIAN_POINT('Ctrl Pts',(-46.648405930062,-3.93158009079269,-0.286631003204834));
#38738=CARTESIAN_POINT('Ctrl Pts',(-46.6556212040135,-3.93861251745559,
-0.144563414971144));
#38739=CARTESIAN_POINT('Ctrl Pts',(-46.662836477965,-3.93759335115904,-0.00239393627812612));
#38740=CARTESIAN_POINT('Ctrl Pts',(-46.8461635220349,-3.93789469888383,
-0.00220862991458794));
#38741=CARTESIAN_POINT('Ctrl Pts',(-46.8396247088909,-3.93876148669644,
-0.131023207527449));
#38742=CARTESIAN_POINT('Ctrl Pts',(-46.8330858957469,-3.93298872969746,
-0.259759136601678));
#38743=CARTESIAN_POINT('Ctrl Pts',(-46.826547082603,-3.9203211565074,-0.387813004366422));
#38744=CARTESIAN_POINT('Ctrl Pts',(-46.7603893653603,-3.79215451421213,
-1.68342298570133));
#38745=CARTESIAN_POINT('Ctrl Pts',(-46.6942316481175,-2.95818103314946,
-2.90921188357983));
#38746=CARTESIAN_POINT('Ctrl Pts',(-46.6280739308748,-1.80011789897827,
-3.50412506145166));
#38747=CARTESIAN_POINT('Ctrl Pts',(-46.5619162136321,-0.642054764807075,
-4.09903823932348));
#38748=CARTESIAN_POINT('Ctrl Pts',(-46.4957584963894,0.840098022472642,
-4.06307569718863));
#38749=CARTESIAN_POINT('Ctrl Pts',(-46.4296007791467,1.96794576144187,-3.41269781500477));
#38750=CARTESIAN_POINT('Ctrl Pts',(-46.363443061904,3.0957935004111,-2.76231993282091));
#38751=CARTESIAN_POINT('Ctrl Pts',(-46.2972853446612,3.86933619106982,-1.49752671058804));
#38752=CARTESIAN_POINT('Ctrl Pts',(-46.2311276274185,3.93451636568059,-0.197225415976034));
#38753=CARTESIAN_POINT('Ctrl Pts',(-46.1649699101758,3.99969654029137,1.10307587863597));
#38754=CARTESIAN_POINT('Ctrl Pts',(-46.0988121929332,3.35651419885418,2.43888524562711));
#38755=CARTESIAN_POINT('Ctrl Pts',(-46.0326544756904,2.29935970127119,3.19879068722626));
#38756=CARTESIAN_POINT('Ctrl Pts',(-45.9664967584477,1.2422052036882,3.95869612882542));
#38757=CARTESIAN_POINT('Ctrl Pts',(-45.900339041205,-0.228921450040587,
4.1426976450326));
#38758=CARTESIAN_POINT('Ctrl Pts',(-45.8341813239623,-1.44067231929053,
3.66657608197968));
#38759=CARTESIAN_POINT('Ctrl Pts',(-45.7680236067196,-2.65242318854047,
3.19045451892675));
#38760=CARTESIAN_POINT('Ctrl Pts',(-45.7018658894769,-3.60479827331157,
2.0542098766137));
#38761=CARTESIAN_POINT('Ctrl Pts',(-45.6357081722342,-3.86188690581226,
0.777911578028733));
#38762=CARTESIAN_POINT('Ctrl Pts',(-45.6225266221678,-3.91311035822352,
0.52361637825961));
#38763=CARTESIAN_POINT('Ctrl Pts',(-45.6093450721013,-3.93673211827082,
0.263761285985406));
#38764=CARTESIAN_POINT('Ctrl Pts',(-45.5961635220349,-3.93433860385037,
0.003473953574826));
#38765=CARTESIAN_POINT('Origin',(-27.25,0.,0.));
#38766=CARTESIAN_POINT('',(-44.162836477965,-3.92656883402695,0.000277810122669975));
#38767=CARTESIAN_POINT('',(-44.3461635220349,-3.92655167676131,5.76543438965291E-5));
#38768=CARTESIAN_POINT('',(-27.25,-3.933,-4.81653586104654E-16));
#38769=CARTESIAN_POINT('Ctrl Pts',(-44.162836477965,-3.92656883402695,0.000277810122669975));
#38770=CARTESIAN_POINT('Ctrl Pts',(-44.1950619304343,-3.92697179969628,
0.639804442392745));
#38771=CARTESIAN_POINT('Ctrl Pts',(-44.2272873829036,-3.77958365909042,
1.27915600723495));
#38772=CARTESIAN_POINT('Ctrl Pts',(-44.2595128353729,-3.48339515771394,
1.83991196305406));
#38773=CARTESIAN_POINT('Ctrl Pts',(-44.3256705526156,-2.8753306117383,2.99112416100792));
#38774=CARTESIAN_POINT('Ctrl Pts',(-44.3918282698584,-1.64012251647393,
3.81108226155247));
#38775=CARTESIAN_POINT('Ctrl Pts',(-44.4579859871011,-0.343136760086226,
3.92448404512643));
#38776=CARTESIAN_POINT('Ctrl Pts',(-44.5241437043438,0.953848996301473,
4.03788582870038));
#38777=CARTESIAN_POINT('Ctrl Pts',(-44.5903014215865,2.31261241381248,3.44473129530375));
#38778=CARTESIAN_POINT('Ctrl Pts',(-44.6564591388292,3.11123521868153,2.41651262579156));
#38779=CARTESIAN_POINT('Ctrl Pts',(-44.7226168560719,3.90985802355059,1.38829395627936));
#38780=CARTESIAN_POINT('Ctrl Pts',(-44.7887745733146,4.14834021577764,-0.0749888493484113));
#38781=CARTESIAN_POINT('Ctrl Pts',(-44.8549322905573,3.71752634460343,-1.30357805050323));
#38782=CARTESIAN_POINT('Ctrl Pts',(-44.9210900078001,3.28671247342922,-2.53216725165805));
#38783=CARTESIAN_POINT('Ctrl Pts',(-44.9872477250427,2.18660253885373,-3.52606284833993));
#38784=CARTESIAN_POINT('Ctrl Pts',(-45.0534054422855,0.920726782158098,
-3.83034985989415));
#38785=CARTESIAN_POINT('Ctrl Pts',(-45.1195631595282,-0.345148974537538,
-4.13463687144837));
#38786=CARTESIAN_POINT('Ctrl Pts',(-45.1857208767709,-1.77679055335334,
-3.74931529787494));
#38787=CARTESIAN_POINT('Ctrl Pts',(-45.2518785940136,-2.71892268865198,
-2.85075029943133));
#38788=CARTESIAN_POINT('Ctrl Pts',(-45.3055312219974,-3.48297361231569,
-2.12203148037195));
#38789=CARTESIAN_POINT('Ctrl Pts',(-45.3591838499812,-3.92507926527206,
-1.05575779787344));
#38790=CARTESIAN_POINT('Ctrl Pts',(-45.412836477965,-3.93474092475559,0.00340612917001049));
#38791=CARTESIAN_POINT('Ctrl Pts',(-45.5961635220349,-3.93433860385037,
0.003473953574826));
#38792=CARTESIAN_POINT('Ctrl Pts',(-45.5431873548586,-3.92471915701462,
-1.04261130697134));
#38793=CARTESIAN_POINT('Ctrl Pts',(-45.4902111876823,-3.49489926040405,
-2.0956781390531));
#38794=CARTESIAN_POINT('Ctrl Pts',(-45.437235020506,-2.74786054164776,-2.82286721972017));
#38795=CARTESIAN_POINT('Ctrl Pts',(-45.3710773032633,-1.81494336475224,
-3.73099576402723));
#38796=CARTESIAN_POINT('Ctrl Pts',(-45.3049195860206,-0.387306830730913,
-4.13090089778447));
#38797=CARTESIAN_POINT('Ctrl Pts',(-45.2387618687779,0.881606939911368,
-3.8395424336782));
#38798=CARTESIAN_POINT('Ctrl Pts',(-45.1726041515352,2.15052071055363,-3.54818396957193));
#38799=CARTESIAN_POINT('Ctrl Pts',(-45.1064464342925,3.26071171781685,-2.56556190760216));
#38800=CARTESIAN_POINT('Ctrl Pts',(-45.0402887170498,3.70403552250813,-1.34143122988594));
#38801=CARTESIAN_POINT('Ctrl Pts',(-44.9741309998071,4.14735932719942,-0.117300552169714));
#38802=CARTESIAN_POINT('Ctrl Pts',(-44.9079732825644,3.92381592931878,1.34833874129297));
#38803=CARTESIAN_POINT('Ctrl Pts',(-44.8418155653217,3.13572315868845,2.3846503241734));
#38804=CARTESIAN_POINT('Ctrl Pts',(-44.7756578480789,2.34763038805812,3.42096190705384));
#38805=CARTESIAN_POINT('Ctrl Pts',(-44.7095001308362,0.994988244678091,
4.02794577935202));
#38806=CARTESIAN_POINT('Ctrl Pts',(-44.6433424135935,-0.30308676007683,
3.92777994704152));
#38807=CARTESIAN_POINT('Ctrl Pts',(-44.5771846963508,-1.60116176483176,
3.82761411473103));
#38808=CARTESIAN_POINT('Ctrl Pts',(-44.5110269791081,-2.84466963096158,
3.02029857781185));
#38809=CARTESIAN_POINT('Ctrl Pts',(-44.4448692618654,-3.46444559030253,
1.87534894042382));
#38810=CARTESIAN_POINT('Ctrl Pts',(-44.4119673485886,-3.77267591799805,
1.30593640254117));
#38811=CARTESIAN_POINT('Ctrl Pts',(-44.3790654353117,-3.92663703969061,
0.653015960009206));
#38812=CARTESIAN_POINT('Ctrl Pts',(-44.3461635220349,-3.92655167676131,
5.76543438965291E-5));
#38813=CARTESIAN_POINT('Origin',(-27.25,0.,0.));
#38814=CARTESIAN_POINT('',(-42.912836477965,-3.93372101951109,-0.00354898223331679));
#38815=CARTESIAN_POINT('',(-43.0961635220349,-3.93412692362359,-0.00350358252896577));
#38816=CARTESIAN_POINT('',(-27.25,-3.933,-4.81653586104654E-16));
#38817=CARTESIAN_POINT('Ctrl Pts',(-42.912836477965,-3.93372101951109,-0.00354898223331679));
#38818=CARTESIAN_POINT('Ctrl Pts',(-42.9647822936447,-3.92424142884988,
1.02260461028873));
#38819=CARTESIAN_POINT('Ctrl Pts',(-43.0167281093244,-3.51272955475539,
2.05549339592713));
#38820=CARTESIAN_POINT('Ctrl Pts',(-43.0686739250041,-2.79138702348944,
2.779833869437));
#38821=CARTESIAN_POINT('Ctrl Pts',(-43.1348316422469,-1.87269175238464,
3.70234729245046));
#38822=CARTESIAN_POINT('Ctrl Pts',(-43.2009893594896,-0.45144070276789,
4.12438494387334));
#38823=CARTESIAN_POINT('Ctrl Pts',(-43.2671470767323,0.82184669867214,3.85277638339627));
#38824=CARTESIAN_POINT('Ctrl Pts',(-43.333304793975,2.09513410011217,3.5811678229192));
#38825=CARTESIAN_POINT('Ctrl Pts',(-43.3994625112177,3.22045785337548,2.61591305054217));
#38826=CARTESIAN_POINT('Ctrl Pts',(-43.4656202284604,3.68274712491062,1.3988178832632));
#38827=CARTESIAN_POINT('Ctrl Pts',(-43.5317779457031,4.14503639644575,0.181722715984218));
#38828=CARTESIAN_POINT('Ctrl Pts',(-43.5979356629459,3.94429118625271,-1.28721284619671));
#38829=CARTESIAN_POINT('Ctrl Pts',(-43.6640933801886,3.17239438798388,-2.3356437450225));
#38830=CARTESIAN_POINT('Ctrl Pts',(-43.7302510974313,2.40049758971504,-3.38407464384829));
#38831=CARTESIAN_POINT('Ctrl Pts',(-43.7964088146739,1.05744920337041,-4.01200087931894));
#38832=CARTESIAN_POINT('Ctrl Pts',(-43.8625665319166,-0.242025408816761,
-3.93201494886037));
#38833=CARTESIAN_POINT('Ctrl Pts',(-43.9287242491593,-1.54150002100394,
-3.8520290184018));
#38834=CARTESIAN_POINT('Ctrl Pts',(-43.9948819664021,-2.79740085903366,
-3.06413092201401));
#38835=CARTESIAN_POINT('Ctrl Pts',(-44.0610396836448,-3.43489077970507,
-1.92894872613853));
#38836=CARTESIAN_POINT('Ctrl Pts',(-44.0949719484182,-3.76185908635389,
-1.34671426518835));
#38837=CARTESIAN_POINT('Ctrl Pts',(-44.1289042131916,-3.9261445253908,-0.673121175865286));
#38838=CARTESIAN_POINT('Ctrl Pts',(-44.162836477965,-3.92656883402695,0.000277810122669975));
#38839=CARTESIAN_POINT('Ctrl Pts',(-44.3461635220349,-3.92655167676131,
5.76543438965291E-5));
#38840=CARTESIAN_POINT('Ctrl Pts',(-44.312907718069,-3.92646539567429,-0.659923825407093));
#38841=CARTESIAN_POINT('Ctrl Pts',(-44.2796519141031,-3.7690009817897,-1.31994398717828));
#38842=CARTESIAN_POINT('Ctrl Pts',(-44.2463961101372,-3.45438842079276,
-1.89381032176095));
#38843=CARTESIAN_POINT('Ctrl Pts',(-44.1802383928945,-2.82851123938996,
-3.03543620870082));
#38844=CARTESIAN_POINT('Ctrl Pts',(-44.1140806756519,-1.58071282403231,
-3.83610424472369));
#38845=CARTESIAN_POINT('Ctrl Pts',(-44.0479229584092,-0.282121765970689,
-3.9293414468179));
#38846=CARTESIAN_POINT('Ctrl Pts',(-43.9817652411665,1.01646929209093,-4.0225786489121));
#38847=CARTESIAN_POINT('Ctrl Pts',(-43.9156075239237,2.36585299285652,-3.40838501707761));
#38848=CARTESIAN_POINT('Ctrl Pts',(-43.849449806681,3.14840424353069,-2.36788251732077));
#38849=CARTESIAN_POINT('Ctrl Pts',(-43.7832920894383,3.93095549420486,-1.32738001756392));
#38850=CARTESIAN_POINT('Ctrl Pts',(-43.7171343721956,4.14667429478762,0.139431350115277));
#38851=CARTESIAN_POINT('Ctrl Pts',(-43.6509766549529,3.69682420422663,1.36117879044582));
#38852=CARTESIAN_POINT('Ctrl Pts',(-43.5848189377102,3.24697411366564,2.58292623077635));
#38853=CARTESIAN_POINT('Ctrl Pts',(-43.5186612204675,2.13155513196088,3.55960974375823));
#38854=CARTESIAN_POINT('Ctrl Pts',(-43.4525035032247,0.861104589369346,
3.84419247471851));
#38855=CARTESIAN_POINT('Ctrl Pts',(-43.386345785982,-0.409345953222192,
4.12877520567879));
#38856=CARTESIAN_POINT('Ctrl Pts',(-43.3201880687393,-1.83482805670052,
3.7212571546175));
#38857=CARTESIAN_POINT('Ctrl Pts',(-43.2540303514966,-2.76288570285569,
2.80816300977543));
#38858=CARTESIAN_POINT('Ctrl Pts',(-43.2014080750094,-3.50106876127229,
2.08188201715149));
#38859=CARTESIAN_POINT('Ctrl Pts',(-43.1487857985221,-3.92454556393865,
1.03573746106949));
#38860=CARTESIAN_POINT('Ctrl Pts',(-43.0961635220349,-3.93412692362359,
-0.00350358252896577));
#38861=CARTESIAN_POINT('Origin',(-27.25,0.,0.));
#38862=CARTESIAN_POINT('',(-41.662836477965,-3.93831397248116,0.00190595679815712));
#38863=CARTESIAN_POINT('',(-41.8461635220348,-3.93804437062894,0.00210735149479831));
#38864=CARTESIAN_POINT('',(-27.25,-3.933,-4.81653586104654E-16));
#38865=CARTESIAN_POINT('Ctrl Pts',(-41.662836477965,-3.93831397248116,0.00190595679815712));
#38866=CARTESIAN_POINT('Ctrl Pts',(-41.6683449396124,-3.93896170190249,
0.110392148591447));
#38867=CARTESIAN_POINT('Ctrl Pts',(-41.6738534012598,-3.93486758661977,
0.218828713482624));
#38868=CARTESIAN_POINT('Ctrl Pts',(-41.6793618629072,-3.92587342546206,
0.326857314168025));
#38869=CARTESIAN_POINT('Ctrl Pts',(-41.7455195801499,-3.8178517655515,1.62430224085299));
#38870=CARTESIAN_POINT('Ctrl Pts',(-41.8116772973927,-3.00302364739276,
2.86290042554131));
#38871=CARTESIAN_POINT('Ctrl Pts',(-41.8778350146354,-1.85434325133095,
3.47573430555584));
#38872=CARTESIAN_POINT('Ctrl Pts',(-41.9439927318781,-0.70566285526915,
4.08856818557036));
#38873=CARTESIAN_POINT('Ctrl Pts',(-42.0101504491208,0.776869818695703,
4.07563776091109));
#38874=CARTESIAN_POINT('Ctrl Pts',(-42.0763081663635,1.91468619158182,3.44286140359153));
#38875=CARTESIAN_POINT('Ctrl Pts',(-42.1424658836062,3.05250256446794,2.81008504627197));
#38876=CARTESIAN_POINT('Ctrl Pts',(-42.2086236008489,3.84560263627532,1.55746275629211));
#38877=CARTESIAN_POINT('Ctrl Pts',(-42.2747813180916,3.93097734948523,0.258331055834204));
#38878=CARTESIAN_POINT('Ctrl Pts',(-42.3409390353344,4.01635206269515,-1.0408006446237));
#38879=CARTESIAN_POINT('Ctrl Pts',(-42.4070967525771,3.39400141730759,-2.38644175555967));
#38880=CARTESIAN_POINT('Ctrl Pts',(-42.4732544698198,2.34878091801755,-3.16268020130568));
#38881=CARTESIAN_POINT('Ctrl Pts',(-42.5394121870625,1.30356041872751,-3.93891864705171));
#38882=CARTESIAN_POINT('Ctrl Pts',(-42.6055699043052,-0.164529934465034,
-4.14575442760779));
#38883=CARTESIAN_POINT('Ctrl Pts',(-42.6717276215479,-1.3835319430817,-3.68851694032262));
#38884=CARTESIAN_POINT('Ctrl Pts',(-42.7378853387906,-2.60253395169839,
-3.23127945303743));
#38885=CARTESIAN_POINT('Ctrl Pts',(-42.8040430560333,-3.57244761573919,
-2.10996869791097));
#38886=CARTESIAN_POINT('Ctrl Pts',(-42.870200773276,-3.84933470146315,-0.837818723045716));
#38887=CARTESIAN_POINT('Ctrl Pts',(-42.884412674839,-3.90881516981029,-0.56453737402596));
#38888=CARTESIAN_POINT('Ctrl Pts',(-42.898624576402,-3.93631454908748,-0.284295249369827));
#38889=CARTESIAN_POINT('Ctrl Pts',(-42.912836477965,-3.93372101951109,-0.00354898223331679));
#38890=CARTESIAN_POINT('Ctrl Pts',(-43.0961635220349,-3.93412692362359,
-0.00350358252896577));
#38891=CARTESIAN_POINT('Ctrl Pts',(-43.0826280812794,-3.93659142981811,
-0.270815955069072));
#38892=CARTESIAN_POINT('Ctrl Pts',(-43.0690926405239,-3.91167198021206,
-0.537671580660341));
#38893=CARTESIAN_POINT('Ctrl Pts',(-43.0555571997685,-3.85768057402877,
-0.79850953987816));
#38894=CARTESIAN_POINT('Ctrl Pts',(-42.9893994825258,-3.59378461021468,
-2.07341770606684));
#38895=CARTESIAN_POINT('Ctrl Pts',(-42.9232417652831,-2.63535949375449,
-3.20456379982134));
#38896=CARTESIAN_POINT('Ctrl Pts',(-42.8570840480404,-1.42108504652191,
-3.67421204982336));
#38897=CARTESIAN_POINT('Ctrl Pts',(-42.7909263307977,-0.20681059928933,
-4.14386029982538));
#38898=CARTESIAN_POINT('Ctrl Pts',(-42.7247686135549,1.26331317871563,-3.95201070607491));
#38899=CARTESIAN_POINT('Ctrl Pts',(-42.6586108963122,2.31639737213419,-3.18647455833013));
#38900=CARTESIAN_POINT('Ctrl Pts',(-42.5924531790695,3.36948156555278,-2.42093841058533));
#38901=CARTESIAN_POINT('Ctrl Pts',(-42.5262954618268,4.00552617438494,-1.08171570884617));
#38902=CARTESIAN_POINT('Ctrl Pts',(-42.4601377445841,3.93340784333217,0.218219235009942));
#38903=CARTESIAN_POINT('Ctrl Pts',(-42.3939800273414,3.86128951227941,1.51815417886602));
#38904=CARTESIAN_POINT('Ctrl Pts',(-42.3278223100986,3.08100824134177,2.77880136483906));
#38905=CARTESIAN_POINT('Ctrl Pts',(-42.2616645928559,1.94970580723992,3.42315120345717));
#38906=CARTESIAN_POINT('Ctrl Pts',(-42.1955068756132,0.818403373138075,
4.06750104207528));
#38907=CARTESIAN_POINT('Ctrl Pts',(-42.1293491583706,-0.663920224127962,
4.09555353333847));
#38908=CARTESIAN_POINT('Ctrl Pts',(-42.0631914411279,-1.81879210186756,
3.49446879893061));
#38909=CARTESIAN_POINT('Ctrl Pts',(-41.9970337238852,-2.97366397960716,
2.89338406452276));
#38910=CARTESIAN_POINT('Ctrl Pts',(-41.9308760066424,-3.80108413782031,
1.66316210444388));
#38911=CARTESIAN_POINT('Ctrl Pts',(-41.8647182893997,-3.92233490583468,
0.366886607804419));
#38912=CARTESIAN_POINT('Ctrl Pts',(-41.8585333669447,-3.93367034225883,
0.245700996191627));
#38913=CARTESIAN_POINT('Ctrl Pts',(-41.8523484444898,-3.93883391417578,
0.123938081903965));
#38914=CARTESIAN_POINT('Ctrl Pts',(-41.8461635220348,-3.93804437062894,
0.00210735149479831));
#38915=CARTESIAN_POINT('Origin',(-27.25,0.,0.));
#38916=CARTESIAN_POINT('',(-40.412836477965,-3.92801100457036,0.00235306236043675));
#38917=CARTESIAN_POINT('',(-40.5961635220348,-3.92777652835409,0.00218069315271673));
#38918=CARTESIAN_POINT('',(-27.25,-3.933,-4.81653586104654E-16));
#38919=CARTESIAN_POINT('Ctrl Pts',(-40.412836477965,-3.92801100457036,0.00235306236043675));
#38920=CARTESIAN_POINT('Ctrl Pts',(-40.4380653028228,-3.93074080988322,
0.502569384095045));
#38921=CARTESIAN_POINT('Ctrl Pts',(-40.4632941276807,-3.84214798031435,
1.00185495457367));
#38922=CARTESIAN_POINT('Ctrl Pts',(-40.4885229525385,-3.65778817178925,
1.46284091646802));
#38923=CARTESIAN_POINT('Ctrl Pts',(-40.5546806697812,-3.17434020494728,
2.67168750729197));
#38924=CARTESIAN_POINT('Ctrl Pts',(-40.6208383870239,-2.03235131675089,
3.61716712340826));
#38925=CARTESIAN_POINT('Ctrl Pts',(-40.6869961042666,-0.754520123348716,
3.86652521523346));
#38926=CARTESIAN_POINT('Ctrl Pts',(-40.7531538215093,0.523311070053491,
4.11588330705867));
#38927=CARTESIAN_POINT('Ctrl Pts',(-40.819311538752,1.93698456866149,3.66911987459282));
#38928=CARTESIAN_POINT('Ctrl Pts',(-40.8854692559947,2.83944925924138,2.73072257118293));
#38929=CARTESIAN_POINT('Ctrl Pts',(-40.9516269732374,3.74191394982125,1.79232526777306));
#38930=CARTESIAN_POINT('Ctrl Pts',(-41.0177846904802,4.133169832373,0.362294093419191));
#38931=CARTESIAN_POINT('Ctrl Pts',(-41.0839424077229,3.83413555988564,-0.904832782891263));
#38932=CARTESIAN_POINT('Ctrl Pts',(-41.1501001249656,3.53510128739829,-2.17195965920172));
#38933=CARTESIAN_POINT('Ctrl Pts',(-41.2162578422083,2.54577685987183,-3.27618223746875));
#38934=CARTESIAN_POINT('Ctrl Pts',(-41.282415559451,1.31898499260147,-3.71208788229299));
#38935=CARTESIAN_POINT('Ctrl Pts',(-41.3485732766937,0.0921931253310943,
-4.14799352711723));
#38936=CARTESIAN_POINT('Ctrl Pts',(-41.4147309939364,-1.3720661816832,-3.91558223849864));
#38937=CARTESIAN_POINT('Ctrl Pts',(-41.4808887111791,-2.40358823435914,
-3.12123075984854));
#38938=CARTESIAN_POINT('Ctrl Pts',(-41.5415379667744,-3.34922310860086,
-2.39301902780813));
#38939=CARTESIAN_POINT('Ctrl Pts',(-41.6021872223697,-3.93118234304533,
-1.19254853808352));
#38940=CARTESIAN_POINT('Ctrl Pts',(-41.662836477965,-3.93831397248116,0.00190595679815712));
#38941=CARTESIAN_POINT('Ctrl Pts',(-41.8461635220348,-3.93804437062894,
0.00210735149479831));
#38942=CARTESIAN_POINT('Ctrl Pts',(-41.7861907272471,-3.93038847300766,
-1.17923800034984));
#38943=CARTESIAN_POINT('Ctrl Pts',(-41.7262179324593,-3.36299512682459,
-2.36695971479872));
#38944=CARTESIAN_POINT('Ctrl Pts',(-41.6662451376716,-2.4353015692775,-3.09655020356362));
#38945=CARTESIAN_POINT('Ctrl Pts',(-41.6000874204289,-1.41193608689036,
-3.90138248509218));
#38946=CARTESIAN_POINT('Ctrl Pts',(-41.5339297031862,0.0498762556995175,
-4.14871801494928));
#38947=CARTESIAN_POINT('Ctrl Pts',(-41.4677719859434,1.28105076210131,-3.72534908987534));
#38948=CARTESIAN_POINT('Ctrl Pts',(-41.4016142687007,2.5122252685031,-3.3019801648014));
#38949=CARTESIAN_POINT('Ctrl Pts',(-41.335456551458,3.51276193871678,-2.20790678479643));
#38950=CARTESIAN_POINT('Ctrl Pts',(-41.2692988342153,3.82470611282222,-0.943896205658093));
#38951=CARTESIAN_POINT('Ctrl Pts',(-41.2031411169726,4.13665028692766,0.320114373480223));
#38952=CARTESIAN_POINT('Ctrl Pts',(-41.1369833997299,3.76000196492484,1.75406215175193));
#38953=CARTESIAN_POINT('Ctrl Pts',(-41.0708256824872,2.86715648158494,2.70161629522418));
#38954=CARTESIAN_POINT('Ctrl Pts',(-41.0046679652445,1.97431099824503,3.64917043869645));
#38955=CARTESIAN_POINT('Ctrl Pts',(-40.9385102480018,0.565268353568015,
4.1103309473693));
#38956=CARTESIAN_POINT('Ctrl Pts',(-40.8723525307591,-0.715039922831877,
3.87402049623798));
#38957=CARTESIAN_POINT('Ctrl Pts',(-40.8061948135164,-1.99534819923177,
3.63771004510666));
#38958=CARTESIAN_POINT('Ctrl Pts',(-40.7400370962736,-3.14692210735452,
2.70392863417116));
#38959=CARTESIAN_POINT('Ctrl Pts',(-40.6738793790309,-3.64267588096367,
1.50007643897266));
#38960=CARTESIAN_POINT('Ctrl Pts',(-40.6479740933656,-3.83679749912515,
1.02868570308809));
#38961=CARTESIAN_POINT('Ctrl Pts',(-40.6220688077002,-3.930364852657,0.515886099618727));
#38962=CARTESIAN_POINT('Ctrl Pts',(-40.5961635220348,-3.92777652835409,
0.00218069315271673));
#38963=CARTESIAN_POINT('Origin',(-27.25,0.,0.));
#38964=CARTESIAN_POINT('',(-39.162836477965,-3.92975286260395,-0.00317618749887255));
#38965=CARTESIAN_POINT('',(-39.3461635220348,-3.93009648465997,-0.00327554246926138));
#38966=CARTESIAN_POINT('',(-27.25,-3.933,-4.81653586104654E-16));
#38967=CARTESIAN_POINT('Ctrl Pts',(-39.162836477965,-3.92975286260395,-0.00317618749887255));
#38968=CARTESIAN_POINT('Ctrl Pts',(-39.2077856660332,-3.92299702030768,
0.887046174022243));
#38969=CARTESIAN_POINT('Ctrl Pts',(-39.2527348541015,-3.6233189159279,1.78138571892125));
#38970=CARTESIAN_POINT('Ctrl Pts',(-39.2976840421697,-3.06861220208183,
2.47041231574991));
#38971=CARTESIAN_POINT('Ctrl Pts',(-39.3638417594124,-2.2521763218261,3.48454468887551));
#38972=CARTESIAN_POINT('Ctrl Pts',(-39.4299994766551,-0.883273592225803,
4.05390893270202));
#38973=CARTESIAN_POINT('Ctrl Pts',(-39.4961571938978,0.411536858342489,
3.91790189652574));
#38974=CARTESIAN_POINT('Ctrl Pts',(-39.5623149111405,1.7063473089108,3.78189486034945));
#38975=CARTESIAN_POINT('Ctrl Pts',(-39.6284726283832,2.92706548044712,2.94051654417035));
#38976=CARTESIAN_POINT('Ctrl Pts',(-39.6946303456259,3.51495765359173,1.77887339348006));
#38977=CARTESIAN_POINT('Ctrl Pts',(-39.7607880628686,4.10284982673633,0.61723024278978));
#38978=CARTESIAN_POINT('Ctrl Pts',(-39.8269457801114,4.05791600148925,-0.864677742411652));
#38979=CARTESIAN_POINT('Ctrl Pts',(-39.8931034973541,3.40072279501961,-1.98856790882493));
#38980=CARTESIAN_POINT('Ctrl Pts',(-39.9592612145968,2.74352958854996,-3.11245807523822));
#38981=CARTESIAN_POINT('Ctrl Pts',(-40.0254189318395,1.47407700085769,-3.87833042286331));
#38982=CARTESIAN_POINT('Ctrl Pts',(-40.0915766490822,0.173404933216231,
-3.93563826916431));
#38983=CARTESIAN_POINT('Ctrl Pts',(-40.1577343663249,-1.12726713442519,
-3.9929461154653));
#38984=CARTESIAN_POINT('Ctrl Pts',(-40.2238920835676,-2.45915868201583,
-3.34168946044224));
#38985=CARTESIAN_POINT('Ctrl Pts',(-40.2900498008103,-3.21265093306733,
-2.27995435016492));
#38986=CARTESIAN_POINT('Ctrl Pts',(-40.3309786931952,-3.67880370467823,
-1.62310517397008));
#38987=CARTESIAN_POINT('Ctrl Pts',(-40.3719075855801,-3.92358242303668,
-0.809151243401977));
#38988=CARTESIAN_POINT('Ctrl Pts',(-40.412836477965,-3.92801100457036,0.00235306236043675));
#38989=CARTESIAN_POINT('Ctrl Pts',(-40.5961635220348,-3.92777652835409,
0.00218069315271673));
#38990=CARTESIAN_POINT('Ctrl Pts',(-40.5559110904575,-3.92375471024914,
-0.796030605954551));
#38991=CARTESIAN_POINT('Ctrl Pts',(-40.5156586588801,-3.68757556068199,
-1.59642886698926));
#38992=CARTESIAN_POINT('Ctrl Pts',(-40.4754062273028,-3.23574061561438,
-2.24706465527338));
#38993=CARTESIAN_POINT('Ctrl Pts',(-40.4092485100601,-2.49311793756043,
-3.31643057485933));
#38994=CARTESIAN_POINT('Ctrl Pts',(-40.3430907928174,-1.16793894235701,
-3.98123943456976));
#38995=CARTESIAN_POINT('Ctrl Pts',(-40.2769330755747,0.13324998928991,-3.93720222199338));
#38996=CARTESIAN_POINT('Ctrl Pts',(-40.210775358332,1.43443892093683,-3.89316500941701));
#38997=CARTESIAN_POINT('Ctrl Pts',(-40.1446176410892,2.71163778902724,-3.14028172455383));
#38998=CARTESIAN_POINT('Ctrl Pts',(-40.0784599238465,3.3802611498694,-2.02315383873767));
#38999=CARTESIAN_POINT('Ctrl Pts',(-40.0123022066038,4.04888451071156,-0.906025952921513));
#39000=CARTESIAN_POINT('Ctrl Pts',(-39.9461444893611,4.10893236430546,0.575346533847623));
#39001=CARTESIAN_POINT('Ctrl Pts',(-39.8799867721184,3.53292026636216,1.74292607073361));
#39002=CARTESIAN_POINT('Ctrl Pts',(-39.8138290548757,2.95690816841886,2.9105056076196));
#39003=CARTESIAN_POINT('Ctrl Pts',(-39.747671337633,1.74483611893836,3.76429219462244));
#39004=CARTESIAN_POINT('Ctrl Pts',(-39.6815136203903,0.451480429217691,
3.91350000875799));
#39005=CARTESIAN_POINT('Ctrl Pts',(-39.6153559031476,-0.84187526050298,
4.06270782289354));
#39006=CARTESIAN_POINT('Ctrl Pts',(-39.5491981859049,-2.21651459046383,
3.5073368641618));
#39007=CARTESIAN_POINT('Ctrl Pts',(-39.4830404686621,-3.0432527385527,2.50158543044344));
#39008=CARTESIAN_POINT('Ctrl Pts',(-39.4374148197864,-3.61341244219722,
1.80796927070229));
#39009=CARTESIAN_POINT('Ctrl Pts',(-39.3917891709106,-3.92298120014008,
0.900144640920363));
#39010=CARTESIAN_POINT('Ctrl Pts',(-39.3461635220348,-3.93009648465997,
-0.00327554246926138));
#39011=CARTESIAN_POINT('Origin',(-27.25,0.,0.));
#39012=CARTESIAN_POINT('',(-37.912836477965,-3.93936327777038,-0.000544856984334152));
#39013=CARTESIAN_POINT('',(-38.0961635220349,-3.93942817610916,-0.000298174263498583));
#39014=CARTESIAN_POINT('',(-27.25,-3.933,-4.81653586104654E-16));
#39015=CARTESIAN_POINT('Ctrl Pts',(-37.912836477965,-3.93936327777038,-0.000544856984334152));
#39016=CARTESIAN_POINT('Ctrl Pts',(-37.9775060292436,-3.93689177231164,
1.2721842897132));
#39017=CARTESIAN_POINT('Ctrl Pts',(-38.0421755805223,-3.26357656031174,
2.54715895566795));
#39018=CARTESIAN_POINT('Ctrl Pts',(-38.1068451318009,-2.21006500503054,
3.2611241206237));
#39019=CARTESIAN_POINT('Ctrl Pts',(-38.1730028490436,-1.13231020067255,
3.991518944314));
#39020=CARTESIAN_POINT('Ctrl Pts',(-38.2391605662863,0.343340319979478,
4.13478745500189));
#39021=CARTESIAN_POINT('Ctrl Pts',(-38.305318283529,1.54146800159971,3.62535436290282));
#39022=CARTESIAN_POINT('Ctrl Pts',(-38.3714760007717,2.73959568321995,3.11592127080375));
#39023=CARTESIAN_POINT('Ctrl Pts',(-38.4376337180145,3.66020052580842,1.95378657591777));
#39024=CARTESIAN_POINT('Ctrl Pts',(-38.5037914352572,3.88191338802384,0.670869811852932));
#39025=CARTESIAN_POINT('Ctrl Pts',(-38.5699491524999,4.10362625023927,-0.612046952211922));
#39026=CARTESIAN_POINT('Ctrl Pts',(-38.6361068697426,3.62644713208157,-2.01574578545561));
#39027=CARTESIAN_POINT('Ctrl Pts',(-38.7022645869853,2.66878522062258,-2.89774106896403));
#39028=CARTESIAN_POINT('Ctrl Pts',(-38.768422304228,1.7111233091636,-3.77973635247244));
#39029=CARTESIAN_POINT('Ctrl Pts',(-38.8345800214707,0.272978604403351,
-4.14002808624563));
#39030=CARTESIAN_POINT('Ctrl Pts',(-38.9007377387134,-0.987397088610618,
-3.81370749349994));
#39031=CARTESIAN_POINT('Ctrl Pts',(-38.9668954559561,-2.24777278162459,
-3.48738690075425));
#39032=CARTESIAN_POINT('Ctrl Pts',(-39.0330531731989,-3.33037946289226,
-2.47445398148969));
#39033=CARTESIAN_POINT('Ctrl Pts',(-39.0992108904416,-3.73969828807051,
-1.23853727064504));
#39034=CARTESIAN_POINT('Ctrl Pts',(-39.120419419616,-3.87091578781602,-0.842332916691583));
#39035=CARTESIAN_POINT('Ctrl Pts',(-39.1416279487905,-3.9329404947859,-0.423212849728327));
#39036=CARTESIAN_POINT('Ctrl Pts',(-39.162836477965,-3.92975286260395,-0.00317618749887255));
#39037=CARTESIAN_POINT('Ctrl Pts',(-39.3461635220348,-3.93009648465997,
-0.00327554246926138));
#39038=CARTESIAN_POINT('Ctrl Pts',(-39.3256314536679,-3.93329844478136,
-0.409825047550122));
#39039=CARTESIAN_POINT('Ctrl Pts',(-39.305099385301,-3.8752504360904,-0.815482606504164));
#39040=CARTESIAN_POINT('Ctrl Pts',(-39.284567316934,-3.75213744234363,-1.20032558511363));
#39041=CARTESIAN_POINT('Ctrl Pts',(-39.2184095996913,-3.3554470318288,-2.44035325824738));
#39042=CARTESIAN_POINT('Ctrl Pts',(-39.1522518824486,-2.28322924458223,
-3.46427669580993));
#39043=CARTESIAN_POINT('Ctrl Pts',(-39.0860941652059,-1.02624783443413,
-3.80343690349066));
#39044=CARTESIAN_POINT('Ctrl Pts',(-39.0199364479632,0.230733575713977,
-4.1425971111714));
#39045=CARTESIAN_POINT('Ctrl Pts',(-38.9537787307205,1.67247860876359,-3.79699408897032));
#39046=CARTESIAN_POINT('Ctrl Pts',(-38.8876210134778,2.63908755693015,-2.92481345787587));
#39047=CARTESIAN_POINT('Ctrl Pts',(-38.821463296235,3.60569650509673,-2.05263282678141));
#39048=CARTESIAN_POINT('Ctrl Pts',(-38.7553055789924,4.09716936838019,-0.653874586793549));
#39049=CARTESIAN_POINT('Ctrl Pts',(-38.6891478617496,3.88855458361905,0.631236997276519));
#39050=CARTESIAN_POINT('Ctrl Pts',(-38.6229901445069,3.67993979885791,1.91634858134655));
#39051=CARTESIAN_POINT('Ctrl Pts',(-38.5568324272642,2.77123736605219,3.08781350949882));
#39052=CARTESIAN_POINT('Ctrl Pts',(-38.4906747100215,1.57836858621257,3.60944171619002));
#39053=CARTESIAN_POINT('Ctrl Pts',(-38.4245169927788,0.385499806372948,
4.13106992288121));
#39054=CARTESIAN_POINT('Ctrl Pts',(-38.3583592755361,-1.09153532050054,
4.00286140811134));
#39055=CARTESIAN_POINT('Ctrl Pts',(-38.2922015582934,-2.17668449232393,
3.28349836567523));
#39056=CARTESIAN_POINT('Ctrl Pts',(-38.2268555462072,-3.24851970449009,
2.57296136372699));
#39057=CARTESIAN_POINT('Ctrl Pts',(-38.161509534121,-3.93802625789471,1.28568688300243));
#39058=CARTESIAN_POINT('Ctrl Pts',(-38.0961635220349,-3.93942817610916,
-0.000298174263498583));
#39059=CARTESIAN_POINT('Origin',(-27.25,0.,0.));
#39060=CARTESIAN_POINT('',(-36.662836477965,-3.93134770437533,0.00351664141719457));
#39061=CARTESIAN_POINT('',(-36.8461635220348,-3.93096795489117,0.00346177198455457));
#39062=CARTESIAN_POINT('',(-27.25,-3.933,-4.81653586104654E-16));
#39063=CARTESIAN_POINT('Ctrl Pts',(-36.662836477965,-3.93134770437533,0.00351664141719457));
#39064=CARTESIAN_POINT('Ctrl Pts',(-36.6810686752113,-3.93447342139821,
0.36423620257401));
#39065=CARTESIAN_POINT('Ctrl Pts',(-36.6993008724577,-3.88890920393724,
0.724180603369993));
#39066=CARTESIAN_POINT('Ctrl Pts',(-36.717533069704,-3.79150170657231,1.06950112932788));
#39067=CARTESIAN_POINT('Ctrl Pts',(-36.7836907869467,-3.43804690455791,
2.32253812787313));
#39068=CARTESIAN_POINT('Ctrl Pts',(-36.8498485041894,-2.40197766182226,
3.38302426616653));
#39069=CARTESIAN_POINT('Ctrl Pts',(-36.9160062214321,-1.15751221727247,
3.76556547193636));
#39070=CARTESIAN_POINT('Ctrl Pts',(-36.9821639386749,0.0869532272773088,
4.1481066777062));
#39071=CARTESIAN_POINT('Ctrl Pts',(-37.0483216559175,1.53981487364122,3.85270295095248));
#39072=CARTESIAN_POINT('Ctrl Pts',(-37.1144793731602,2.53608483983638,3.01456324228343));
#39073=CARTESIAN_POINT('Ctrl Pts',(-37.180637090403,3.53235480603154,2.17642353361439));
#39074=CARTESIAN_POINT('Ctrl Pts',(-37.2467948076457,4.07203309205794,0.795547843030021));
#39075=CARTESIAN_POINT('Ctrl Pts',(-37.3129525248884,3.90810407789765,-0.49602456884117));
#39076=CARTESIAN_POINT('Ctrl Pts',(-37.3791102421311,3.74417506373737,-1.78759698071236));
#39077=CARTESIAN_POINT('Ctrl Pts',(-37.4452679593738,2.87663874939039,-2.98986611387037));
#39078=CARTESIAN_POINT('Ctrl Pts',(-37.5114256766165,1.70257433208425,-3.55254254025229));
#39079=CARTESIAN_POINT('Ctrl Pts',(-37.5775833938592,0.528509914778081,
-4.11521896663422));
#39080=CARTESIAN_POINT('Ctrl Pts',(-37.643741111102,-0.952082605487279,
-4.03830268624002));
#39081=CARTESIAN_POINT('Ctrl Pts',(-37.7098988283447,-2.06152267558061,
-3.35699897447725));
#39082=CARTESIAN_POINT('Ctrl Pts',(-37.7760565455874,-3.17096274567392,
-2.6756952627145));
#39083=CARTESIAN_POINT('Ctrl Pts',(-37.8422142628301,-3.90925036559522,
-1.39000411958323));
#39084=CARTESIAN_POINT('Ctrl Pts',(-37.9083719800728,-3.93846463152386,
-0.0883979796712423));
#39085=CARTESIAN_POINT('Ctrl Pts',(-37.9098601460368,-3.93912178352415,
-0.0591193703603289));
#39086=CARTESIAN_POINT('Ctrl Pts',(-37.9113483120009,-3.93942015168138,
-0.0298327082243094));
#39087=CARTESIAN_POINT('Ctrl Pts',(-37.912836477965,-3.93936327777038,-0.000544856984334152));
#39088=CARTESIAN_POINT('Ctrl Pts',(-38.0961635220349,-3.93942817610916,
-0.000298174263498583));
#39089=CARTESIAN_POINT('Ctrl Pts',(-38.0953518168783,-3.93944559024367,
-0.0162722279033564));
#39090=CARTESIAN_POINT('Ctrl Pts',(-38.0945401117218,-3.93935683166498,
-0.032246082588608));
#39091=CARTESIAN_POINT('Ctrl Pts',(-38.0937284065652,-3.93916131431453,
-0.0482186304571659));
#39092=CARTESIAN_POINT('Ctrl Pts',(-38.0275706893225,-3.92322574770849,
-1.35005501405111));
#39093=CARTESIAN_POINT('Ctrl Pts',(-37.9614129720798,-3.19809139772313,
-2.64321021113658));
#39094=CARTESIAN_POINT('Ctrl Pts',(-37.8952552548371,-2.09565879787217,
-3.33579542229681));
#39095=CARTESIAN_POINT('Ctrl Pts',(-37.8290975375944,-0.993226198021244,
-4.02838063345702));
#39096=CARTESIAN_POINT('Ctrl Pts',(-37.7629398203517,0.486504651695298,
-4.12039585869199));
#39097=CARTESIAN_POINT('Ctrl Pts',(-37.696782103109,1.66624759252964,-3.56972489933111));
#39098=CARTESIAN_POINT('Ctrl Pts',(-37.6306243858663,2.84599053336401,-3.01905393997023));
#39099=CARTESIAN_POINT('Ctrl Pts',(-37.5644666686236,3.72574556531621,-1.8256967960135));
#39100=CARTESIAN_POINT('Ctrl Pts',(-37.4983089513809,3.90284087388428,-0.535863797670248));
#39101=CARTESIAN_POINT('Ctrl Pts',(-37.4321512341382,4.07993618245235,0.753969200673001));
#39102=CARTESIAN_POINT('Ctrl Pts',(-37.3659935168954,3.55437176763629,2.14027805340274));
#39103=CARTESIAN_POINT('Ctrl Pts',(-37.2998357996527,2.56670320327809,2.98853669256333));
#39104=CARTESIAN_POINT('Ctrl Pts',(-37.23367808241,1.5790346389199,3.83679533172392));
#39105=CARTESIAN_POINT('Ctrl Pts',(-37.1675203651673,0.129261925019584,
4.14700375731534));
#39106=CARTESIAN_POINT('Ctrl Pts',(-37.1013626479246,-1.1190408886942,3.77717677451637));
#39107=CARTESIAN_POINT('Ctrl Pts',(-37.0352049306819,-2.36734370240797,
3.4073497917174));
#39108=CARTESIAN_POINT('Ctrl Pts',(-36.9690472134392,-3.41417661593523,
2.35748740052801));
#39109=CARTESIAN_POINT('Ctrl Pts',(-36.9028894961965,-3.78039476114712,
1.10812108833231));
#39110=CARTESIAN_POINT('Ctrl Pts',(-36.8839808381426,-3.88506423841353,
0.751037419700503));
#39111=CARTESIAN_POINT('Ctrl Pts',(-36.8650721800887,-3.93413538382226,
0.377656594845544));
#39112=CARTESIAN_POINT('Ctrl Pts',(-36.8461635220348,-3.93096795489117,
0.00346177198455457));
#39113=CARTESIAN_POINT('Origin',(-27.25,0.,0.));
#39114=CARTESIAN_POINT('',(-35.412836477965,-3.92712485552383,-0.0015385046896832));
#39115=CARTESIAN_POINT('',(-35.5961635220348,-3.92729240225598,-0.00173544043971706));
#39116=CARTESIAN_POINT('',(-27.25,-3.933,-4.81653586104654E-16));
#39117=CARTESIAN_POINT('Ctrl Pts',(-35.412836477965,-3.92712485552383,-0.0015385046896832));
#39118=CARTESIAN_POINT('Ctrl Pts',(-35.4507890384217,-3.92447549046237,
0.751378600752031));
#39119=CARTESIAN_POINT('Ctrl Pts',(-35.4887415988785,-3.71620164740591,
1.50565253191416));
#39120=CARTESIAN_POINT('Ctrl Pts',(-35.5266941593352,-3.3117103233741,2.13351648473401));
#39121=CARTESIAN_POINT('Ctrl Pts',(-35.5928518765779,-2.60661368903953,
3.22798930442411));
#39122=CARTESIAN_POINT('Ctrl Pts',(-35.6590095938206,-1.30528330217824,
3.93834805145753));
#39123=CARTESIAN_POINT('Ctrl Pts',(-35.7251673110634,-0.00334982031690134,
3.93945511908414));
#39124=CARTESIAN_POINT('Ctrl Pts',(-35.7913250283061,1.29858366154446,3.94056218671074));
#39125=CARTESIAN_POINT('Ctrl Pts',(-35.8574827455488,2.60112023840593,3.23241757493054));
#39126=CARTESIAN_POINT('Ctrl Pts',(-35.9236404627915,3.30807716869666,2.13914546081425));
#39127=CARTESIAN_POINT('Ctrl Pts',(-35.9897981800342,4.01503409898737,1.045873346698));
#39128=CARTESIAN_POINT('Ctrl Pts',(-36.0559558972769,4.12641138270738,-0.432526269754304));
#39129=CARTESIAN_POINT('Ctrl Pts',(-36.1221136145196,3.59123063234998,-1.61937654726919));
#39130=CARTESIAN_POINT('Ctrl Pts',(-36.1882713317623,3.05604988199257,-2.8062268247841));
#39131=CARTESIAN_POINT('Ctrl Pts',(-36.254429049005,1.87431109755773,-3.70152776336159));
#39132=CARTESIAN_POINT('Ctrl Pts',(-36.3205867662477,0.586906781291004,
-3.89549204679576));
#39133=CARTESIAN_POINT('Ctrl Pts',(-36.3867444834904,-0.700497534975741,
-4.08945633022993));
#39134=CARTESIAN_POINT('Ctrl Pts',(-36.4529022007332,-2.09356738307438,
-3.58208395852077));
#39135=CARTESIAN_POINT('Ctrl Pts',(-36.5190599179759,-2.95468212647712,
-2.60560384326762));
#39136=CARTESIAN_POINT('Ctrl Pts',(-36.5669854379723,-3.57848496572447,
-1.89822881220443));
#39137=CARTESIAN_POINT('Ctrl Pts',(-36.6149109579686,-3.92313138180822,
-0.944678044485885));
#39138=CARTESIAN_POINT('Ctrl Pts',(-36.662836477965,-3.93134770437533,0.00351664141719457));
#39139=CARTESIAN_POINT('Ctrl Pts',(-36.8461635220348,-3.93096795489117,
0.00346177198455457));
#39140=CARTESIAN_POINT('Ctrl Pts',(-36.798914462846,-3.92305316598257,-0.931578318282404));
#39141=CARTESIAN_POINT('Ctrl Pts',(-36.7516654036572,-3.58895920163905,
-1.87170103574137));
#39142=CARTESIAN_POINT('Ctrl Pts',(-36.7044163444683,-2.98110706244138,
-2.57532863510223));
#39143=CARTESIAN_POINT('Ctrl Pts',(-36.6382586272256,-2.12999784162727,
-3.56054181313891));
#39144=CARTESIAN_POINT('Ctrl Pts',(-36.5721009099829,-0.742176023102554,
-4.08209793601023));
#39145=CARTESIAN_POINT('Ctrl Pts',(-36.5059431927402,0.547139827084099,
-3.9012760612566));
#39146=CARTESIAN_POINT('Ctrl Pts',(-36.4397854754975,1.83645567727075,-3.72045418650296));
#39147=CARTESIAN_POINT('Ctrl Pts',(-36.3736277582548,3.02726555911932,-2.83725431412436));
#39148=CARTESIAN_POINT('Ctrl Pts',(-36.3074700410121,3.57452504726655,-1.65592499316225));
#39149=CARTESIAN_POINT('Ctrl Pts',(-36.2413123237694,4.12178453541378,-0.474595672200148));
#39150=CARTESIAN_POINT('Ctrl Pts',(-36.1751546065266,4.02549362985964,1.0048630973455));
#39151=CARTESIAN_POINT('Ctrl Pts',(-36.1089968892839,3.32972554672827,2.10528969027555));
#39152=CARTESIAN_POINT('Ctrl Pts',(-36.0428391720412,2.6339574635969,3.20571628320559));
#39153=CARTESIAN_POINT('Ctrl Pts',(-35.9766814547985,1.33871220288834,3.92711069952008));
#39154=CARTESIAN_POINT('Ctrl Pts',(-35.9105237375558,0.0368352049943507,
3.93928420708489));
#39155=CARTESIAN_POINT('Ctrl Pts',(-35.8443660203131,-1.26504179289966,
3.95145771464969));
#39156=CARTESIAN_POINT('Ctrl Pts',(-35.7782083030704,-2.57355052797908,
3.25441031346478));
#39157=CARTESIAN_POINT('Ctrl Pts',(-35.7120505858277,-3.28977474798118,
2.16718688720211));
#39158=CARTESIAN_POINT('Ctrl Pts',(-35.6734215645634,-3.70797298361485,
1.53236484976624));
#39159=CARTESIAN_POINT('Ctrl Pts',(-35.6347925432991,-3.92424311660023,
0.764519742442217));
#39160=CARTESIAN_POINT('Ctrl Pts',(-35.5961635220348,-3.92729240225598,
-0.00173544043971706));
#39161=CARTESIAN_POINT('Origin',(-27.25,0.,0.));
#39162=CARTESIAN_POINT('',(-34.162836477965,-3.93697895265161,-0.00271025535696023));
#39163=CARTESIAN_POINT('',(-34.3461635220348,-3.93731358771045,-0.00254698605159045));
#39164=CARTESIAN_POINT('',(-27.25,-3.933,-4.81653586104654E-16));
#39165=CARTESIAN_POINT('Ctrl Pts',(-34.162836477965,-3.93697895265161,-0.00271025535696023));
#39166=CARTESIAN_POINT('Ctrl Pts',(-34.2205094016322,-3.92802881866666,
1.13413956848541));
#39167=CARTESIAN_POINT('Ctrl Pts',(-34.2781823252993,-3.40846140270135,
2.27812248496691));
#39168=CARTESIAN_POINT('Ctrl Pts',(-34.3358552489664,-2.54120789046762,
3.01024588929201));
#39169=CARTESIAN_POINT('Ctrl Pts',(-34.4020129662092,-1.54636474758752,
3.85007869280399));
#39170=CARTESIAN_POINT('Ctrl Pts',(-34.4681706834519,-0.0940075806728428,
4.14795280206281));
#39171=CARTESIAN_POINT('Ctrl Pts',(-34.5343284006946,1.15110663308848,3.76752855010205));
#39172=CARTESIAN_POINT('Ctrl Pts',(-34.6004861179373,2.39622084684978,3.38710429814129));
#39173=CARTESIAN_POINT('Ctrl Pts',(-34.66664383518,3.43409210745772,2.32838168496089));
#39174=CARTESIAN_POINT('Ctrl Pts',(-34.7328015524227,3.78967737616872,1.07594760147943));
#39175=CARTESIAN_POINT('Ctrl Pts',(-34.7989592696654,4.14526264487973,-0.176486482002049));
#39176=CARTESIAN_POINT('Ctrl Pts',(-34.8651169869081,3.81856192169385,-1.62263203578459));
#39177=CARTESIAN_POINT('Ctrl Pts',(-34.9312747041508,2.95910907482034,-2.60057519404655));
#39178=CARTESIAN_POINT('Ctrl Pts',(-34.9974324213936,2.09965622794684,-3.5785183523085));
#39179=CARTESIAN_POINT('Ctrl Pts',(-35.0635901386363,0.707451257385696,
-4.08825911504983));
#39180=CARTESIAN_POINT('Ctrl Pts',(-35.129747855879,-0.58028106258638,-3.89648453673025));
#39181=CARTESIAN_POINT('Ctrl Pts',(-35.1959055731217,-1.86801338255846,
-3.70470995841067));
#39182=CARTESIAN_POINT('Ctrl Pts',(-35.2620632903644,-3.05127305194149,
-2.81142003903016));
#39183=CARTESIAN_POINT('Ctrl Pts',(-35.3282210076071,-3.58847144572904,
-1.62548163316652));
#39184=CARTESIAN_POINT('Ctrl Pts',(-35.3564261643931,-3.81749635096215,
-1.11987805326706));
#39185=CARTESIAN_POINT('Ctrl Pts',(-35.384631321179,-3.92909378083592,-0.561082966255875));
#39186=CARTESIAN_POINT('Ctrl Pts',(-35.412836477965,-3.92712485552383,-0.0015385046896832));
#39187=CARTESIAN_POINT('Ctrl Pts',(-35.5961635220348,-3.92729240225598,
-0.00173544043971706));
#39188=CARTESIAN_POINT('Ctrl Pts',(-35.5686348260564,-3.92946545388974,
-0.547801721206673));
#39189=CARTESIAN_POINT('Ctrl Pts',(-35.541106130078,-3.82335220054039,-1.09306054320404));
#39190=CARTESIAN_POINT('Ctrl Pts',(-35.5135774340996,-3.60486554173621,
-1.58879241013994));
#39191=CARTESIAN_POINT('Ctrl Pts',(-35.4474197168568,-3.07979241056439,
-2.78014882987897));
#39192=CARTESIAN_POINT('Ctrl Pts',(-35.3812619996142,-1.90570644329594,
-3.68546221801658));
#39193=CARTESIAN_POINT('Ctrl Pts',(-35.3151042823714,-0.619997378722377,
-3.89036246985969));
#39194=CARTESIAN_POINT('Ctrl Pts',(-35.2489465651287,0.665711685851162,
-4.09526272170278));
#39195=CARTESIAN_POINT('Ctrl Pts',(-35.182788847886,2.06304384772982,-3.59974983725139));
#39196=CARTESIAN_POINT('Ctrl Pts',(-35.1166311306433,2.93242757091785,-2.63062453380109));
#39197=CARTESIAN_POINT('Ctrl Pts',(-35.0504734134006,3.80181129410592,-1.66149923035074));
#39198=CARTESIAN_POINT('Ctrl Pts',(-34.9843156961579,4.14324657860332,-0.218761507901483));
#39199=CARTESIAN_POINT('Ctrl Pts',(-34.9181579789152,3.80045541456625,1.03723456286872));
#39200=CARTESIAN_POINT('Ctrl Pts',(-34.8520002616725,3.45766425052919,2.29323063363886));
#39201=CARTESIAN_POINT('Ctrl Pts',(-34.7858425444298,2.4306466379577,3.36248505272994));
#39202=CARTESIAN_POINT('Ctrl Pts',(-34.7196848271871,1.18947780297691,3.7555904266494));
#39203=CARTESIAN_POINT('Ctrl Pts',(-34.6535271099443,-0.0516910320038823,
4.14869580056886));
#39204=CARTESIAN_POINT('Ctrl Pts',(-34.5873693927016,-1.50701108939393,
3.86565212931673));
#39205=CARTESIAN_POINT('Ctrl Pts',(-34.5212116754589,-2.51036925030615,
3.0360110545966));
#39206=CARTESIAN_POINT('Ctrl Pts',(-34.4628622909842,-3.39530503008972,
2.30428922285262));
#39207=CARTESIAN_POINT('Ctrl Pts',(-34.4045129065095,-3.92866955648817,
1.14738125101164));
#39208=CARTESIAN_POINT('Ctrl Pts',(-34.3461635220348,-3.93731358771045,
-0.00254698605159045));
#39209=CARTESIAN_POINT('Origin',(-27.25,0.,0.));
#39210=CARTESIAN_POINT('',(-32.912836477965,-3.93548209384035,0.00323960751162838));
#39211=CARTESIAN_POINT('',(-33.0961635220348,-3.93508971521476,0.00333466163741802));
#39212=CARTESIAN_POINT('',(-27.25,-3.933,-4.81653586104654E-16));
#39213=CARTESIAN_POINT('Ctrl Pts',(-32.912836477965,-3.93548209384035,0.00323960751162838));
#39214=CARTESIAN_POINT('Ctrl Pts',(-32.9240720475999,-3.93745101947663,
0.224934599518961));
#39215=CARTESIAN_POINT('Ctrl Pts',(-32.9353076172347,-3.92033161139393,
0.446325502292901));
#39216=CARTESIAN_POINT('Ctrl Pts',(-32.9465431868695,-3.88304868935319,
0.664267064279747));
#39217=CARTESIAN_POINT('Ctrl Pts',(-33.0127009041123,-3.66351794062248,
1.94755902917007));
#39218=CARTESIAN_POINT('Ctrl Pts',(-33.078858621355,-2.74489081412106,3.11125767044752));
#39219=CARTESIAN_POINT('Ctrl Pts',(-33.1450163385977,-1.54763123269596,
3.62272762213202));
#39220=CARTESIAN_POINT('Ctrl Pts',(-33.2111740558404,-0.35037165127085,
4.13419757381653));
#39221=CARTESIAN_POINT('Ctrl Pts',(-33.2773317730831,1.12552038507792,3.99343883590807));
#39222=CARTESIAN_POINT('Ctrl Pts',(-33.3434894903258,2.20451577711144,3.26487795254908));
#39223=CARTESIAN_POINT('Ctrl Pts',(-33.4096472075685,3.28351116914494,2.53631706919011));
#39224=CARTESIAN_POINT('Ctrl Pts',(-33.4758049248112,3.96560991686318,1.21995404038064));
#39225=CARTESIAN_POINT('Ctrl Pts',(-33.5419626420539,3.93860927013953,-0.0816999005217973));
#39226=CARTESIAN_POINT('Ctrl Pts',(-33.6081203592966,3.91160862341588,-1.38335384142423));
#39227=CARTESIAN_POINT('Ctrl Pts',(-33.6742780765394,3.1755085822503,-2.67029869441967));
#39228=CARTESIAN_POINT('Ctrl Pts',(-33.7404357937821,2.06722877593257,-3.35348819060552));
#39229=CARTESIAN_POINT('Ctrl Pts',(-33.8065935110248,0.958948969614857,
-4.03667768679136));
#39230=CARTESIAN_POINT('Ctrl Pts',(-33.8727512282675,-0.521510601854994,
-4.11611182616768));
#39231=CARTESIAN_POINT('Ctrl Pts',(-33.9389089455102,-1.69653023720889,
-3.55543288655689));
#39232=CARTESIAN_POINT('Ctrl Pts',(-34.0050666627529,-2.87154987256281,
-2.99475394694609));
#39233=CARTESIAN_POINT('Ctrl Pts',(-34.0712243799956,-3.74112957180075,
-1.79396192834816));
#39234=CARTESIAN_POINT('Ctrl Pts',(-34.1373820972383,-3.90725486199698,
-0.502670170166627));
#39235=CARTESIAN_POINT('Ctrl Pts',(-34.1458668908139,-3.92856059704561,
-0.337060707346072));
#39236=CARTESIAN_POINT('Ctrl Pts',(-34.1543516843894,-3.93829568907673,
-0.169962675875666));
#39237=CARTESIAN_POINT('Ctrl Pts',(-34.162836477965,-3.93697895265161,-0.00271025535696023));
#39238=CARTESIAN_POINT('Ctrl Pts',(-34.3461635220348,-3.93731358771045,
-0.00254698605159045));
#39239=CARTESIAN_POINT('Ctrl Pts',(-34.3383551892668,-3.93847033465557,
-0.156430740185009));
#39240=CARTESIAN_POINT('Ctrl Pts',(-34.3305468564988,-3.93023045225109,
-0.310189502096346));
#39241=CARTESIAN_POINT('Ctrl Pts',(-34.3227385237308,-3.91217899916458,
-0.462787613286053));
#39242=CARTESIAN_POINT('Ctrl Pts',(-34.2565808064881,-3.75923432267645,
-1.75570672826033));
#39243=CARTESIAN_POINT('Ctrl Pts',(-34.1904230892453,-2.90194870526589,
-2.96530648002073));
#39244=CARTESIAN_POINT('Ctrl Pts',(-34.1242653720026,-1.73270950769983,
-3.5379421502396));
#39245=CARTESIAN_POINT('Ctrl Pts',(-34.0581076547599,-0.563470310133773,
-4.11057782045846));
#39246=CARTESIAN_POINT('Ctrl Pts',(-33.9919499375172,0.917722467587795,
-4.04624940913581));
#39247=CARTESIAN_POINT('Ctrl Pts',(-33.9257922202745,2.03291352908098,-3.37440061044845));
#39248=CARTESIAN_POINT('Ctrl Pts',(-33.8596345030318,3.14810459057416,-2.7025518117611));
#39249=CARTESIAN_POINT('Ctrl Pts',(-33.7934767857891,3.89729393583897,-1.42318262570904));
#39250=CARTESIAN_POINT('Ctrl Pts',(-33.7273190685464,3.93757084301924,-0.121871870093793));
#39251=CARTESIAN_POINT('Ctrl Pts',(-33.6611613513037,3.9778477501995,1.17943888552147));
#39252=CARTESIAN_POINT('Ctrl Pts',(-33.595003634061,3.30921221929523,2.50269121069989));
#39253=CARTESIAN_POINT('Ctrl Pts',(-33.5288459168182,2.23770476464396,3.24222057898674));
#39254=CARTESIAN_POINT('Ctrl Pts',(-33.4626881995756,1.16619730999271,3.98174994727357));
#39255=CARTESIAN_POINT('Ctrl Pts',(-33.3965304823328,-0.308182068405588,
4.1375563586688));
#39256=CARTESIAN_POINT('Ctrl Pts',(-33.3303727650901,-1.5105966285017,3.63832581312816));
#39257=CARTESIAN_POINT('Ctrl Pts',(-33.2642150478474,-2.71301118859784,
3.13909526758751));
#39258=CARTESIAN_POINT('Ctrl Pts',(-33.1980573306047,-3.64346093039182,
1.98482776511106));
#39259=CARTESIAN_POINT('Ctrl Pts',(-33.131899613362,-3.87607061336398,0.703841954370138));
#39260=CARTESIAN_POINT('Ctrl Pts',(-33.1199875829196,-3.91795315919898,
0.47319400263047));
#39261=CARTESIAN_POINT('Ctrl Pts',(-33.1080755524772,-3.93721185766393,
0.238437866459535));
#39262=CARTESIAN_POINT('Ctrl Pts',(-33.0961635220348,-3.93508971521476,
0.00333466163741802));
#39263=CARTESIAN_POINT('Origin',(-27.25,0.,0.));
#39264=CARTESIAN_POINT('',(-31.662836477965,-3.92666097892795,0.000687624971145162));
#39265=CARTESIAN_POINT('',(-31.8461635220349,-3.92660201554812,0.000470019213647162));
#39266=CARTESIAN_POINT('',(-27.25,-3.933,-4.81653586104654E-16));
#39267=CARTESIAN_POINT('Ctrl Pts',(-31.662836477965,-3.92666097892795,0.000687624971145162));
#39268=CARTESIAN_POINT('Ctrl Pts',(-31.6937924108103,-3.92762034739937,
0.614984183704047));
#39269=CARTESIAN_POINT('Ctrl Pts',(-31.7247483436555,-3.79213432965767,
1.22888030589506));
#39270=CARTESIAN_POINT('Ctrl Pts',(-31.7557042765008,-3.51797781227477,
1.77289310701935));
#39271=CARTESIAN_POINT('Ctrl Pts',(-31.8218619937435,-2.93206203813433,
2.93553437688886));
#39272=CARTESIAN_POINT('Ctrl Pts',(-31.8880197109862,-1.71277652222822,
3.77898749115005));
#39273=CARTESIAN_POINT('Ctrl Pts',(-31.9541774282289,-0.418199244510039,
3.91719635051213));
#39274=CARTESIAN_POINT('Ctrl Pts',(-32.0203351454716,0.87637803320812,4.05540520987422));
#39275=CARTESIAN_POINT('Ctrl Pts',(-32.0864928627143,2.24624707273834,3.48836981433722));
#39276=CARTESIAN_POINT('Ctrl Pts',(-32.152650579957,3.06440645693195,2.47562737973389));
#39277=CARTESIAN_POINT('Ctrl Pts',(-32.2188082971997,3.88256584112558,1.46288494513054));
#39278=CARTESIAN_POINT('Ctrl Pts',(-32.2849660144424,4.14901556998256,0.0044354714608888));
#39279=CARTESIAN_POINT('Ctrl Pts',(-32.3511237316851,3.74179919892956,-1.23217556032592));
#39280=CARTESIAN_POINT('Ctrl Pts',(-32.4172814489278,3.33458282787656,-2.46878659211269));
#39281=CARTESIAN_POINT('Ctrl Pts',(-32.4834391661706,2.25370035691356,-3.48355918201663));
#39282=CARTESIAN_POINT('Ctrl Pts',(-32.5495968834133,0.993881443772989,
-3.81202276125131));
#39283=CARTESIAN_POINT('Ctrl Pts',(-32.615754600656,-0.265937469367559,
-4.14048634048598));
#39284=CARTESIAN_POINT('Ctrl Pts',(-32.6819123178987,-1.7046928246857,-3.78264090905147));
#39285=CARTESIAN_POINT('Ctrl Pts',(-32.7480700351414,-2.66385331686478,
-2.90227554908263));
#39286=CARTESIAN_POINT('Ctrl Pts',(-32.8029921827493,-3.46011951719077,
-2.17142269828554));
#39287=CARTESIAN_POINT('Ctrl Pts',(-32.8579143303571,-3.92585751511942,
-1.08045845771079));
#39288=CARTESIAN_POINT('Ctrl Pts',(-32.912836477965,-3.93548209384035,0.00323960751162838));
#39289=CARTESIAN_POINT('Ctrl Pts',(-33.0961635220348,-3.93508971521476,
0.00333466163741802));
#39290=CARTESIAN_POINT('Ctrl Pts',(-33.0419178352345,-3.92542578132876,
-1.06729178414136));
#39291=CARTESIAN_POINT('Ctrl Pts',(-32.9876721484342,-3.4723741720033,-2.14511560644448));
#39292=CARTESIAN_POINT('Ctrl Pts',(-32.9334264616339,-2.69331962574125,
-2.87495152830659));
#39293=CARTESIAN_POINT('Ctrl Pts',(-32.8672687443912,-1.74318933099608,
-3.76505508123703));
#39294=CARTESIAN_POINT('Ctrl Pts',(-32.8011110271485,-0.308159117355434,
-4.13755806809258));
#39295=CARTESIAN_POINT('Ctrl Pts',(-32.7349533099057,0.954944740814757,
-3.82196251139459));
#39296=CARTESIAN_POINT('Ctrl Pts',(-32.668795592663,2.21804859898495,-3.50636695469659));
#39297=CARTESIAN_POINT('Ctrl Pts',(-32.6026378754203,3.30922610168469,-2.50267285444504));
#39298=CARTESIAN_POINT('Ctrl Pts',(-32.5364801581776,3.72903546228296,-1.27028005477198));
#39299=CARTESIAN_POINT('Ctrl Pts',(-32.4703224409349,4.14884482288123,-0.0378872550989129));
#39300=CARTESIAN_POINT('Ctrl Pts',(-32.4041647236922,3.89728604137803,1.42320424399567));
#39301=CARTESIAN_POINT('Ctrl Pts',(-32.3380070064495,3.08949984140983,2.44423968269154));
#39302=CARTESIAN_POINT('Ctrl Pts',(-32.2718492892068,2.28171364144163,3.46527512138741));
#39303=CARTESIAN_POINT('Ctrl Pts',(-32.205691571964,0.917700023008417,4.04625449968457));
#39304=CARTESIAN_POINT('Ctrl Pts',(-32.1395338547213,-0.378219675799687,
3.92125831505059));
#39305=CARTESIAN_POINT('Ctrl Pts',(-32.0733761374786,-1.67413937460779,
3.7962621304166));
#39306=CARTESIAN_POINT('Ctrl Pts',(-32.0072184202359,-2.90196515379079,
2.96529038285145));
#39307=CARTESIAN_POINT('Ctrl Pts',(-31.9410607029932,-3.49971007785051,
1.80868633751321));
#39308=CARTESIAN_POINT('Ctrl Pts',(-31.9094283093405,-3.78551351137053,
1.2556721769985));
#39309=CARTESIAN_POINT('Ctrl Pts',(-31.8777959156877,-3.92727155150004,
0.628213868479639));
#39310=CARTESIAN_POINT('Ctrl Pts',(-31.8461635220349,-3.92660201554812,
0.000470019213647162));
#39311=CARTESIAN_POINT('Origin',(-27.25,0.,0.));
#39312=CARTESIAN_POINT('',(-30.412836477965,-3.93295883055164,-0.00359432436683793));
#39313=CARTESIAN_POINT('',(-30.5961635220349,-3.93336445157121,-0.00357663055094762));
#39314=CARTESIAN_POINT('',(-27.25,-3.933,-4.81653586104654E-16));
#39315=CARTESIAN_POINT('Ctrl Pts',(-30.412836477965,-3.93295883055164,-0.00359432436683793));
#39316=CARTESIAN_POINT('Ctrl Pts',(-30.4635127740207,-3.923765255997,0.997977755989756));
#39317=CARTESIAN_POINT('Ctrl Pts',(-30.5141890700763,-3.5341466447474,2.00591009962987));
#39318=CARTESIAN_POINT('Ctrl Pts',(-30.564865366132,-2.84408915743405,2.72588971184463));
#39319=CARTESIAN_POINT('Ctrl Pts',(-30.6310230833747,-1.94322165763196,
3.66582043513792));
#39320=CARTESIAN_POINT('Ctrl Pts',(-30.6971808006174,-0.530309991741809,
4.11498738588874));
#39321=CARTESIAN_POINT('Ctrl Pts',(-30.7633385178601,0.74794342470998,3.86780279874859));
#39322=CARTESIAN_POINT('Ctrl Pts',(-30.8294962351028,2.02619684116181,3.62061821160844));
#39323=CARTESIAN_POINT('Ctrl Pts',(-30.8956539523455,3.16979200817529,2.67708208657726));
#39324=CARTESIAN_POINT('Ctrl Pts',(-30.9618116695882,3.65529510129681,1.46905941983634));
#39325=CARTESIAN_POINT('Ctrl Pts',(-31.027969386831,4.14079819441831,0.26103675309547));
#39326=CARTESIAN_POINT('Ctrl Pts',(-31.0941271040737,3.96820921364796,-1.21147245535508));
#39327=CARTESIAN_POINT('Ctrl Pts',(-31.1602848213164,3.21652369243056,-2.27448745712242));
#39328=CARTESIAN_POINT('Ctrl Pts',(-31.2264425385591,2.46483817121316,-3.33750245888977));
#39329=CARTESIAN_POINT('Ctrl Pts',(-31.2926002558018,1.13405610954868,-3.99102325397385));
#39330=CARTESIAN_POINT('Ctrl Pts',(-31.3587579730445,-0.166711537791714,
-3.93592747897385));
#39331=CARTESIAN_POINT('Ctrl Pts',(-31.4249156902872,-1.46747918513211,
-3.88083170397386));
#39332=CARTESIAN_POINT('Ctrl Pts',(-31.4910734075299,-2.73823241814845,
-3.1171193588898));
#39333=CARTESIAN_POINT('Ctrl Pts',(-31.5572311247726,-3.39733601846922,
-1.99434847360887));
#39334=CARTESIAN_POINT('Ctrl Pts',(-31.5924329091701,-3.74803770227979,
-1.39693459237704));
#39335=CARTESIAN_POINT('Ctrl Pts',(-31.6276346935675,-3.92557002546655,
-0.697864575820828));
#39336=CARTESIAN_POINT('Ctrl Pts',(-31.662836477965,-3.92666097892795,0.000687624971145162));
#39337=CARTESIAN_POINT('Ctrl Pts',(-31.8461635220349,-3.92660201554812,
0.000470019213647162));
#39338=CARTESIAN_POINT('Ctrl Pts',(-31.8116381984449,-3.92587124741059,
-0.684683932946426));
#39339=CARTESIAN_POINT('Ctrl Pts',(-31.777112874855,-3.75547031300368,-1.37017804217001));
#39340=CARTESIAN_POINT('Ctrl Pts',(-31.7425875512651,-3.41750273201399,
-1.95958974614389));
#39341=CARTESIAN_POINT('Ctrl Pts',(-31.6764298340224,-2.76988639318133,
-3.08902544135141));
#39342=CARTESIAN_POINT('Ctrl Pts',(-31.6102721167797,-1.50698964657953,
-3.86566048865513));
#39343=CARTESIAN_POINT('Ctrl Pts',(-31.544114399537,-0.206851725873873,
-3.93402202078463));
#39344=CARTESIAN_POINT('Ctrl Pts',(-31.4779566822943,1.09328619483184,-4.00238355291413));
#39345=CARTESIAN_POINT('Ctrl Pts',(-31.4117989650515,2.4306652896414,-3.36247156986939));
#39346=CARTESIAN_POINT('Ctrl Pts',(-31.3456412478088,3.19315508220056,-2.30717955901402));
#39347=CARTESIAN_POINT('Ctrl Pts',(-31.2794835305661,3.95564487475968,-1.2518875481587));
#39348=CARTESIAN_POINT('Ctrl Pts',(-31.2133258133234,4.1432453650684,0.218784490507221));
#39349=CARTESIAN_POINT('Ctrl Pts',(-31.1471680960807,3.67009011634552,1.43169669777447));
#39350=CARTESIAN_POINT('Ctrl Pts',(-31.081010378838,3.19693486762262,2.64460890504174));
#39351=CARTESIAN_POINT('Ctrl Pts',(-31.0148526615953,2.06302387986814,3.59976128091032));
#39352=CARTESIAN_POINT('Ctrl Pts',(-30.9486949443526,0.787358441326591,
3.85997196639913));
#39353=CARTESIAN_POINT('Ctrl Pts',(-30.8825372271099,-0.488306997214944,
4.12018265188792));
#39354=CARTESIAN_POINT('Ctrl Pts',(-30.8163795098671,-1.90572688654355,
3.68545164699692));
#39355=CARTESIAN_POINT('Ctrl Pts',(-30.7502217926244,-2.81613535659577,
2.75475925442616));
#39356=CARTESIAN_POINT('Ctrl Pts',(-30.6988690357612,-3.52281005392954,
2.03233982790978));
#39357=CARTESIAN_POINT('Ctrl Pts',(-30.647516278898,-3.92400372217985,1.01109716125747));
#39358=CARTESIAN_POINT('Ctrl Pts',(-30.5961635220349,-3.93336445157121,
-0.00357663055094761));
#39359=CARTESIAN_POINT('Origin',(-27.25,0.,0.));
#39360=CARTESIAN_POINT('',(-29.162836477965,-3.93875478927679,0.00150291653159836));
#39361=CARTESIAN_POINT('',(-29.3461635220348,-3.93853086460256,0.00172150567391906));
#39362=CARTESIAN_POINT('',(-27.25,-3.933,-4.81653586104654E-16));
#39363=CARTESIAN_POINT('Ctrl Pts',(-29.162836477965,-3.93875478927679,0.00150291653159836));
#39364=CARTESIAN_POINT('Ctrl Pts',(-29.1670754199883,-3.93916252700776,
0.0849618398189939));
#39365=CARTESIAN_POINT('Ctrl Pts',(-29.1713143620117,-3.93673966426794,
0.168396650786846));
#39366=CARTESIAN_POINT('Ctrl Pts',(-29.1755533040351,-3.93141099567647,
0.251645464192195));
#39367=CARTESIAN_POINT('Ctrl Pts',(-29.2417110212778,-3.84824577472923,
1.55092047850407));
#39368=CARTESIAN_POINT('Ctrl Pts',(-29.3078687385205,-3.05727712238509,
2.80488974298552));
#39369=CARTESIAN_POINT('Ctrl Pts',(-29.3740264557632,-1.92053852624666,
3.4396002130737));
#39370=CARTESIAN_POINT('Ctrl Pts',(-29.4401841730059,-0.783799930108228,
4.07431068316188));
#39371=CARTESIAN_POINT('Ctrl Pts',(-29.5063418902486,0.698708609824502,
4.08976235885678));
#39372=CARTESIAN_POINT('Ctrl Pts',(-29.5724996074913,1.84842956093395,3.4788828688014));
#39373=CARTESIAN_POINT('Ctrl Pts',(-29.638657324734,2.99815051204339,2.86800337874602));
#39374=CARTESIAN_POINT('Ctrl Pts',(-29.7048150419767,3.81508387432956,1.63079272294036));
#39375=CARTESIAN_POINT('Ctrl Pts',(-29.7709727592195,3.92531187821855,0.333533379574904));
#39376=CARTESIAN_POINT('Ctrl Pts',(-29.8371304764622,4.03553988210755,-0.963725963790554));
#39377=CARTESIAN_POINT('Ctrl Pts',(-29.9032881937049,3.43906252759938,-2.32103399471581));
#39378=CARTESIAN_POINT('Ctrl Pts',(-29.9694459109476,2.40889288074741,-3.11713858300506));
#39379=CARTESIAN_POINT('Ctrl Pts',(-30.0356036281903,1.3787232338954,-3.91324317129434));
#39380=CARTESIAN_POINT('Ctrl Pts',(-30.101761345433,-0.085138705300437,
-4.14814431694758));
#39381=CARTESIAN_POINT('Ctrl Pts',(-30.1679190626757,-1.31267012159303,
-3.71432564652741));
#39382=CARTESIAN_POINT('Ctrl Pts',(-30.2340767799184,-2.54020153788559,
-3.28050697610725));
#39383=CARTESIAN_POINT('Ctrl Pts',(-30.3002344971611,-3.53140243127492,
-2.17796848961372));
#39384=CARTESIAN_POINT('Ctrl Pts',(-30.3663922144039,-3.83259121111256,
-0.911351998449073));
#39385=CARTESIAN_POINT('Ctrl Pts',(-30.3818736355909,-3.90307173178068,
-0.614953872887294));
#39386=CARTESIAN_POINT('Ctrl Pts',(-30.397355056778,-3.93576743360619,-0.309570893928312));
#39387=CARTESIAN_POINT('Ctrl Pts',(-30.412836477965,-3.93295883055164,-0.00359432436683793));
#39388=CARTESIAN_POINT('Ctrl Pts',(-30.5961635220349,-3.93336445157121,
-0.00357663055094761));
#39389=CARTESIAN_POINT('Ctrl Pts',(-30.5813585616553,-3.93606314266839,
-0.29610630575176));
#39390=CARTESIAN_POINT('Ctrl Pts',(-30.5665536012758,-3.90619407193774,
-0.588089999412536));
#39391=CARTESIAN_POINT('Ctrl Pts',(-30.5517486408963,-3.84168803968927,
-0.872209781087009));
#39392=CARTESIAN_POINT('Ctrl Pts',(-30.4855909236536,-3.55343520195466,
-2.14183264377887));
#39393=CARTESIAN_POINT('Ctrl Pts',(-30.4194332064109,-2.57353247570956,
-3.25442458891207));
#39394=CARTESIAN_POINT('Ctrl Pts',(-30.3532754891682,-1.3504901785784,-3.70074224637148));
#39395=CARTESIAN_POINT('Ctrl Pts',(-30.2871177719255,-0.127447881447261,
-4.14705990383089));
#39396=CARTESIAN_POINT('Ctrl Pts',(-30.2209600546827,1.33873398656992,-3.92710327361655));
#39397=CARTESIAN_POINT('Ctrl Pts',(-30.15480233744,2.37697075787629,-3.14154848963316));
#39398=CARTESIAN_POINT('Ctrl Pts',(-30.0886446201973,3.41520752918271,-2.35599370564973));
#39399=CARTESIAN_POINT('Ctrl Pts',(-30.0224869029546,4.02549920377824,-1.00484076789717));
#39400=CARTESIAN_POINT('Ctrl Pts',(-29.9563291857119,3.92850977668485,0.293475435099665));
#39401=CARTESIAN_POINT('Ctrl Pts',(-29.8901714684692,3.83152034959146,1.5917916380965));
#39402=CARTESIAN_POINT('Ctrl Pts',(-29.8240137512265,3.02724982080915,2.83727110633764));
#39403=CARTESIAN_POINT('Ctrl Pts',(-29.7578560339838,1.88382006678415,3.45984665158685));
#39404=CARTESIAN_POINT('Ctrl Pts',(-29.6916983167411,0.74039031275917,4.08242219683605));
#39405=CARTESIAN_POINT('Ctrl Pts',(-29.6255405994984,-0.74219866650845,
4.08209381909339));
#39406=CARTESIAN_POINT('Ctrl Pts',(-29.5593828822557,-1.88535252059195,
3.459011819814));
#39407=CARTESIAN_POINT('Ctrl Pts',(-29.493225165013,-3.02850637467544,2.83592982053462));
#39408=CARTESIAN_POINT('Ctrl Pts',(-29.4270674477702,-3.8322251035748,1.59009419971851));
#39409=CARTESIAN_POINT('Ctrl Pts',(-29.3609097305275,-3.92863939462808,
0.29173515984833));
#39410=CARTESIAN_POINT('Ctrl Pts',(-29.3559943276966,-3.93580280804277,
0.195269351079819));
#39411=CARTESIAN_POINT('Ctrl Pts',(-29.3510789248657,-3.93906173797095,
0.0985136009347571));
#39412=CARTESIAN_POINT('Ctrl Pts',(-29.3461635220348,-3.93853086460256,
0.00172150567391906));
#39413=CARTESIAN_POINT('Origin',(-27.25,0.,0.));
#39414=CARTESIAN_POINT('',(-27.912836477965,-3.92849944027351,0.00265245323384067));
#39415=CARTESIAN_POINT('',(-28.0961635220349,-3.92823136251108,0.00249701373361682));
#39416=CARTESIAN_POINT('',(-27.25,-3.933,-4.81653586104654E-16));
#39417=CARTESIAN_POINT('Ctrl Pts',(-27.912836477965,-3.92849944027351,0.00265245323384067));
#39418=CARTESIAN_POINT('Ctrl Pts',(-27.9367957831988,-3.93144429728796,
0.477549615694625));
#39419=CARTESIAN_POINT('Ctrl Pts',(-27.9607550884325,-3.85179092258685,
0.95149239765976));
#39420=CARTESIAN_POINT('Ctrl Pts',(-27.9847143936663,-3.68512069940966,
1.39255279517753));
#39421=CARTESIAN_POINT('Ctrl Pts',(-28.050872110909,-3.22490194973579,2.61043239482561));
#39422=CARTESIAN_POINT('Ctrl Pts',(-28.1170298281517,-2.10122138469273,
3.57759955359381));
#39423=CARTESIAN_POINT('Ctrl Pts',(-28.1831875453944,-0.82839773576013,
3.85137313798103));
#39424=CARTESIAN_POINT('Ctrl Pts',(-28.2493452626371,0.444425913172473,
4.12514672236825));
#39425=CARTESIAN_POINT('Ctrl Pts',(-28.3155029798798,1.86639264599462,3.70552673237448));
#39426=CARTESIAN_POINT('Ctrl Pts',(-28.3816606971225,2.78665546135827,2.78457702286299));
#39427=CARTESIAN_POINT('Ctrl Pts',(-28.4478184143653,3.70691827672194,1.86362731335147));
#39428=CARTESIAN_POINT('Ctrl Pts',(-28.513976131608,4.12547717462709,0.441347884322195));
#39429=CARTESIAN_POINT('Ctrl Pts',(-28.5801338488507,3.85075397163164,-0.83127113900189));
#39430=CARTESIAN_POINT('Ctrl Pts',(-28.6462915660934,3.5760307686362,-2.10389016232594));
#39431=CARTESIAN_POINT('Ctrl Pts',(-28.7124492833361,2.60802546474021,-3.22684877994481));
#39432=CARTESIAN_POINT('Ctrl Pts',(-28.7786070005788,1.38980282003078,-3.68615870222768));
#39433=CARTESIAN_POINT('Ctrl Pts',(-28.8447647178215,0.171580175321349,
-4.14546862451055));
#39434=CARTESIAN_POINT('Ctrl Pts',(-28.9109224350642,-1.29685981020152,
-3.94112985145742));
#39435=CARTESIAN_POINT('Ctrl Pts',(-28.9770801523069,-2.34339890818778,
-3.1666700828597));
#39436=CARTESIAN_POINT('Ctrl Pts',(-29.0389989275263,-3.32288281221589,
-2.44183249282753));
#39437=CARTESIAN_POINT('Ctrl Pts',(-29.1009177027456,-3.93279891142486,
-1.21759238663821));
#39438=CARTESIAN_POINT('Ctrl Pts',(-29.162836477965,-3.93875478927679,0.00150291653159836));
#39439=CARTESIAN_POINT('Ctrl Pts',(-29.3461635220348,-3.93853086460256,
0.00172150567391906));
#39440=CARTESIAN_POINT('Ctrl Pts',(-29.284921207623,-3.93191657176457,-1.20423701582998));
#39441=CARTESIAN_POINT('Ctrl Pts',(-29.2236788932112,-3.33699851326665,
-2.41583751049172));
#39442=CARTESIAN_POINT('Ctrl Pts',(-29.1624365787994,-2.3755788853513,-3.14260112899942));
#39443=CARTESIAN_POINT('Ctrl Pts',(-29.0962788615567,-1.33699423181405,
-3.9276959190527));
#39444=CARTESIAN_POINT('Ctrl Pts',(-29.030121144314,0.129284928467726,-4.14700304023501));
#39445=CARTESIAN_POINT('Ctrl Pts',(-28.9639634270713,1.35212939634983,-3.70014364478489));
#39446=CARTESIAN_POINT('Ctrl Pts',(-28.8978057098285,2.57497386423193,-3.25328424933478));
#39447=CARTESIAN_POINT('Ctrl Pts',(-28.8316479925859,3.55438363971437,-2.14025833725233));
#39448=CARTESIAN_POINT('Ctrl Pts',(-28.7654902753432,3.84207403318388,-0.870507909240087));
#39449=CARTESIAN_POINT('Ctrl Pts',(-28.6993325581004,4.1297644266534,0.399242518772191));
#39450=CARTESIAN_POINT('Ctrl Pts',(-28.6331748408577,3.72573543810985,1.82571746271425));
#39451=CARTESIAN_POINT('Ctrl Pts',(-28.567017123615,2.81491478040445,2.75600647233927));
#39452=CARTESIAN_POINT('Ctrl Pts',(-28.5008594063723,1.90409412269907,3.68629548196426));
#39453=CARTESIAN_POINT('Ctrl Pts',(-28.4347016891296,0.486481795831812,
4.12039855727229));
#39454=CARTESIAN_POINT('Ctrl Pts',(-28.3685439718869,-0.789068249736409,
3.85962280459805));
#39455=CARTESIAN_POINT('Ctrl Pts',(-28.3023862546442,-2.0646182953047,3.59884705192379));
#39456=CARTESIAN_POINT('Ctrl Pts',(-28.2362285374015,-3.19810605957393,
2.64319247126727));
#39457=CARTESIAN_POINT('Ctrl Pts',(-28.1700708201588,-3.67072396750674,
1.43007078527147));
#39458=CARTESIAN_POINT('Ctrl Pts',(-28.1454350541175,-3.84671710469501,
0.978329351597568));
#39459=CARTESIAN_POINT('Ctrl Pts',(-28.1207992880762,-3.93106982372138,
0.490885891314328));
#39460=CARTESIAN_POINT('Ctrl Pts',(-28.0961635220349,-3.92823136251108,
0.00249701373361682));
#39461=CARTESIAN_POINT('Origin',(-27.25,0.,0.));
#39462=CARTESIAN_POINT('',(-26.662836477965,-3.92914366735242,-0.00295733212259536));
#39463=CARTESIAN_POINT('',(-26.8461635220349,-3.92946204260484,-0.00307907422078526));
#39464=CARTESIAN_POINT('',(-27.25,-3.933,-4.81653586104654E-16));
#39465=CARTESIAN_POINT('Ctrl Pts',(-26.662836477965,-3.92914366735242,-0.00295733212259536));
#39466=CARTESIAN_POINT('Ctrl Pts',(-26.7065161464092,-3.92309441571187,
0.862460122396525));
#39467=CARTESIAN_POINT('Ctrl Pts',(-26.7501958148533,-3.64146415129019,
1.73145588387443));
#39468=CARTESIAN_POINT('Ctrl Pts',(-26.7938754832975,-3.11534036258412,
2.411218007943));
#39469=CARTESIAN_POINT('Ctrl Pts',(-26.8600332005402,-2.31846735306552,
3.44079336870641));
#39470=CARTESIAN_POINT('Ctrl Pts',(-26.9261909177829,-0.960714648945873,
4.03625782584134));
#39471=CARTESIAN_POINT('Ctrl Pts',(-26.9923486350256,0.336462088646539,
3.92506192555964));
#39472=CARTESIAN_POINT('Ctrl Pts',(-27.0585063522684,1.63363882623891,3.81386602527794));
#39473=CARTESIAN_POINT('Ctrl Pts',(-27.1246640695111,2.87023959730411,2.99600976757956));
#39474=CARTESIAN_POINT('Ctrl Pts',(-27.1908217867538,3.48026107339907,1.8458333395942));
#39475=CARTESIAN_POINT('Ctrl Pts',(-27.2569795039965,4.09028254949405,0.695656911608815));
#39476=CARTESIAN_POINT('Ctrl Pts',(-27.3231372212392,4.07372473061887,-0.786839686663616));
#39477=CARTESIAN_POINT('Ctrl Pts',(-27.3892949384819,3.43816627984279,-1.92310438841117));
#39478=CARTESIAN_POINT('Ctrl Pts',(-27.4554526557246,2.80260782906669,-3.05936909015876));
#39479=CARTESIAN_POINT('Ctrl Pts',(-27.5216103729673,1.54804874638969,-3.84940189538143));
#39480=CARTESIAN_POINT('Ctrl Pts',(-27.58776809021,0.248712041483546,-3.93159766214645));
#39481=CARTESIAN_POINT('Ctrl Pts',(-27.6539258074527,-1.05062466342256,
-4.01379342891147));
#39482=CARTESIAN_POINT('Ctrl Pts',(-27.7200835246955,-2.39473899055777,
-3.3881521572189));
#39483=CARTESIAN_POINT('Ctrl Pts',(-27.7862412419382,-3.16841768697301,
-2.34103550110863));
#39484=CARTESIAN_POINT('Ctrl Pts',(-27.8284396539471,-3.6619052762455,-1.67313669931251));
#39485=CARTESIAN_POINT('Ctrl Pts',(-27.8706380659561,-3.92331280032755,
-0.83376187213494));
#39486=CARTESIAN_POINT('Ctrl Pts',(-27.912836477965,-3.92849944027351,0.00265245323384067));
#39487=CARTESIAN_POINT('Ctrl Pts',(-28.0961635220349,-3.92823136251108,
0.00249701373361682));
#39488=CARTESIAN_POINT('Ctrl Pts',(-28.0546415708335,-3.92344732422855,
-0.820650076891716));
#39489=CARTESIAN_POINT('Ctrl Pts',(-28.013119619632,-3.67098044429315,-1.64648280202908));
#39490=CARTESIAN_POINT('Ctrl Pts',(-27.9715976684306,-3.19213273732399,
-2.30859383257857));
#39491=CARTESIAN_POINT('Ctrl Pts',(-27.9054399511879,-2.42917554761208,
-3.36354797309789));
#39492=CARTESIAN_POINT('Ctrl Pts',(-27.8392822339452,-1.09151311659189,
-4.00286746280153));
#39493=CARTESIAN_POINT('Ctrl Pts',(-27.7731245167025,0.208594393842709,
-3.93393000387307));
#39494=CARTESIAN_POINT('Ctrl Pts',(-27.7069667994598,1.50870190427727,-3.8649925449446));
#39495=CARTESIAN_POINT('Ctrl Pts',(-27.6408090822171,2.7712544941262,-3.08779813738407));
#39496=CARTESIAN_POINT('Ctrl Pts',(-27.5746513649744,3.4183704533748,-1.95807567269744));
#39497=CARTESIAN_POINT('Ctrl Pts',(-27.5084936477317,4.06548641262342,-0.828353208010779));
#39498=CARTESIAN_POINT('Ctrl Pts',(-27.4423359304889,4.09716574127161,0.653897313802084));
#39499=CARTESIAN_POINT('Ctrl Pts',(-27.3761782132462,3.49890852481402,1.81023645734449));
#39500=CARTESIAN_POINT('Ctrl Pts',(-27.3100204960035,2.90065130835643,2.9665756008869));
#39501=CARTESIAN_POINT('Ctrl Pts',(-27.2438627787608,1.6724575467931,3.79700336615891));
#39502=CARTESIAN_POINT('Ctrl Pts',(-27.1777050615181,0.376482604477266,
3.92142547360541));
#39503=CARTESIAN_POINT('Ctrl Pts',(-27.1115473442754,-0.919492337838605,
4.0458475810519));
#39504=CARTESIAN_POINT('Ctrl Pts',(-27.0453896270327,-2.28324846090694,
3.46426403067282));
#39505=CARTESIAN_POINT('Ctrl Pts',(-26.97923190979,-3.09058228458904,2.44287086001282));
#39506=CARTESIAN_POINT('Ctrl Pts',(-26.9348757805383,-3.6318676391175,1.75806719110156));
#39507=CARTESIAN_POINT('Ctrl Pts',(-26.8905196512866,-3.92303163210045,
0.875561558831162));
#39508=CARTESIAN_POINT('Ctrl Pts',(-26.8461635220349,-3.92946204260484,
-0.00307907422078526));
#39509=CARTESIAN_POINT('Origin',(-27.25,0.,0.));
#39510=CARTESIAN_POINT('',(-25.412836477965,-3.93914704469817,-0.000998409943392953));
#39511=CARTESIAN_POINT('',(-25.5961635220349,-3.93927687571695,-0.00075861444495069));
#39512=CARTESIAN_POINT('',(-27.25,-3.933,-4.81653586104654E-16));
#39513=CARTESIAN_POINT('Ctrl Pts',(-25.412836477965,-3.93914704469817,-0.000998409943392953));
#39514=CARTESIAN_POINT('Ctrl Pts',(-25.4762365096196,-3.93490039704559,
1.24692954761248));
#39515=CARTESIAN_POINT('Ctrl Pts',(-25.5396365412741,-3.29132887644148,
2.49862752120908));
#39516=CARTESIAN_POINT('Ctrl Pts',(-25.6030365729287,-2.2720868718378,3.21821986560842));
#39517=CARTESIAN_POINT('Ctrl Pts',(-25.6691942901714,-1.20851130913384,
3.96911202777905));
#39518=CARTESIAN_POINT('Ctrl Pts',(-25.7353520074142,0.26412626364417,4.14060227385076));
#39519=CARTESIAN_POINT('Ctrl Pts',(-25.8015097246569,1.47178634459257,3.6541979711621));
#39520=CARTESIAN_POINT('Ctrl Pts',(-25.8676674418996,2.67944642554097,3.16779366847344));
#39521=CARTESIAN_POINT('Ctrl Pts',(-25.9338251591423,3.62212901465975,2.02349481702441));
#39522=CARTESIAN_POINT('Ctrl Pts',(-25.999982876385,3.86835978685463,0.745057323982752));
#39523=CARTESIAN_POINT('Ctrl Pts',(-26.0661405936277,4.11459055904951,-0.533380169058908));
#39524=CARTESIAN_POINT('Ctrl Pts',(-26.1322983108704,3.66436951432049,-1.9459563036932));
#39525=CARTESIAN_POINT('Ctrl Pts',(-26.1984560281131,2.723766886339,-2.8461222400764));
#39526=CARTESIAN_POINT('Ctrl Pts',(-26.2646137453558,1.78316425835751,-3.7462881764596));
#39527=CARTESIAN_POINT('Ctrl Pts',(-26.3307714625985,0.352180047123545,
-4.13404391459171));
#39528=CARTESIAN_POINT('Ctrl Pts',(-26.3969291798412,-0.914211364797984,
-3.83191015513785));
#39529=CARTESIAN_POINT('Ctrl Pts',(-26.4630868970839,-2.18060277671955,
-3.52977639568397));
#39530=CARTESIAN_POINT('Ctrl Pts',(-26.5292446143267,-3.28240138932867,
-2.53775313864409));
#39531=CARTESIAN_POINT('Ctrl Pts',(-26.5954023315694,-3.71530403817446,
-1.30989837792818));
#39532=CARTESIAN_POINT('Ctrl Pts',(-26.6178803803679,-3.8623890234389,-0.892716824827767));
#39533=CARTESIAN_POINT('Ctrl Pts',(-26.6403584291665,-3.93225668030363,
-0.448310890578607));
#39534=CARTESIAN_POINT('Ctrl Pts',(-26.662836477965,-3.92914366735242,-0.00295733212259536));
#39535=CARTESIAN_POINT('Ctrl Pts',(-26.8461635220349,-3.92946204260484,
-0.00307907422078526));
#39536=CARTESIAN_POINT('Ctrl Pts',(-26.8243619340439,-3.93262266916976,
-0.434941849379828));
#39537=CARTESIAN_POINT('Ctrl Pts',(-26.8025603460529,-3.86699609002072,
-0.865870900831215));
#39538=CARTESIAN_POINT('Ctrl Pts',(-26.7807587580619,-3.72847238930294,
-1.27193181370741));
#39539=CARTESIAN_POINT('Ctrl Pts',(-26.7146010408191,-3.30811714603892,
-2.50413852582693));
#39540=CARTESIAN_POINT('Ctrl Pts',(-26.6484433235764,-2.216495135215,-3.5073491591251));
#39541=CARTESIAN_POINT('Ctrl Pts',(-26.5822856063337,-0.953251598840578,
-3.82238515665588));
#39542=CARTESIAN_POINT('Ctrl Pts',(-26.516127889091,0.309991937533875,-4.13742115418667));
#39543=CARTESIAN_POINT('Ctrl Pts',(-26.4499701718483,1.7448569994588,-3.76428251595003));
#39544=CARTESIAN_POINT('Ctrl Pts',(-26.3838124546056,2.69459290399842,-2.87375816279602));
#39545=CARTESIAN_POINT('Ctrl Pts',(-26.3176547373629,3.64432880853801,-1.98323380964204));
#39546=CARTESIAN_POINT('Ctrl Pts',(-26.2514970201202,4.10893555569232,-0.575323741570636));
#39547=CARTESIAN_POINT('Ctrl Pts',(-26.1853393028774,3.87575844601461,0.705558902333295));
#39548=CARTESIAN_POINT('Ctrl Pts',(-26.1191815856347,3.64258133633691,1.98644154623723));
#39549=CARTESIAN_POINT('Ctrl Pts',(-26.053023868392,2.71162036982735,3.14029676597366));
#39550=CARTESIAN_POINT('Ctrl Pts',(-25.9868661511493,1.50898477916967,3.63899461840075));
#39551=CARTESIAN_POINT('Ctrl Pts',(-25.9207084339066,0.306349188512026,
4.13769247082782));
#39552=CARTESIAN_POINT('Ctrl Pts',(-25.8545507166639,-1.16796102629378,
3.98123295594543));
#39553=CARTESIAN_POINT('Ctrl Pts',(-25.7883929994212,-2.23914077999871,
3.24122900515563));
#39554=CARTESIAN_POINT('Ctrl Pts',(-25.7243165069591,-3.27662278927113,
2.52450449362568));
#39555=CARTESIAN_POINT('Ctrl Pts',(-25.660240014497,-3.93593917010812,1.26037295231601));
#39556=CARTESIAN_POINT('Ctrl Pts',(-25.5961635220349,-3.93927687571695,
-0.00075861444495069));
#39557=CARTESIAN_POINT('Origin',(-27.25,0.,0.));
#39558=CARTESIAN_POINT('',(-24.162836477965,-3.93208044729297,0.00358197651929196));
#39559=CARTESIAN_POINT('',(-24.3461635220348,-3.93168694540681,0.00355335107693575));
#39560=CARTESIAN_POINT('',(-27.25,-3.933,-4.81653586104654E-16));
#39561=CARTESIAN_POINT('Ctrl Pts',(-24.162836477965,-3.93208044729297,0.00358197651929196));
#39562=CARTESIAN_POINT('Ctrl Pts',(-24.1797991555873,-3.93508766644803,
0.33902540008706));
#39563=CARTESIAN_POINT('Ctrl Pts',(-24.1967618332096,-3.89573838320665,
0.673773865534885));
#39564=CARTESIAN_POINT('Ctrl Pts',(-24.2137245108318,-3.81128013311853,
0.99672544036477));
#39565=CARTESIAN_POINT('Ctrl Pts',(-24.2798822280745,-3.48187665375216,
2.25629892554613));
#39566=CARTESIAN_POINT('Ctrl Pts',(-24.3460399453173,-2.46629786501127,
3.33642394104913));
#39567=CARTESIAN_POINT('Ctrl Pts',(-24.41219766256,-1.2293833401628,3.74271752333842));
#39568=CARTESIAN_POINT('Ctrl Pts',(-24.4783553798027,0.00753118468553859,
4.14901110562767));
#39569=CARTESIAN_POINT('Ctrl Pts',(-24.5445130970454,1.46578144564145,3.8814732547034));
#39570=CARTESIAN_POINT('Ctrl Pts',(-24.6106708142881,2.47791314321192,3.06255845842524));
#39571=CARTESIAN_POINT('Ctrl Pts',(-24.6768285315308,3.49004484078246,2.24364366214702));
#39572=CARTESIAN_POINT('Ctrl Pts',(-24.7429862487735,4.05605797496752,0.873351920514928));
#39573=CARTESIAN_POINT('Ctrl Pts',(-24.8091439660162,3.91688322817713,-0.421121874757202));
#39574=CARTESIAN_POINT('Ctrl Pts',(-24.8753016832589,3.77770848138675,-1.71559567002929));
#39575=CARTESIAN_POINT('Ctrl Pts',(-24.9414594005016,2.93334585362089,-2.93425151894138));
#39576=CARTESIAN_POINT('Ctrl Pts',(-25.0076171177443,1.77026773670627,-3.5192996458033));
#39577=CARTESIAN_POINT('Ctrl Pts',(-25.073774834987,0.607189619791642,-4.10434777266522));
#39578=CARTESIAN_POINT('Ctrl Pts',(-25.1399325522298,-0.874603986271784,
-4.05578817747699));
#39579=CARTESIAN_POINT('Ctrl Pts',(-25.2060902694725,-1.99688278054788,
-3.39584702501831));
#39580=CARTESIAN_POINT('Ctrl Pts',(-25.2722479867152,-3.11916157482398,
-2.73590587255962));
#39581=CARTESIAN_POINT('Ctrl Pts',(-25.3384057039579,-3.88192555731279,
-1.46458316283046));
#39582=CARTESIAN_POINT('Ctrl Pts',(-25.4045634212006,-3.93605077224223,
-0.163774768831114));
#39583=CARTESIAN_POINT('Ctrl Pts',(-25.4073211067887,-3.93830690095081,
-0.109552514639702));
#39584=CARTESIAN_POINT('Ctrl Pts',(-25.4100787923769,-3.93933175941713,
-0.0552790286398185));
#39585=CARTESIAN_POINT('Ctrl Pts',(-25.412836477965,-3.93914704469817,-0.000998409943392953));
#39586=CARTESIAN_POINT('Ctrl Pts',(-25.5961635220349,-3.93927687571695,
-0.00075861444495069));
#39587=CARTESIAN_POINT('Ctrl Pts',(-25.5940822972543,-3.93938528545282,
-0.0417205673778243));
#39588=CARTESIAN_POINT('Ctrl Pts',(-25.5920010724737,-3.93880165671922,
-0.082679355424592));
#39589=CARTESIAN_POINT('Ctrl Pts',(-25.5899198476931,-3.93751647003208,
-0.12361611845337));
#39590=CARTESIAN_POINT('Ctrl Pts',(-25.5237621304504,-3.89666311375636,
-1.42490890457529));
#39591=CARTESIAN_POINT('Ctrl Pts',(-25.4576044132076,-3.14690710860075,
-2.70394609012188));
#39592=CARTESIAN_POINT('Ctrl Pts',(-25.3914466959649,-2.03141854176537,
-3.37530081691799));
#39593=CARTESIAN_POINT('Ctrl Pts',(-25.3252889787222,-0.915929974929986,
-4.0466555437141));
#39594=CARTESIAN_POINT('Ctrl Pts',(-25.2591312614795,0.565291153585176,
-4.11032781175974));
#39595=CARTESIAN_POINT('Ctrl Pts',(-25.1929735442368,1.73427657098226,-3.53717424957513));
#39596=CARTESIAN_POINT('Ctrl Pts',(-25.1268158269941,2.90326198837934,-2.96402068739052));
#39597=CARTESIAN_POINT('Ctrl Pts',(-25.0606581097514,3.76001169465834,-1.75404129497565));
#39598=CARTESIAN_POINT('Ctrl Pts',(-24.9945003925087,3.91238362041176,-0.461054555610493));
#39599=CARTESIAN_POINT('Ctrl Pts',(-24.928342675266,4.06475554616517,0.831932183754663));
#39600=CARTESIAN_POINT('Ctrl Pts',(-24.8621849580232,3.512749691393,2.2079262700701));
#39601=CARTESIAN_POINT('Ctrl Pts',(-24.7960272407805,2.50902411553662,3.03712279701876));
#39602=CARTESIAN_POINT('Ctrl Pts',(-24.7298695235378,1.50529853968021,3.86631932396744));
#39603=CARTESIAN_POINT('Ctrl Pts',(-24.6637118062951,0.0498532427395583,
4.1487182915493));
#39604=CARTESIAN_POINT('Ctrl Pts',(-24.5975540890524,-1.19114133312601,
3.75506314474659));
#39605=CARTESIAN_POINT('Ctrl Pts',(-24.5313963718097,-2.43213590899152,
3.36140799794391));
#39606=CARTESIAN_POINT('Ctrl Pts',(-24.465238654567,-3.45867976378196,2.29169873675672));
#39607=CARTESIAN_POINT('Ctrl Pts',(-24.3990809373243,-3.80091451458247,
1.03555094000812));
#39608=CARTESIAN_POINT('Ctrl Pts',(-24.3814417988945,-3.89216201217545,
0.700633627280088));
#39609=CARTESIAN_POINT('Ctrl Pts',(-24.3638026604647,-3.93476363339442,
0.352462850730819));
#39610=CARTESIAN_POINT('Ctrl Pts',(-24.3461635220348,-3.93168694540681,
0.00355335107693575));
#39611=CARTESIAN_POINT('Origin',(-27.25,0.,0.));
#39612=CARTESIAN_POINT('',(-22.912836477965,-3.92686657274101,-0.00115429526849065));
#39613=CARTESIAN_POINT('',(-23.0961635220349,-3.92699480624753,-0.00136118811112632));
#39614=CARTESIAN_POINT('',(-27.25,-3.933,-4.81653586104654E-16));
#39615=CARTESIAN_POINT('Ctrl Pts',(-22.912836477965,-3.92686657274101,-0.00115429526849065));
#39616=CARTESIAN_POINT('Ctrl Pts',(-22.9495195187977,-3.92495252483706,
0.726697173104542));
#39617=CARTESIAN_POINT('Ctrl Pts',(-22.9862025596304,-3.73121721702526,
1.45549568713423));
#39618=CARTESIAN_POINT('Ctrl Pts',(-23.022885600463,-3.35194483101353,2.06973034630505));
#39619=CARTESIAN_POINT('Ctrl Pts',(-23.0890433177058,-2.66792860165602,
3.17750009438718));
#39620=CARTESIAN_POINT('Ctrl Pts',(-23.1552010349485,-1.38043487888614,
3.91263969955316));
#39621=CARTESIAN_POINT('Ctrl Pts',(-23.2213587521912,-0.0787611542536249,
3.93866913273443));
#39622=CARTESIAN_POINT('Ctrl Pts',(-23.2875164694339,1.22291257037878,3.9646985659157));
#39623=CARTESIAN_POINT('Ctrl Pts',(-23.3536741866766,2.53876629687382,3.28161782711241));
#39624=CARTESIAN_POINT('Ctrl Pts',(-23.4198319039193,3.26652190413782,2.20207913262947));
#39625=CARTESIAN_POINT('Ctrl Pts',(-23.485989621162,3.99427751140188,1.12254043814643));
#39626=CARTESIAN_POINT('Ctrl Pts',(-23.5521473384047,4.13393499943478,-0.353456212016352));
#39627=CARTESIAN_POINT('Ctrl Pts',(-23.6183050556474,3.62157187609663,-1.55033383593352));
#39628=CARTESIAN_POINT('Ctrl Pts',(-23.6844627728902,3.10920875275847,-2.74721145985068));
#39629=CARTESIAN_POINT('Ctrl Pts',(-23.7506204901329,1.94482501804926,-3.66497005752223));
#39630=CARTESIAN_POINT('Ctrl Pts',(-23.8167782073756,0.661369611393123,
-3.88354323958161));
#39631=CARTESIAN_POINT('Ctrl Pts',(-23.8829359246183,-0.622085795262939,
-4.10211642164099));
#39632=CARTESIAN_POINT('Ctrl Pts',(-23.949093641861,-2.02461287386591,-3.62150418808829));
#39633=CARTESIAN_POINT('Ctrl Pts',(-24.0152513591037,-2.90426232817139,
-2.66168709388216));
#39634=CARTESIAN_POINT('Ctrl Pts',(-24.0644463987241,-3.55837180413624,
-1.94796476569749));
#39635=CARTESIAN_POINT('Ctrl Pts',(-24.1136414383446,-3.92335893122251,
-0.969268706628277));
#39636=CARTESIAN_POINT('Ctrl Pts',(-24.162836477965,-3.93208044729297,0.00358197651929196));
#39637=CARTESIAN_POINT('Ctrl Pts',(-24.3461635220348,-3.93168694540681,
0.00355335107693575));
#39638=CARTESIAN_POINT('Ctrl Pts',(-24.2976449432219,-3.92322414382476,
-0.95616433155768));
#39639=CARTESIAN_POINT('Ctrl Pts',(-24.249126364409,-3.56916317924449,-1.9214711297343));
#39640=CARTESIAN_POINT('Ctrl Pts',(-24.2006077855961,-2.93126197236318,
-2.63192327887667));
#39641=CARTESIAN_POINT('Ctrl Pts',(-24.1344500683534,-2.06144903253297,
-3.60066336870251));
#39642=CARTESIAN_POINT('Ctrl Pts',(-24.0682923511107,-0.663897506062122,
-4.0955572160442));
#39643=CARTESIAN_POINT('Ctrl Pts',(-24.002134633868,0.621720665900904,-3.8900874424757));
#39644=CARTESIAN_POINT('Ctrl Pts',(-23.9359769166253,1.90733883786397,-3.68461766890719));
#39645=CARTESIAN_POINT('Ctrl Pts',(-23.8698191993826,3.0810236553192,-2.77878427442845));
#39646=CARTESIAN_POINT('Ctrl Pts',(-23.8036614821399,3.60556898936345,-1.58719537532593));
#39647=CARTESIAN_POINT('Ctrl Pts',(-23.7375037648972,4.1301143234077,-0.39560647622341));
#39648=CARTESIAN_POINT('Ctrl Pts',(-23.6713460476545,4.00552017404096,1.08173792750288));
#39649=CARTESIAN_POINT('Ctrl Pts',(-23.6051883304118,3.28881440740741,2.16864397496335));
#39650=CARTESIAN_POINT('Ctrl Pts',(-23.5390306131691,2.57210864077385,3.25555002242383));
#39651=CARTESIAN_POINT('Ctrl Pts',(-23.4728728959263,1.26329125687349,3.95201771361849));
#39652=CARTESIAN_POINT('Ctrl Pts',(-23.4067151786836,-0.0385802206812267,
3.93926750336755));
#39653=CARTESIAN_POINT('Ctrl Pts',(-23.3405574614409,-1.34045169823594,
3.9265172931166));
#39654=CARTESIAN_POINT('Ctrl Pts',(-23.2743997441982,-2.63537726944501,
3.20454918142005));
#39655=CARTESIAN_POINT('Ctrl Pts',(-23.2082420269555,-3.33065781868451,
2.1038144859638));
#39656=CARTESIAN_POINT('Ctrl Pts',(-23.1708825253153,-3.72328525358264,
1.48222563171916));
#39657=CARTESIAN_POINT('Ctrl Pts',(-23.1335230236751,-3.92469178838456,
0.73985183902043));
#39658=CARTESIAN_POINT('Ctrl Pts',(-23.0961635220349,-3.92699480624753,
-0.00136118811112632));
#39659=CARTESIAN_POINT('Origin',(-27.25,0.,0.));
#39660=CARTESIAN_POINT('',(-21.662836477965,-3.93631159263206,-0.00298228534019229));
#39661=CARTESIAN_POINT('',(-21.8461635220349,-3.93667291872696,-0.00284305540341681));
#39662=CARTESIAN_POINT('',(-27.25,-3.933,-4.81653586104654E-16));
#39663=CARTESIAN_POINT('Ctrl Pts',(-21.662836477965,-3.93631159263206,-0.00298228534019229));
#39664=CARTESIAN_POINT('Ctrl Pts',(-21.7192398820081,-3.92694175997278,
1.1093344945322));
#39665=CARTESIAN_POINT('Ctrl Pts',(-21.7756432860512,-3.43266800109764,
2.22893605216819));
#39666=CARTESIAN_POINT('Ctrl Pts',(-21.8320466900943,-2.59836658334952,
2.96104862423887));
#39667=CARTESIAN_POINT('Ctrl Pts',(-21.898204407337,-1.61978243178991,3.81977155691665));
#39668=CARTESIAN_POINT('Ctrl Pts',(-21.9643621245797,-0.173393518595285,
4.14539317327969));
#39669=CARTESIAN_POINT('Ctrl Pts',(-22.0305198418224,1.07877490261441,3.78887352204631));
#39670=CARTESIAN_POINT('Ctrl Pts',(-22.0966775590651,2.33094332382414,3.43235387081292));
#39671=CARTESIAN_POINT('Ctrl Pts',(-22.1628352763078,3.38889125304889,2.39369295198309));
#39672=CARTESIAN_POINT('Ctrl Pts',(-22.2289929935505,3.76838637920517,1.14829523799207));
#39673=CARTESIAN_POINT('Ctrl Pts',(-22.2951507107932,4.14788150536145,-0.0971024759989268));
#39674=CARTESIAN_POINT('Ctrl Pts',(-22.361308428036,3.84892382844929,-1.54923698515106));
#39675=CARTESIAN_POINT('Ctrl Pts',(-22.4274661452787,3.00834897412506,-2.5434532247429));
#39676=CARTESIAN_POINT('Ctrl Pts',(-22.4936238625214,2.16777411980086,-3.53766946433471));
#39677=CARTESIAN_POINT('Ctrl Pts',(-22.5597815797641,0.785582088064504,
-4.07396743436626));
#39678=CARTESIAN_POINT('Ctrl Pts',(-22.6259392970068,-0.505585359235217,
-3.90687871594465));
#39679=CARTESIAN_POINT('Ctrl Pts',(-22.6920970142495,-1.79675280653497,
-3.73978999752304));
#39680=CARTESIAN_POINT('Ctrl Pts',(-22.7582547314922,-2.99689566939817,
-2.86931459064829));
#39681=CARTESIAN_POINT('Ctrl Pts',(-22.8244124487349,-3.55669773285718,
-1.69387694171179));
#39682=CARTESIAN_POINT('Ctrl Pts',(-22.853887125145,-3.80610151161202,-1.17019435732824));
#39683=CARTESIAN_POINT('Ctrl Pts',(-22.883361801555,-3.92840450256694,-0.585980035389735));
#39684=CARTESIAN_POINT('Ctrl Pts',(-22.912836477965,-3.92686657274101,-0.00115429526849065));
#39685=CARTESIAN_POINT('Ctrl Pts',(-23.0961635220349,-3.92699480624753,
-0.00136118811112632));
#39686=CARTESIAN_POINT('Ctrl Pts',(-23.0673653064324,-3.92877006560706,
-0.572718182331229));
#39687=CARTESIAN_POINT('Ctrl Pts',(-23.0385670908299,-3.81223900635808,
-1.14338545542971));
#39688=CARTESIAN_POINT('Ctrl Pts',(-23.0097688752274,-3.57379115692316,
-1.65750826942529));
#39689=CARTESIAN_POINT('Ctrl Pts',(-22.9436111579847,-3.02600841865232,
-2.83859505014238));
#39690=CARTESIAN_POINT('Ctrl Pts',(-22.877453440742,-1.83480741484064,-3.72126733236049));
#39691=CARTESIAN_POINT('Ctrl Pts',(-22.8112957234993,-0.545411590902302,
-3.90151804981405));
#39692=CARTESIAN_POINT('Ctrl Pts',(-22.7451380062565,0.743984233035964,
-4.0817687672676));
#39693=CARTESIAN_POINT('Ctrl Pts',(-22.6789802890138,2.13157487710084,-3.55959791995668));
#39694=CARTESIAN_POINT('Ctrl Pts',(-22.6128225717711,2.98224758587941,-2.57400781526239));
#39695=CARTESIAN_POINT('Ctrl Pts',(-22.5466648545284,3.83292029465795,-1.58841771056812));
#39696=CARTESIAN_POINT('Ctrl Pts',(-22.4805071372857,4.14667506815019,-0.139408348490439));
#39697=CARTESIAN_POINT('Ctrl Pts',(-22.414349420043,3.77990351610863,1.1097956142574));
#39698=CARTESIAN_POINT('Ctrl Pts',(-22.3481917028003,3.41313196406706,2.35899957700527));
#39699=CARTESIAN_POINT('Ctrl Pts',(-22.2820339855575,2.36583408649171,3.40839814042334));
#39700=CARTESIAN_POINT('Ctrl Pts',(-22.2158762683148,1.11736756975067,3.77767211528275));
#39701=CARTESIAN_POINT('Ctrl Pts',(-22.1497185510721,-0.131098946990363,
4.14694609014217));
#39702=CARTESIAN_POINT('Ctrl Pts',(-22.0835608338294,-1.58073410289704,
3.8360954764429));
#39703=CARTESIAN_POINT('Ctrl Pts',(-22.0174031165867,-2.56802680977533,
2.9873994042964));
#39704=CARTESIAN_POINT('Ctrl Pts',(-21.9603232517361,-3.4198478311971,2.25515743591571));
#39705=CARTESIAN_POINT('Ctrl Pts',(-21.9032433868855,-3.92750233438827,
1.12254470519444));
#39706=CARTESIAN_POINT('Ctrl Pts',(-21.8461635220349,-3.93667291872696,
-0.00284305540341681));
#39707=CARTESIAN_POINT('Origin',(-27.25,0.,0.));
#39708=CARTESIAN_POINT('',(-20.412836477965,-3.93619598941234,0.00302311619237688));
#39709=CARTESIAN_POINT('',(-20.5961635220349,-3.9358195614,0.00314458056749582));
#39710=CARTESIAN_POINT('',(-27.25,-3.933,-4.81653586104654E-16));
#39711=CARTESIAN_POINT('Ctrl Pts',(-20.412836477965,-3.93619598941234,0.00302311619237688));
#39712=CARTESIAN_POINT('Ctrl Pts',(-20.4228025279758,-3.93786691095472,
0.199575999993651));
#39713=CARTESIAN_POINT('Ctrl Pts',(-20.4327685779866,-3.92441667643614,
0.395899437378701));
#39714=CARTESIAN_POINT('Ctrl Pts',(-20.4427346279974,-3.89505305236271,
0.589813170295716));
#39715=CARTESIAN_POINT('Ctrl Pts',(-20.5088923452401,-3.7001282489982,1.87707240519113));
#39716=CARTESIAN_POINT('Ctrl Pts',(-20.5750500624828,-2.8039458261767,3.05814284774776));
#39717=CARTESIAN_POINT('Ctrl Pts',(-20.6412077797255,-1.61669656339455,
3.59243790182692));
#39718=CARTESIAN_POINT('Ctrl Pts',(-20.7073654969682,-0.429447300612364,
4.12673295590609));
#39719=CARTESIAN_POINT('Ctrl Pts',(-20.7735232142109,1.04886880213053,4.01425262150776));
#39720=CARTESIAN_POINT('Ctrl Pts',(-20.8396809314536,2.14161312853879,3.30648016238487));
#39721=CARTESIAN_POINT('Ctrl Pts',(-20.9058386486963,3.23435745494705,2.59870770326197));
#39722=CARTESIAN_POINT('Ctrl Pts',(-20.971996365939,3.94153000502067,1.29564311941459));
#39723=CARTESIAN_POINT('Ctrl Pts',(-21.0381540831818,3.93945152310121,-0.00628917402589305));
#39724=CARTESIAN_POINT('Ctrl Pts',(-21.1043118004245,3.93737304118174,-1.30822146746638));
#39725=CARTESIAN_POINT('Ctrl Pts',(-21.1704695176672,3.22604352726911,-2.60902147049994));
#39726=CARTESIAN_POINT('Ctrl Pts',(-21.2366272349099,2.13104491687146,-3.3133012870626));
#39727=CARTESIAN_POINT('Ctrl Pts',(-21.3027849521526,1.03604630647378,-4.01758110362527));
#39728=CARTESIAN_POINT('Ctrl Pts',(-21.3689426693953,-0.44262140040899,
-4.125340733717));
#39729=CARTESIAN_POINT('Ctrl Pts',(-21.435100386638,-1.62815865509478,-3.58725762253205));
#39730=CARTESIAN_POINT('Ctrl Pts',(-21.5012581038807,-2.81369590978054,
-3.04917451134711));
#39731=CARTESIAN_POINT('Ctrl Pts',(-21.5674158211234,-3.70610271226938,
-1.8652486588855));
#39732=CARTESIAN_POINT('Ctrl Pts',(-21.6335735383661,-3.89691641855152,
-0.57737360815846));
#39733=CARTESIAN_POINT('Ctrl Pts',(-21.6433278515658,-3.92505004727135,
-0.387488933620916));
#39734=CARTESIAN_POINT('Ctrl Pts',(-21.6530821647654,-3.93793199629274,
-0.195344544890875));
#39735=CARTESIAN_POINT('Ctrl Pts',(-21.662836477965,-3.93631159263206,-0.00298228534019229));
#39736=CARTESIAN_POINT('Ctrl Pts',(-21.8461635220349,-3.93667291872696,
-0.00284305540341681));
#39737=CARTESIAN_POINT('Ctrl Pts',(-21.8370856696428,-3.93813138768434,
-0.181822175296321));
#39738=CARTESIAN_POINT('Ctrl Pts',(-21.8280078172507,-3.92698170238435,
-0.360618554012682));
#39739=CARTESIAN_POINT('Ctrl Pts',(-21.8189299648586,-3.90260311466682,
-0.537592620771706));
#39740=CARTESIAN_POINT('Ctrl Pts',(-21.7527722476159,-3.72493645483012,
-1.82734704309961));
#39741=CARTESIAN_POINT('Ctrl Pts',(-21.6866145303732,-2.84465287730681,
-3.02031435716174));
#39742=CARTESIAN_POINT('Ctrl Pts',(-21.6204568131305,-1.66466611667486,
-3.57046266140818));
#39743=CARTESIAN_POINT('Ctrl Pts',(-21.5542990958878,-0.48467935604291,
-4.12061096565462));
#39744=CARTESIAN_POINT('Ctrl Pts',(-21.4881413786451,0.995010587697721,
-4.02794026008539));
#39745=CARTESIAN_POINT('Ctrl Pts',(-21.4219836614023,2.09713627883344,-3.33486676263326));
#39746=CARTESIAN_POINT('Ctrl Pts',(-21.3558259441596,3.19926196996916,-2.64179326518112));
#39747=CARTESIAN_POINT('Ctrl Pts',(-21.2896682269169,3.9238234085,-1.34831697584607));
#39748=CARTESIAN_POINT('Ctrl Pts',(-21.2235105096742,3.93918228765327,-0.046473660864169));
#39749=CARTESIAN_POINT('Ctrl Pts',(-21.1573527924315,3.95454116680654,1.25536965411777));
#39750=CARTESIAN_POINT('Ctrl Pts',(-21.0911950751888,3.26069748658226,2.56557999474652));
#39751=CARTESIAN_POINT('Ctrl Pts',(-21.0250373579461,2.17522975866749,3.2844622685491));
#39752=CARTESIAN_POINT('Ctrl Pts',(-20.9588796407034,1.08976203075273,4.00334454235169));
#39753=CARTESIAN_POINT('Ctrl Pts',(-20.8927219234607,-0.387329744852509,
4.13089874932803));
#39754=CARTESIAN_POINT('Ctrl Pts',(-20.8265642062179,-1.57996733742856,
3.60874217826299));
#39755=CARTESIAN_POINT('Ctrl Pts',(-20.7604064889752,-2.77260493000459,
3.08658560719796));
#39756=CARTESIAN_POINT('Ctrl Pts',(-20.6942487717325,-3.68078833955148,
1.91471825809157));
#39757=CARTESIAN_POINT('Ctrl Pts',(-20.6280910544898,-3.88883382668629,
0.62951438818813));
#39758=CARTESIAN_POINT('Ctrl Pts',(-20.6174485436715,-3.92230122005796,
0.422769103446732));
#39759=CARTESIAN_POINT('Ctrl Pts',(-20.6068060328532,-3.93765059158261,
0.213090920066174));
#39760=CARTESIAN_POINT('Ctrl Pts',(-20.5961635220349,-3.9358195614,0.00314458056749582));
#39761=CARTESIAN_POINT('Origin',(-27.25,0.,0.));
#39762=CARTESIAN_POINT('',(-19.162836477965,-3.92683079790197,0.00108863462069703));
#39763=CARTESIAN_POINT('',(-19.3461635220349,-3.9267306052256,0.000876370530420753));
#39764=CARTESIAN_POINT('',(-27.25,-3.933,-4.81653586104654E-16));
#39765=CARTESIAN_POINT('Ctrl Pts',(-19.162836477965,-3.92683079790197,0.00108863462069703));
#39766=CARTESIAN_POINT('Ctrl Pts',(-19.1925228911862,-3.92829091087402,
0.590128976753198));
#39767=CARTESIAN_POINT('Ctrl Pts',(-19.2222093044074,-3.80414942562565,
1.17858470241226));
#39768=CARTESIAN_POINT('Ctrl Pts',(-19.2518957176286,-3.55127120570492,
1.70522452483698));
#39769=CARTESIAN_POINT('Ctrl Pts',(-19.3180534348713,-2.98771892858378,
2.87886878428782));
#39770=CARTESIAN_POINT('Ctrl Pts',(-19.384211152114,-1.78480283323472,3.74550780533721));
#39771=CARTESIAN_POINT('Ctrl Pts',(-19.4503688693567,-0.493108468151834,
3.90847308999452));
#39772=CARTESIAN_POINT('Ctrl Pts',(-19.5165265865994,0.798585896931094,
4.07143837465183));
#39773=CARTESIAN_POINT('Ctrl Pts',(-19.5826843038421,2.17905853174786,3.53072992291702));
#39774=CARTESIAN_POINT('Ctrl Pts',(-19.6488420210848,3.01645465793078,2.53383487094602));
#39775=CARTESIAN_POINT('Ctrl Pts',(-19.7149997383276,3.85385078411367,1.53693981897505));
#39776=CARTESIAN_POINT('Ctrl Pts',(-19.7811574555703,4.14817040166277,0.0838581667679125));
#39777=CARTESIAN_POINT('Ctrl Pts',(-19.847315172813,3.76470076653265,-1.16032150503335));
#39778=CARTESIAN_POINT('Ctrl Pts',(-19.9134728900557,3.38123113140253,-2.40450117683462));
#39779=CARTESIAN_POINT('Ctrl Pts',(-19.9796306072984,2.31997224359321,-3.43977886823002));
#39780=CARTESIAN_POINT('Ctrl Pts',(-20.0457883245411,1.06667186980089,-3.79229864050154));
#39781=CARTESIAN_POINT('Ctrl Pts',(-20.1119460417838,-0.186628503991429,
-4.14481841277306));
#39782=CARTESIAN_POINT('Ctrl Pts',(-20.1781037590265,-1.63197036376675,
-3.81458026592071));
#39783=CARTESIAN_POINT('Ctrl Pts',(-20.2442614762692,-2.60780770170069,
-2.95273717887741));
#39784=CARTESIAN_POINT('Ctrl Pts',(-20.3004531435012,-3.43664414363103,
-2.2207228051708));
#39785=CARTESIAN_POINT('Ctrl Pts',(-20.3566448107331,-3.9267748178169,-1.10520273337645));
#39786=CARTESIAN_POINT('Ctrl Pts',(-20.412836477965,-3.93619598941234,0.00302311619237688));
#39787=CARTESIAN_POINT('Ctrl Pts',(-20.5961635220349,-3.9358195614,0.00314458056749582));
#39788=CARTESIAN_POINT('Ctrl Pts',(-20.5406483156105,-3.92626824213971,
-1.09201187022606));
#39789=CARTESIAN_POINT('Ctrl Pts',(-20.4851331091861,-3.44923046847552,
-2.19446496955116));
#39790=CARTESIAN_POINT('Ctrl Pts',(-20.4296179027617,-2.63779166770679,
-2.9259822306863));
#39791=CARTESIAN_POINT('Ctrl Pts',(-20.363460185519,-1.67079645686973,-3.79773458895681));
#39792=CARTESIAN_POINT('Ctrl Pts',(-20.2973024682763,-0.228898470472945,
-4.14269891479728));
#39793=CARTESIAN_POINT('Ctrl Pts',(-20.2311447510336,1.02793257557226,-3.80298192430529));
#39794=CARTESIAN_POINT('Ctrl Pts',(-20.1649870337908,2.28476362161743,-3.46326493381331));
#39795=CARTESIAN_POINT('Ctrl Pts',(-20.0988293165481,3.35652772731096,-2.43886662698886));
#39796=CARTESIAN_POINT('Ctrl Pts',(-20.0326715993054,3.75266879296217,-1.19866335008759));
#39797=CARTESIAN_POINT('Ctrl Pts',(-19.9665138820627,4.14880985861339,0.0415399268137066));
#39798=CARTESIAN_POINT('Ctrl Pts',(-19.90035616482,3.86932788422227,1.49754817379188));
#39799=CARTESIAN_POINT('Ctrl Pts',(-19.8341984475773,3.04214429070861,2.50293328137695));
#39800=CARTESIAN_POINT('Ctrl Pts',(-19.7680407303346,2.214960697195,3.50831838896196));
#39801=CARTESIAN_POINT('Ctrl Pts',(-19.7018830130919,0.840075484558995,
4.06308035715393));
#39802=CARTESIAN_POINT('Ctrl Pts',(-19.6357252958492,-0.453213982368851,
3.9132996285361));
#39803=CARTESIAN_POINT('Ctrl Pts',(-19.5695675786065,-1.74650344929677,
3.76351889991825));
#39804=CARTESIAN_POINT('Ctrl Pts',(-19.5034098613638,-2.9581971705165,2.90919547449042));
#39805=CARTESIAN_POINT('Ctrl Pts',(-19.437252144121,-3.53369199898883,1.74136089102682));
#39806=CARTESIAN_POINT('Ctrl Pts',(-19.4068892700923,-3.79781352115349,
1.2053869212177));
#39807=CARTESIAN_POINT('Ctrl Pts',(-19.3765263960636,-3.92793108062113,
0.603377411256794));
#39808=CARTESIAN_POINT('Ctrl Pts',(-19.3461635220349,-3.9267306052256,0.000876370530420753));
#39809=CARTESIAN_POINT('Origin',(-27.25,0.,0.));
#39810=CARTESIAN_POINT('',(-17.912836477965,-3.93220475577819,-0.00358799939168875));
#39811=CARTESIAN_POINT('',(-18.0961635220349,-3.93260484470905,-0.00359775545859465));
#39812=CARTESIAN_POINT('',(-27.25,-3.933,-4.81653586104654E-16));
#39813=CARTESIAN_POINT('Ctrl Pts',(-17.912836477965,-3.93220475577819,-0.00358799939168875));
#39814=CARTESIAN_POINT('Ctrl Pts',(-17.9622432543966,-3.92340751667497,
0.973371178801284));
#39815=CARTESIAN_POINT('Ctrl Pts',(-18.0116500308282,-3.55495908794336,
1.95625352284316));
#39816=CARTESIAN_POINT('Ctrl Pts',(-18.0610568072598,-2.89574899554892,
2.67094657590745));
#39817=CARTESIAN_POINT('Ctrl Pts',(-18.1272145245025,-2.01303941508155,
3.62795013564035));
#39818=CARTESIAN_POINT('Ctrl Pts',(-18.1933722417452,-0.608984933822139,
4.10408177595699));
#39819=CARTESIAN_POINT('Ctrl Pts',(-18.2595299589879,0.673766046010135,
3.88141174984286));
#39820=CARTESIAN_POINT('Ctrl Pts',(-18.3256876762306,1.95651702584241,3.65874172372872));
#39821=CARTESIAN_POINT('Ctrl Pts',(-18.3918453934734,3.11796450424755,2.7372700311838));
#39822=CARTESIAN_POINT('Ctrl Pts',(-18.4580031107161,3.62650349280015,1.53876257859445));
#39823=CARTESIAN_POINT('Ctrl Pts',(-18.5241608279588,4.13504248135275,0.340255126005093));
#39824=CARTESIAN_POINT('Ctrl Pts',(-18.5903185452015,3.99067298005282,-1.1352880866287));
#39825=CARTESIAN_POINT('Ctrl Pts',(-18.6564762624442,3.2594742120202,-2.21249761982914));
#39826=CARTESIAN_POINT('Ctrl Pts',(-18.7226339796869,2.52827544398759,-3.28970715302959));
#39827=CARTESIAN_POINT('Ctrl Pts',(-18.7887916969296,1.2102474092223,-3.96858300679668));
#39828=CARTESIAN_POINT('Ctrl Pts',(-18.8549494141723,-0.0913365706719286,
-3.93839757863934));
#39829=CARTESIAN_POINT('Ctrl Pts',(-18.921107131415,-1.39292055056615,-3.908212150482));
#39830=CARTESIAN_POINT('Ctrl Pts',(-18.9872648486577,-2.67806047558931,
-3.16896544040023));
#39831=CARTESIAN_POINT('Ctrl Pts',(-19.0534225659004,-3.35853620865428,
-2.05901733643319));
#39832=CARTESIAN_POINT('Ctrl Pts',(-19.089893869922,-3.73366761243046,-1.44712719821412));
#39833=CARTESIAN_POINT('Ctrl Pts',(-19.1263651739435,-3.92503697310701,
-0.722578089237031));
#39834=CARTESIAN_POINT('Ctrl Pts',(-19.162836477965,-3.92683079790197,0.00108863462069703));
#39835=CARTESIAN_POINT('Ctrl Pts',(-19.3461635220349,-3.9267306052256,0.000876370530420753));
#39836=CARTESIAN_POINT('Ctrl Pts',(-19.3103686788209,-3.92531536276454,
-0.709413118819952));
#39837=CARTESIAN_POINT('Ctrl Pts',(-19.2745738356069,-3.74139311099748,
-1.42038574213652));
#39838=CARTESIAN_POINT('Ctrl Pts',(-19.2387789923929,-3.37936460400123,
-2.0246510241864));
#39839=CARTESIAN_POINT('Ctrl Pts',(-19.1726212751502,-2.7102464448163,-3.1414826144367));
#39840=CARTESIAN_POINT('Ctrl Pts',(-19.1064635579075,-1.43271419072146,
-3.89380005343788));
#39841=CARTESIAN_POINT('Ctrl Pts',(-19.0403058406648,-0.131505879190206,
-3.9372608626117));
#39842=CARTESIAN_POINT('Ctrl Pts',(-18.9741481234221,1.16970243234101,-3.98072167178552));
#39843=CARTESIAN_POINT('Ctrl Pts',(-18.9079904061794,2.4945868013086,-3.31532585113203));
#39844=CARTESIAN_POINT('Ctrl Pts',(-18.8418326889366,3.23673570009262,-2.24563107038117));
#39845=CARTESIAN_POINT('Ctrl Pts',(-18.7756749716939,3.97888459887663,-1.17593628963034));
#39846=CARTESIAN_POINT('Ctrl Pts',(-18.7095172544512,4.13829802747708,0.2980574512179));
#39847=CARTESIAN_POINT('Ctrl Pts',(-18.6433595372085,3.64201102153556,1.50168991989987));
#39848=CARTESIAN_POINT('Ctrl Pts',(-18.5772018199658,3.145724015594,2.70532238858192));
#39849=CARTESIAN_POINT('Ctrl Pts',(-18.5110441027231,1.99373657511054,3.63859358509767));
#39850=CARTESIAN_POINT('Ctrl Pts',(-18.4448863854804,0.71332374381352,3.8743368636487));
#39851=CARTESIAN_POINT('Ctrl Pts',(-18.3787286682377,-0.567089087483427,
4.11008014219972));
#39852=CARTESIAN_POINT('Ctrl Pts',(-18.312570950995,-1.97592730959393,3.64829550278594));
#39853=CARTESIAN_POINT('Ctrl Pts',(-18.2464132337523,-2.86835295895642,
2.70034594068266));
#39854=CARTESIAN_POINT('Ctrl Pts',(-18.1963299965131,-3.54394406726701,
1.98272168174144));
#39855=CARTESIAN_POINT('Ctrl Pts',(-18.146246759274,-3.92358365927177,0.986480569459381));
#39856=CARTESIAN_POINT('Ctrl Pts',(-18.0961635220349,-3.93260484470905,
-0.00359775545859465));
#39857=CARTESIAN_POINT('Origin',(-27.25,0.,0.));
#39858=CARTESIAN_POINT('',(-16.662836477965,-3.93909976961691,0.00107240331368951));
#39859=CARTESIAN_POINT('',(-16.8461635220349,-3.93892856332975,0.00130481274881613));
#39860=CARTESIAN_POINT('',(-27.25,-3.933,-4.81653586104654E-16));
#39861=CARTESIAN_POINT('Ctrl Pts',(-16.662836477965,-3.93909976961691,0.00107240331368951));
#39862=CARTESIAN_POINT('Ctrl Pts',(-16.6658059003643,-3.9393119090298,0.0595225963558853));
#39863=CARTESIAN_POINT('Ctrl Pts',(-16.6687753227636,-3.93812355350836,
0.117963973516891));
#39864=CARTESIAN_POINT('Ctrl Pts',(-16.6717447451629,-3.93550779063421,
0.176341391714401));
#39865=CARTESIAN_POINT('Ctrl Pts',(-16.7379024624056,-3.87722948686605,
1.47697033807084));
#39866=CARTESIAN_POINT('Ctrl Pts',(-16.8040601796483,-3.11041017286938,
2.74585113031923));
#39867=CARTESIAN_POINT('Ctrl Pts',(-16.870217896891,-1.98602996623102,3.4022055831191));
#39868=CARTESIAN_POINT('Ctrl Pts',(-16.9363756141337,-0.861649759592656,
4.05856003591897));
#39869=CARTESIAN_POINT('Ctrl Pts',(-17.0025333313764,0.620291339687363,
4.10238814927032));
#39870=CARTESIAN_POINT('Ctrl Pts',(-17.0686910486192,1.78149552169719,3.51362940031347));
#39871=CARTESIAN_POINT('Ctrl Pts',(-17.1348487658619,2.94269970370699,2.92487065135663));
#39872=CARTESIAN_POINT('Ctrl Pts',(-17.2010064831046,3.78316696844663,1.70352504009155));
#39873=CARTESIAN_POINT('Ctrl Pts',(-17.2671642003473,3.91820786688699,0.408613470702097));
#39874=CARTESIAN_POINT('Ctrl Pts',(-17.33332191759,4.05324876532736,-0.886298098687392));
#39875=CARTESIAN_POINT('Ctrl Pts',(-17.3994796348327,3.48286329746849,-2.25477562620133));
#39876=CARTESIAN_POINT('Ctrl Pts',(-17.4656373520754,2.46812203746625,-3.0704546022939));
#39877=CARTESIAN_POINT('Ctrl Pts',(-17.5317950693181,1.45338077746402,-3.88613357838647));
#39878=CARTESIAN_POINT('Ctrl Pts',(-17.5979527865608,-0.00571627468155991,
-4.14901400305765));
#39879=CARTESIAN_POINT('Ctrl Pts',(-17.6641105038035,-1.241327235511,-3.73877313445908));
#39880=CARTESIAN_POINT('Ctrl Pts',(-17.7302682210463,-2.47693819634043,
-3.32853226586051));
#39881=CARTESIAN_POINT('Ctrl Pts',(-17.796425938289,-3.48906306585369,-2.24517010399219));
#39882=CARTESIAN_POINT('Ctrl Pts',(-17.8625836555317,-3.81444316077267,
-0.98455128348345));
#39883=CARTESIAN_POINT('Ctrl Pts',(-17.8793345963428,-3.89682845062647,
-0.665366279408071));
#39884=CARTESIAN_POINT('Ctrl Pts',(-17.8960855371539,-3.9351873837123,-0.334817570530705));
#39885=CARTESIAN_POINT('Ctrl Pts',(-17.912836477965,-3.93220475577819,-0.00358799939168875));
#39886=CARTESIAN_POINT('Ctrl Pts',(-18.0961635220349,-3.93260484470905,
-0.00359775545859465));
#39887=CARTESIAN_POINT('Ctrl Pts',(-18.0800890420313,-3.93550024191007,
-0.321368632766151));
#39888=CARTESIAN_POINT('Ctrl Pts',(-18.0640145620277,-3.90021738496414,
-0.638504667178511));
#39889=CARTESIAN_POINT('Ctrl Pts',(-18.0479400820241,-3.82428761157383,
-0.945590376684499));
#39890=CARTESIAN_POINT('Ctrl Pts',(-17.9817823647814,-3.51178353821415,
-2.2094626471555));
#39891=CARTESIAN_POINT('Ctrl Pts',(-17.9156246475387,-2.51076231488021,
-3.30309270330469));
#39892=CARTESIAN_POINT('Ctrl Pts',(-17.849466930296,-1.27940038582653,-3.72591620266241));
#39893=CARTESIAN_POINT('Ctrl Pts',(-17.7833092130533,-0.0480384567728447,
-4.14873970202014));
#39894=CARTESIAN_POINT('Ctrl Pts',(-17.7171514958106,1.41366417800062,-3.90075664458642));
#39895=CARTESIAN_POINT('Ctrl Pts',(-17.6509937785679,2.43667303636025,-3.09547111283409));
#39896=CARTESIAN_POINT('Ctrl Pts',(-17.5848360613252,3.45968189471991,-2.29018558108173));
#39897=CARTESIAN_POINT('Ctrl Pts',(-17.5186783440825,4.04399697666572,-0.927597575010803));
#39898=CARTESIAN_POINT('Ctrl Pts',(-17.4525206268397,3.9221719980135,0.368624082927527));
#39899=CARTESIAN_POINT('Ctrl Pts',(-17.386362909597,3.80034701936129,1.66484574086582));
#39900=CARTESIAN_POINT('Ctrl Pts',(-17.3202051923543,2.97238198011102,2.89470105067148));
#39901=CARTESIAN_POINT('Ctrl Pts',(-17.2540474751116,1.81724394790119,3.49527414237165));
#39902=CARTESIAN_POINT('Ctrl Pts',(-17.1878897578689,0.66210591569132,4.09584723407185));
#39903=CARTESIAN_POINT('Ctrl Pts',(-17.1217320406262,-0.82020510947818,
4.06713810766653));
#39904=CARTESIAN_POINT('Ctrl Pts',(-17.0555743233835,-1.9512219992786,3.42228718929996));
#39905=CARTESIAN_POINT('Ctrl Pts',(-16.9894166061408,-3.08223888907898,
2.77743627093341));
#39906=CARTESIAN_POINT('Ctrl Pts',(-16.9232588888981,-3.86196164351034,
1.51644356060562));
#39907=CARTESIAN_POINT('Ctrl Pts',(-16.8571011716554,-3.93350412389534,
0.216476797402691));
#39908=CARTESIAN_POINT('Ctrl Pts',(-16.8534552884485,-3.93744675581616,
0.144836976850907));
#39909=CARTESIAN_POINT('Ctrl Pts',(-16.8498094052417,-3.93923864578278,
0.0730787921851864));
#39910=CARTESIAN_POINT('Ctrl Pts',(-16.8461635220349,-3.93892856332975,
0.00130481274881613));
#39911=CARTESIAN_POINT('Origin',(-27.25,0.,0.));
#39912=CARTESIAN_POINT('',(-15.4128364779651,-3.92904698718966,0.00291690129643835));
#39913=CARTESIAN_POINT('',(-15.5961635220349,-3.92874808319062,0.00278058184941524));
#39914=CARTESIAN_POINT('',(-27.25,-3.933,-4.81653586104654E-16));
#39915=CARTESIAN_POINT('Ctrl Pts',(-15.4128364779651,-3.92904698718966,
0.00291690129643835));
#39916=CARTESIAN_POINT('Ctrl Pts',(-15.4355262635747,-3.93214136813459,
0.452493402373492));
#39917=CARTESIAN_POINT('Ctrl Pts',(-15.4582160491844,-3.86091700943663,
0.901119249181804));
#39918=CARTESIAN_POINT('Ctrl Pts',(-15.4809058347941,-3.71110271172466,
1.32175433405916));
#39919=CARTESIAN_POINT('Ctrl Pts',(-15.5470635520368,-3.27428183922111,
2.5482206165698));
#39920=CARTESIAN_POINT('Ctrl Pts',(-15.6132212692795,-2.16932140142824,
3.53672087259794));
#39921=CARTESIAN_POINT('Ctrl Pts',(-15.6793789865222,-0.901971758706727,
3.83480961757815));
#39922=CARTESIAN_POINT('Ctrl Pts',(-15.7455367037649,0.365377884014899,
4.13289836255838));
#39923=CARTESIAN_POINT('Ctrl Pts',(-15.8116944210077,1.79511673166521,3.74057559649053));
#39924=CARTESIAN_POINT('Ctrl Pts',(-15.8778521382504,2.73284041582605,2.83741098859542));
#39925=CARTESIAN_POINT('Ctrl Pts',(-15.9440098554931,3.67056409998685,1.93424638070035));
#39926=CARTESIAN_POINT('Ctrl Pts',(-16.0101675727358,4.11627262065823,0.520239930978085));
#39927=CARTESIAN_POINT('Ctrl Pts',(-16.0763252899785,3.86596116713799,-0.757404852608853));
#39928=CARTESIAN_POINT('Ctrl Pts',(-16.1424830072212,3.61564971361774,-2.03504963619579));
#39929=CARTESIAN_POINT('Ctrl Pts',(-16.2086407244639,2.66931828590586,-3.1763327536474));
#39930=CARTESIAN_POINT('Ctrl Pts',(-16.2747984417066,1.46011131543732,-3.65887862645186));
#39931=CARTESIAN_POINT('Ctrl Pts',(-16.3409561589493,0.250904344968778,
-4.14142449925632));
#39932=CARTESIAN_POINT('Ctrl Pts',(-16.4071138761921,-1.22117816825643,
-3.96523312741364));
#39933=CARTESIAN_POINT('Ctrl Pts',(-16.4732715934348,-2.28235077809922,
-3.21094889126006));
#39934=CARTESIAN_POINT('Ctrl Pts',(-16.5364598882782,-3.29589372584808,
-2.49051994213288));
#39935=CARTESIAN_POINT('Ctrl Pts',(-16.5996481831216,-3.9345855153387,-1.24272774869351));
#39936=CARTESIAN_POINT('Ctrl Pts',(-16.662836477965,-3.93909976961691,0.00107240331368951));
#39937=CARTESIAN_POINT('Ctrl Pts',(-16.8461635220349,-3.93892856332975,
0.00130481274881613));
#39938=CARTESIAN_POINT('Ctrl Pts',(-16.783651687999,-3.9336119303655,-1.22932240049576));
#39939=CARTESIAN_POINT('Ctrl Pts',(-16.7211398539631,-3.31035574987545,
-2.46459297315745));
#39940=CARTESIAN_POINT('Ctrl Pts',(-16.6586280199272,-2.3149856042573,-3.18750036056419));
#39941=CARTESIAN_POINT('Ctrl Pts',(-16.5924703026845,-1.26156239789562,
-3.95256993925005));
#39942=CARTESIAN_POINT('Ctrl Pts',(-16.5263125854418,0.208646221166482,
-4.14376828054371));
#39943=CARTESIAN_POINT('Ctrl Pts',(-16.4601548681991,1.42271250505289,-3.67358217881151));
#39944=CARTESIAN_POINT('Ctrl Pts',(-16.3939971509564,2.63677878893936,-3.20339607707928));
#39945=CARTESIAN_POINT('Ctrl Pts',(-16.3278394337137,3.59470273765017,-2.07182553232115));
#39946=CARTESIAN_POINT('Ctrl Pts',(-16.261681716471,3.8580339183116,-0.796800590908822));
#39947=CARTESIAN_POINT('Ctrl Pts',(-16.1955239992282,4.121365098973,0.478224350503403));
#39948=CARTESIAN_POINT('Ctrl Pts',(-16.1293662819855,3.69010351158514,1.89670368856975));
#39949=CARTESIAN_POINT('Ctrl Pts',(-16.0632085647428,2.7616414751588,2.80938663398225));
#39950=CARTESIAN_POINT('Ctrl Pts',(-15.9970508475001,1.83317943873238,3.72206957939482));
#39951=CARTESIAN_POINT('Ctrl Pts',(-15.9308931302574,0.407516953267295,
4.12895613215341));
#39952=CARTESIAN_POINT('Ctrl Pts',(-15.8647354130147,-0.862807400563734,
3.84381064648713));
#39953=CARTESIAN_POINT('Ctrl Pts',(-15.798577695772,-2.13313175439469,3.55866516082088));
#39954=CARTESIAN_POINT('Ctrl Pts',(-15.7324199785293,-3.24811797659165,
2.58148763672992));
#39955=CARTESIAN_POINT('Ctrl Pts',(-15.6662622612866,-3.69742681482843,
1.35954104222826));
#39956=CARTESIAN_POINT('Ctrl Pts',(-15.6428960148693,-3.85611821878305,
0.927961682694594));
#39957=CARTESIAN_POINT('Ctrl Pts',(-15.6195297684521,-3.93177089551102,
0.465849045989298));
#39958=CARTESIAN_POINT('Ctrl Pts',(-15.5961635220349,-3.92874808319062,
0.00278058184941524));
#39959=CARTESIAN_POINT('Origin',(-27.25,0.,0.));
#39960=CARTESIAN_POINT('',(-14.1628364779651,-3.92858680232973,-0.00269909542886165));
#39961=CARTESIAN_POINT('',(-14.3461635220349,-3.92887651838583,-0.00284137689771559));
#39962=CARTESIAN_POINT('',(-27.25,-3.933,-4.81653586104654E-16));
#39963=CARTESIAN_POINT('Ctrl Pts',(-14.1628364779651,-3.92858680232973,
-0.00269909542886165));
#39964=CARTESIAN_POINT('Ctrl Pts',(-14.2052466267851,-3.92327502960724,
0.837865115529639));
#39965=CARTESIAN_POINT('Ctrl Pts',(-14.2476567756052,-3.65903126967813,
1.6814769480063));
#39966=CARTESIAN_POINT('Ctrl Pts',(-14.2900669244253,-3.16092681968387,
2.35114004201739));
#39967=CARTESIAN_POINT('Ctrl Pts',(-14.356224641668,-2.38390871725174,3.39578107379964));
#39968=CARTESIAN_POINT('Ctrl Pts',(-14.4223823589108,-1.03780362497608,
4.01712751967761));
#39969=CARTESIAN_POINT('Ctrl Pts',(-14.4885400761535,0.261264013030088,
3.93078350613078));
#39970=CARTESIAN_POINT('Ctrl Pts',(-14.5546977933962,1.56033165103629,3.84443949258394));
#39971=CARTESIAN_POINT('Ctrl Pts',(-14.6208555106389,2.81236183477307,3.05040501961242));
#39972=CARTESIAN_POINT('Ctrl Pts',(-14.6870132278816,3.44428905442718,1.91211682857702));
#39973=CARTESIAN_POINT('Ctrl Pts',(-14.7531709451243,4.07621627408126,0.773828637541696));
#39974=CARTESIAN_POINT('Ctrl Pts',(-14.819328662367,4.08804052965268,-0.708713271557329));
#39975=CARTESIAN_POINT('Ctrl Pts',(-14.8854863796097,3.47434975269838,-1.85693609273422));
#39976=CARTESIAN_POINT('Ctrl Pts',(-14.9516440968524,2.86065897574404,-3.00515891391118));
#39977=CARTESIAN_POINT('Ctrl Pts',(-15.0178018140951,1.62145316626383,-3.81906264716589));
#39978=CARTESIAN_POINT('Ctrl Pts',(-15.0839595313379,0.32392800228367,-3.92611621146278));
#39979=CARTESIAN_POINT('Ctrl Pts',(-15.1501172485806,-0.973597161696452,
-4.03316977575966));
#39980=CARTESIAN_POINT('Ctrl Pts',(-15.2162749658233,-2.32944168017656,
-3.43337317109877));
#39981=CARTESIAN_POINT('Ctrl Pts',(-15.282432683066,-3.1230232858095,-2.40125871427174));
#39982=CARTESIAN_POINT('Ctrl Pts',(-15.325900614699,-3.64443412669937,-1.72312345633623));
#39983=CARTESIAN_POINT('Ctrl Pts',(-15.369368546332,-3.92311893032414,-0.858358782343565));
#39984=CARTESIAN_POINT('Ctrl Pts',(-15.4128364779651,-3.92904698718966,
0.00291690129643835));
#39985=CARTESIAN_POINT('Ctrl Pts',(-15.5961635220349,-3.92874808319062,
0.00278058184941524));
#39986=CARTESIAN_POINT('Ctrl Pts',(-15.5533720512094,-3.92321229524635,
-0.845253814416959));
#39987=CARTESIAN_POINT('Ctrl Pts',(-15.5105805803839,-3.65381503891493,
-1.69649386003438));
#39988=CARTESIAN_POINT('Ctrl Pts',(-15.4677891095584,-3.14735501292257,
-2.36927696125771));
#39989=CARTESIAN_POINT('Ctrl Pts',(-15.4016313923157,-2.36434291850349,
-3.40943270532938));
#39990=CARTESIAN_POINT('Ctrl Pts',(-15.335473675073,-1.01468727538901,-4.0230285285604));
#39991=CARTESIAN_POINT('Ctrl Pts',(-15.2693159578303,0.28386235315941,-3.92921608733526));
#39992=CARTESIAN_POINT('Ctrl Pts',(-15.2031582405876,1.58241198170787,-3.83540364611011));
#39993=CARTESIAN_POINT('Ctrl Pts',(-15.1370005233449,2.82985559569023,-3.03418294042861));
#39994=CARTESIAN_POINT('Ctrl Pts',(-15.0708428061022,3.45522699964562,-1.892279915191));
#39995=CARTESIAN_POINT('Ctrl Pts',(-15.0046850888595,4.08059840360102,-0.750376889953396));
#39996=CARTESIAN_POINT('Ctrl Pts',(-14.9385273716168,4.08389759752955,0.732208454840364));
#39997=CARTESIAN_POINT('Ctrl Pts',(-14.8723696543741,3.46361451060769,1.87688343229494));
#39998=CARTESIAN_POINT('Ctrl Pts',(-14.8062119371313,2.84333142368583,3.02155840974951));
#39999=CARTESIAN_POINT('Ctrl Pts',(-14.7400542198886,1.59946605591359,3.8283230198649));
#40000=CARTESIAN_POINT('Ctrl Pts',(-14.6738965026459,0.301346807181522,
3.92791382266934));
#40001=CARTESIAN_POINT('Ctrl Pts',(-14.6077387854032,-0.996772441550546,
4.02750462547378));
#40002=CARTESIAN_POINT('Ctrl Pts',(-14.5415810681605,-2.34914557124244,
3.41992162096726));
#40003=CARTESIAN_POINT('Ctrl Pts',(-14.4754233509178,-3.13677920051122,
2.38326103139282));
#40004=CARTESIAN_POINT('Ctrl Pts',(-14.4323367412902,-3.64974222475523,
1.70811394348043));
#40005=CARTESIAN_POINT('Ctrl Pts',(-14.3892501316625,-3.92316870128949,
0.850971859025732));
#40006=CARTESIAN_POINT('Ctrl Pts',(-14.3461635220349,-3.92887651838583,
-0.00284137689771559));
#40007=CARTESIAN_POINT('Origin',(-27.25,0.,0.));
#40008=CARTESIAN_POINT('',(-12.9128364779651,-3.93881934497104,-0.00143284320175408));
#40009=CARTESIAN_POINT('',(-13.0961635220349,-3.93900688952732,-0.0012041997225416));
#40010=CARTESIAN_POINT('',(-27.25,-3.933,-4.81653586104654E-16));
#40011=CARTESIAN_POINT('Ctrl Pts',(-12.9128364779651,-3.93881934497104,
-0.00143284320175408));
#40012=CARTESIAN_POINT('Ctrl Pts',(-12.9749669899956,-3.93308493623946,
1.22177796479248));
#40013=CARTESIAN_POINT('Ctrl Pts',(-13.0370975020261,-3.31842665197076,
2.44996177311049));
#40014=CARTESIAN_POINT('Ctrl Pts',(-13.0992280140566,-2.33327606901329,
3.17413620412613));
#40015=CARTESIAN_POINT('Ctrl Pts',(-13.1653857312993,-1.28426952490503,
3.94525051939226));
#40016=CARTESIAN_POINT('Ctrl Pts',(-13.231543448542,0.184815410869772,4.14489965346203));
#40017=CARTESIAN_POINT('Ctrl Pts',(-13.2977011657847,1.40156531041257,3.68170239661253));
#40018=CARTESIAN_POINT('Ctrl Pts',(-13.3638588830274,2.61831520995538,3.21850513976302));
#40019=CARTESIAN_POINT('Ctrl Pts',(-13.4300166002701,3.58273007326619,2.09246149199423));
#40020=CARTESIAN_POINT('Ctrl Pts',(-13.4961743175128,3.85338851730353,0.818971789067029));
#40021=CARTESIAN_POINT('Ctrl Pts',(-13.5623320347555,4.12404696134087,-0.454517913860173));
#40022=CARTESIAN_POINT('Ctrl Pts',(-13.6284897519982,3.70094898610474,-1.87545367194579));
#40023=CARTESIAN_POINT('Ctrl Pts',(-13.6946474692409,2.77775035167917,-2.79346037027924));
#40024=CARTESIAN_POINT('Ctrl Pts',(-13.7608051864837,1.85455171725356,-3.71146706861271));
#40025=CARTESIAN_POINT('Ctrl Pts',(-13.8269629037264,0.431252423638476,
-4.12654470719399));
#40026=CARTESIAN_POINT('Ctrl Pts',(-13.8931206209691,-0.840690602721897,
-3.8487085063784));
#40027=CARTESIAN_POINT('Ctrl Pts',(-13.9592783382118,-2.11263362908223,
-3.57087230556282));
#40028=CARTESIAN_POINT('Ctrl Pts',(-14.0254360554545,-3.23322038818787,
-2.60012226535041));
#40029=CARTESIAN_POINT('Ctrl Pts',(-14.0915937726972,-3.68954821144631,
-1.38077943640092));
#40030=CARTESIAN_POINT('Ctrl Pts',(-14.1153413411198,-3.85334884813117,
-0.943091613000512));
#40031=CARTESIAN_POINT('Ctrl Pts',(-14.1390889095424,-3.93156113016593,
-0.473373136164104));
#40032=CARTESIAN_POINT('Ctrl Pts',(-14.1628364779651,-3.92858680232973,
-0.00269909542886165));
#40033=CARTESIAN_POINT('Ctrl Pts',(-14.3461635220349,-3.92887651838583,
-0.00284137689771559));
#40034=CARTESIAN_POINT('Ctrl Pts',(-14.3230924144198,-3.93193281971971,
-0.460023253573669));
#40035=CARTESIAN_POINT('Ctrl Pts',(-14.3000213068047,-3.85822984188482,
-0.916250695417715));
#40036=CARTESIAN_POINT('Ctrl Pts',(-14.2769501991897,-3.70344093352043,
-1.34307190739762));
#40037=CARTESIAN_POINT('Ctrl Pts',(-14.210792481947,-3.2595749084152,-2.56700608197123));
#40038=CARTESIAN_POINT('Ctrl Pts',(-14.1446347647043,-2.14894872935906,
-3.54913625647613));
#40039=CARTESIAN_POINT('Ctrl Pts',(-14.0784770474615,-0.879906017600263,
-3.83993259012528));
#40040=CARTESIAN_POINT('Ctrl Pts',(-14.0123193302188,0.389136694158539,
-4.13072892377443));
#40041=CARTESIAN_POINT('Ctrl Pts',(-13.9461616129761,1.81659593862004,-3.73019141656785));
#40042=CARTESIAN_POINT('Ctrl Pts',(-13.8800038957334,2.74911074231022,-2.82164969885171));
#40043=CARTESIAN_POINT('Ctrl Pts',(-13.8138461784907,3.68162554600042,-1.91310798113555));
#40044=CARTESIAN_POINT('Ctrl Pts',(-13.747688461248,4.11919590891929,-0.496562052909773));
#40045=CARTESIAN_POINT('Ctrl Pts',(-13.6815307440053,3.86154192858324,0.77962223564303));
#40046=CARTESIAN_POINT('Ctrl Pts',(-13.6153730267626,3.60388794824719,2.0558065241958));
#40047=CARTESIAN_POINT('Ctrl Pts',(-13.5492153095199,2.65100962465633,3.19162917307553));
#40048=CARTESIAN_POINT('Ctrl Pts',(-13.4830575922772,1.43904796254968,3.66721390949546));
#40049=CARTESIAN_POINT('Ctrl Pts',(-13.4168998750344,0.227086300443004,
4.14279864591541));
#40050=CARTESIAN_POINT('Ctrl Pts',(-13.3507421577917,-1.24395870017946,
3.95814546987541));
#40051=CARTESIAN_POINT('Ctrl Pts',(-13.284584440549,-2.30077647205636,3.19777180582781));
#40052=CARTESIAN_POINT('Ctrl Pts',(-13.221777467711,-3.30406872365444,2.47590941312473));
#40053=CARTESIAN_POINT('Ctrl Pts',(-13.1589704948729,-3.9340305853428,1.23516767268343));
#40054=CARTESIAN_POINT('Ctrl Pts',(-13.0961635220349,-3.93900688952732,
-0.0012041997225416));
#40055=CARTESIAN_POINT('Origin',(-27.25,0.,0.));
#40056=CARTESIAN_POINT('',(-11.6628364779651,-3.93283223678505,0.00359684100027402));
#40057=CARTESIAN_POINT('',(-11.8461635220349,-3.93242970906489,0.00359528210897375));
#40058=CARTESIAN_POINT('',(-27.25,-3.933,-4.81653586104654E-16));
#40059=CARTESIAN_POINT('Ctrl Pts',(-11.6628364779651,-3.93283223678505,
0.00359684100027402));
#40060=CARTESIAN_POINT('Ctrl Pts',(-11.6785296359633,-3.93567289122675,
0.313783719918517));
#40061=CARTESIAN_POINT('Ctrl Pts',(-11.6942227939615,-3.90206523256919,
0.623362207654243));
#40062=CARTESIAN_POINT('Ctrl Pts',(-11.7099159519597,-3.82966180971454,
0.923584473553057));
#40063=CARTESIAN_POINT('Ctrl Pts',(-11.7760736692024,-3.52443037209239,
2.18923283952105));
#40064=CARTESIAN_POINT('Ctrl Pts',(-11.8422313864451,-2.52971422453108,
3.28860089028295));
#40065=CARTESIAN_POINT('Ctrl Pts',(-11.9083891036878,-1.30080392122511,
3.71849795147176));
#40066=CARTESIAN_POINT('Ctrl Pts',(-11.9745468209305,-0.0718936179191432,
4.14839501266058));
#40067=CARTESIAN_POINT('Ctrl Pts',(-12.0407045381732,1.39121084113145,3.90882108427631));
#40068=CARTESIAN_POINT('Ctrl Pts',(-12.1068622554159,2.41883334617547,3.10943131456605));
#40069=CARTESIAN_POINT('Ctrl Pts',(-12.1730199726586,3.44645585121948,2.31004154485579));
#40070=CARTESIAN_POINT('Ctrl Pts',(-12.2391776899013,4.03859640225687,0.950835933819561));
#40071=CARTESIAN_POINT('Ctrl Pts',(-12.305335407144,3.92422692730571,-0.346064848811758));
#40072=CARTESIAN_POINT('Ctrl Pts',(-12.3714931243867,3.80985745235456,-1.64296563144304));
#40073=CARTESIAN_POINT('Ctrl Pts',(-12.4376508416295,2.98897795141481,-2.87756158566949));
#40074=CARTESIAN_POINT('Ctrl Pts',(-12.5038085588722,1.83731237732077,-3.48476700580085));
#40075=CARTESIAN_POINT('Ctrl Pts',(-12.5699662761149,0.685646803226695,
-4.09197242593223));
#40076=CARTESIAN_POINT('Ctrl Pts',(-12.6361239933576,-0.796804844021701,
-4.07178731196857));
#40077=CARTESIAN_POINT('Ctrl Pts',(-12.7022817106003,-1.93151107210173,
-3.43345057266342));
#40078=CARTESIAN_POINT('Ctrl Pts',(-12.768439427843,-3.06621730018176,-2.79511383335826));
#40079=CARTESIAN_POINT('Ctrl Pts',(-12.8345971450857,-3.8531781090934,-1.53862546871164));
#40080=CARTESIAN_POINT('Ctrl Pts',(-12.9007548623284,-3.93219443732835,
-0.239091538157064));
#40081=CARTESIAN_POINT('Ctrl Pts',(-12.9047820675406,-3.93700438214174,
-0.159985274569187));
#40082=CARTESIAN_POINT('Ctrl Pts',(-12.9088092727529,-3.93919104061586,
-0.0807195057544253));
#40083=CARTESIAN_POINT('Ctrl Pts',(-12.9128364779651,-3.93881934497104,
-0.00143284320175408));
#40084=CARTESIAN_POINT('Ctrl Pts',(-13.0961635220349,-3.93900688952732,
-0.0012041997225416));
#40085=CARTESIAN_POINT('Ctrl Pts',(-13.0928127776302,-3.9392723747537,-0.0671644895814343));
#40086=CARTESIAN_POINT('Ctrl Pts',(-13.0894620332256,-3.93775902008951,
-0.133112341879996));
#40087=CARTESIAN_POINT('Ctrl Pts',(-13.0861112888209,-3.93442861297152,
-0.198968303873675));
#40088=CARTESIAN_POINT('Ctrl Pts',(-13.0199535715782,-3.86867243887846,
-1.49924059747244));
#40089=CARTESIAN_POINT('Ctrl Pts',(-12.9537958543355,-3.09456954756098,
-2.76369103261481));
#40090=CARTESIAN_POINT('Ctrl Pts',(-12.8876381370927,-1.96643381565171,
-3.41356923837453));
#40091=CARTESIAN_POINT('Ctrl Pts',(-12.82148041985,-0.838298083742433,-4.06344744413424));
#40092=CARTESIAN_POINT('Ctrl Pts',(-12.7553227026073,0.643870488758641,
-4.09875342051129));
#40093=CARTESIAN_POINT('Ctrl Pts',(-12.6891649853646,1.80166997539429,-3.50332730361839));
#40094=CARTESIAN_POINT('Ctrl Pts',(-12.6230072681219,2.95946946202995,-2.90790118672549));
#40095=CARTESIAN_POINT('Ctrl Pts',(-12.5568495508792,3.79289986280018,-1.68174297656263));
#40096=CARTESIAN_POINT('Ctrl Pts',(-12.4906918336365,3.92049256479515,-0.386076347244129));
#40097=CARTESIAN_POINT('Ctrl Pts',(-12.4245341163938,4.04808526679012,0.909590282074408));
#40098=CARTESIAN_POINT('Ctrl Pts',(-12.3583763991511,3.46984027000979,2.27476533054859));
#40099=CARTESIAN_POINT('Ctrl Pts',(-12.2922186819084,2.45042552589917,3.08459586308112));
#40100=CARTESIAN_POINT('Ctrl Pts',(-12.2260609646657,1.43101078178864,3.89442639561358));
#40101=CARTESIAN_POINT('Ctrl Pts',(-12.1599032474229,-0.0295737096520995,
4.14891241220449));
#40102=CARTESIAN_POINT('Ctrl Pts',(-12.0937455301802,-1.26280525057983,
3.73157336731082));
#40103=CARTESIAN_POINT('Ctrl Pts',(-12.0275878129375,-2.4960367915077,3.31423432241709));
#40104=CARTESIAN_POINT('Ctrl Pts',(-11.9614300956948,-3.5019153819225,2.22507021603861));
#40105=CARTESIAN_POINT('Ctrl Pts',(-11.8952723784521,-3.82004131683789,
0.962601285147102));
#40106=CARTESIAN_POINT('Ctrl Pts',(-11.8789027596464,-3.89875624993747,
0.650224498067916));
#40107=CARTESIAN_POINT('Ctrl Pts',(-11.8625331408406,-3.93536475652441,
0.327237433006823));
#40108=CARTESIAN_POINT('Ctrl Pts',(-11.8461635220349,-3.93242970906489,
0.00359528210897375));
#40109=CARTESIAN_POINT('Origin',(-27.25,0.,0.));
#40110=CARTESIAN_POINT('',(-10.4128364779651,-3.92668394074156,-0.000755260177356665));
#40111=CARTESIAN_POINT('',(-10.5961635220349,-3.92677159154525,-0.000969419521030996));
#40112=CARTESIAN_POINT('',(-27.25,-3.933,-4.81653586104654E-16));
#40113=CARTESIAN_POINT('Ctrl Pts',(-10.4128364779651,-3.92668394074156,
-0.000755260177356665));
#40114=CARTESIAN_POINT('Ctrl Pts',(-10.4482499991737,-3.9254780780401,0.701988440301541));
#40115=CARTESIAN_POINT('Ctrl Pts',(-10.4836635203823,-3.74567922430472,
1.40530796224216));
#40116=CARTESIAN_POINT('Ctrl Pts',(-10.5190770415909,-3.39095092494106,
2.00518569743945));
#40117=CARTESIAN_POINT('Ctrl Pts',(-10.5852347588336,-2.72826577739384,
3.12584640077951));
#40118=CARTESIAN_POINT('Ctrl Pts',(-10.6513924760763,-1.45508055671478,
3.88549745165729));
#40119=CARTESIAN_POINT('Ctrl Pts',(-10.717550193319,-0.154143623967885,
3.93643971118121));
#40120=CARTESIAN_POINT('Ctrl Pts',(-10.7837079105617,1.14679330877898,3.98738197070513));
#40121=CARTESIAN_POINT('Ctrl Pts',(-10.8498656278044,2.47548195359371,3.32961543887524));
#40122=CARTESIAN_POINT('Ctrl Pts',(-10.9160233450471,3.22376953148229,2.26420579110221));
#40123=CARTESIAN_POINT('Ctrl Pts',(-10.9821810622898,3.97205710937091,1.19879614332912));
#40124=CARTESIAN_POINT('Ctrl Pts',(-11.0483387795326,4.13994362033332,-0.274256620387207));
#40125=CARTESIAN_POINT('Ctrl Pts',(-11.1144964967753,3.65058589377732,-1.48072296150509));
#40126=CARTESIAN_POINT('Ctrl Pts',(-11.180654214018,3.16122816722133,-2.68718930262293));
#40127=CARTESIAN_POINT('Ctrl Pts',(-11.2468119312607,2.01462620314707,-3.6270692211423));
#40128=CARTESIAN_POINT('Ctrl Pts',(-11.3129696485034,0.735590064147372,
-3.87017119958562));
#40129=CARTESIAN_POINT('Ctrl Pts',(-11.3791273657461,-0.543446074852362,
-4.11327317802895));
#40130=CARTESIAN_POINT('Ctrl Pts',(-11.4452850829888,-1.9549163887775,-3.65959721639607));
#40131=CARTESIAN_POINT('Ctrl Pts',(-11.5114428002315,-2.85277818189858,
-2.71679489499259));
#40132=CARTESIAN_POINT('Ctrl Pts',(-11.561907359476,-3.53765972770696,-1.99763308610216));
#40133=CARTESIAN_POINT('Ctrl Pts',(-11.6123719187205,-3.92369753143239,
-0.993872510282313));
#40134=CARTESIAN_POINT('Ctrl Pts',(-11.6628364779651,-3.93283223678505,
0.00359684100027402));
#40135=CARTESIAN_POINT('Ctrl Pts',(-11.8461635220349,-3.93242970906489,
0.00359528210897375));
#40136=CARTESIAN_POINT('Ctrl Pts',(-11.7963754235979,-3.92350277963752,
-0.980760398892982));
#40137=CARTESIAN_POINT('Ctrl Pts',(-11.746587325161,-3.54877084267473,-1.97117607336868));
#40138=CARTESIAN_POINT('Ctrl Pts',(-11.696799226724,-2.88034263954507,-2.68755338092733));
#40139=CARTESIAN_POINT('Ctrl Pts',(-11.6306415094813,-1.9921447479208,-3.63946536070601));
#40140=CARTESIAN_POINT('Ctrl Pts',(-11.5644837922386,-0.585375685256206,
-4.1075155648589));
#40141=CARTESIAN_POINT('Ctrl Pts',(-11.4983260749959,0.696073657831846,
-3.87747319260726));
#40142=CARTESIAN_POINT('Ctrl Pts',(-11.4321683577532,1.9775230009199,-3.64743082035563));
#40143=CARTESIAN_POINT('Ctrl Pts',(-11.3660106405104,3.13365262443137,-2.71929587169946));
#40144=CARTESIAN_POINT('Ctrl Pts',(-11.2998529232677,3.63529157009874,-1.51788408545725));
#40145=CARTESIAN_POINT('Ctrl Pts',(-11.233695206025,4.13693051576613,-0.316472299215008));
#40146=CARTESIAN_POINT('Ctrl Pts',(-11.1675374887823,3.98407878358935,1.15821632461326));
#40147=CARTESIAN_POINT('Ctrl Pts',(-11.1013797715396,3.24669799027985,2.23120349955538));
#40148=CARTESIAN_POINT('Ctrl Pts',(-11.0352220542969,2.50931719697037,3.30419067449748));
#40149=CARTESIAN_POINT('Ctrl Pts',(-10.9690643370542,1.18740734252809,3.97547640055349));
#40150=CARTESIAN_POINT('Ctrl Pts',(-10.9029066198114,-0.113981507558553,
3.93780714515707));
#40151=CARTESIAN_POINT('Ctrl Pts',(-10.8367489025687,-1.41537035764512,
3.90013788976065));
#40152=CARTESIAN_POINT('Ctrl Pts',(-10.770591185326,-2.69623820337613,3.15351365291197));
#40153=CARTESIAN_POINT('Ctrl Pts',(-10.7044334680833,-3.37032027689551,
2.03967108320493));
#40154=CARTESIAN_POINT('Ctrl Pts',(-10.6683434860672,-3.73804169965065,
1.43205401319522));
#40155=CARTESIAN_POINT('Ctrl Pts',(-10.6322535040511,-3.92519224964437,
0.715157955617078));
#40156=CARTESIAN_POINT('Ctrl Pts',(-10.5961635220349,-3.92677159154525,
-0.000969419521030996));
#40157=CARTESIAN_POINT('Origin',(-27.25,0.,0.));
#40158=CARTESIAN_POINT('',(-9.16283647796508,-3.93560336451511,-0.00320692409599477));
#40159=CARTESIAN_POINT('',(-9.34616352203492,-3.93598498577306,-0.00309328146845306));
#40160=CARTESIAN_POINT('',(-27.25,-3.933,-4.81653586104654E-16));
#40161=CARTESIAN_POINT('Ctrl Pts',(-9.16283647796508,-3.93560336451511,
-0.00320692409599477));
#40162=CARTESIAN_POINT('Ctrl Pts',(-9.21797036238408,-3.92600068327744,
1.08458219431681));
#40163=CARTESIAN_POINT('Ctrl Pts',(-9.27310424680308,-3.45624748136882,
2.17965170096766));
#40164=CARTESIAN_POINT('Ctrl Pts',(-9.32823813122209,-2.65457303229532,
2.91076620029585));
#40165=CARTESIAN_POINT('Ctrl Pts',(-9.3943958484648,-1.69260650152374,3.78806455916005));
#40166=CARTESIAN_POINT('Ctrl Pts',(-9.46055356570752,-0.252715911624579,
4.14131434950024));
#40167=CARTESIAN_POINT('Ctrl Pts',(-9.52671128295023,1.00604782497662,3.80882995556827));
#40168=CARTESIAN_POINT('Ctrl Pts',(-9.59286900019294,2.26481156157778,3.4763455616363));
#40169=CARTESIAN_POINT('Ctrl Pts',(-9.65902671743565,3.34244844488098,2.4581269834322));
#40170=CARTESIAN_POINT('Ctrl Pts',(-9.72518443467836,3.74571435190455,1.22022204967401));
#40171=CARTESIAN_POINT('Ctrl Pts',(-9.79134215192107,4.14898025892809,-0.0176828840841227));
#40172=CARTESIAN_POINT('Ctrl Pts',(-9.85749986916378,3.87787518967209,-1.47527417339632));
#40173=CARTESIAN_POINT('Ctrl Pts',(-9.92365758640649,3.05648638000691,-2.48539913603562));
#40174=CARTESIAN_POINT('Ctrl Pts',(-9.9898153036492,2.2350975703417,-3.49552409867495));
#40175=CARTESIAN_POINT('Ctrl Pts',(-10.0559730208919,0.863425020267273,
-4.05818273464135));
#40176=CARTESIAN_POINT('Ctrl Pts',(-10.1221307381346,-0.430704370021922,
-3.91584111044081));
#40177=CARTESIAN_POINT('Ctrl Pts',(-10.1882884553773,-1.72483376031112,
-3.77349948624028));
#40178=CARTESIAN_POINT('Ctrl Pts',(-10.25444617262,-2.94141999081508,-2.92615760187282));
#40179=CARTESIAN_POINT('Ctrl Pts',(-10.3206038898627,-3.52362056885937,
-1.7616514817879));
#40180=CARTESIAN_POINT('Ctrl Pts',(-10.3513480858969,-3.794175380128,-1.22049308136327));
#40181=CARTESIAN_POINT('Ctrl Pts',(-10.382092281931,-3.92773080866145,-0.610841163863507));
#40182=CARTESIAN_POINT('Ctrl Pts',(-10.4128364779651,-3.92668394074156,
-0.000755260177356665));
#40183=CARTESIAN_POINT('Ctrl Pts',(-10.5961635220349,-3.92677159154525,
-0.000969419521030996));
#40184=CARTESIAN_POINT('Ctrl Pts',(-10.5660957868083,-3.92808739253641,
-0.59759837584792));
#40185=CARTESIAN_POINT('Ctrl Pts',(-10.5360280515818,-3.80059642103898,
-1.19369378224975));
#40186=CARTESIAN_POINT('Ctrl Pts',(-10.5059603163552,-3.54140705662186,
-1.72561668855637));
#40187=CARTESIAN_POINT('Ctrl Pts',(-10.4398025991125,-2.97111546152114,
-2.89600098804493));
#40188=CARTESIAN_POINT('Ctrl Pts',(-10.3736448818698,-1.76323597001208,
-3.7557086844566));
#40189=CARTESIAN_POINT('Ctrl Pts',(-10.3074871646271,-0.470625921786567,
-3.9112438096158));
#40190=CARTESIAN_POINT('Ctrl Pts',(-10.2413294473844,0.821984126439017,
-4.06677893477501));
#40191=CARTESIAN_POINT('Ctrl Pts',(-10.1751717301416,2.19932473138106,-3.51814148868164));
#40192=CARTESIAN_POINT('Ctrl Pts',(-10.1090140128989,3.03097467299996,-2.51644777973797));
#40193=CARTESIAN_POINT('Ctrl Pts',(-10.0428562956562,3.86262461461886,-1.51475407079431));
#40194=CARTESIAN_POINT('Ctrl Pts',(-9.97669857841352,4.14858389291461,-0.0600040990003427));
#40195=CARTESIAN_POINT('Ctrl Pts',(-9.91054086117081,3.75796636653772,1.18194995007685));
#40196=CARTESIAN_POINT('Ctrl Pts',(-9.8443831439281,3.36734884016083,2.42390399915404));
#40197=CARTESIAN_POINT('Ctrl Pts',(-9.77822542668539,2.30015450911129,3.45306212551446));
#40198=CARTESIAN_POINT('Ctrl Pts',(-9.71206770944267,1.04484784600073,3.79836937056193));
#40199=CARTESIAN_POINT('Ctrl Pts',(-9.64590999219997,-0.210458817109762,
4.14367661560937));
#40200=CARTESIAN_POINT('Ctrl Pts',(-9.57975227495726,-1.65387781228124,
3.80513297934396));
#40201=CARTESIAN_POINT('Ctrl Pts',(-9.51359455771455,-2.62474324416494,
2.93769293812779));
#40202=CARTESIAN_POINT('Ctrl Pts',(-9.457784212488,-3.44376084604448,2.20592451894252));
#40203=CARTESIAN_POINT('Ctrl Pts',(-9.40197386726146,-3.92648420156164,
1.09776529091601));
#40204=CARTESIAN_POINT('Ctrl Pts',(-9.34616352203492,-3.93598498577306,
-0.00309328146845306));
#40205=CARTESIAN_POINT('Origin',(-27.25,0.,0.));
#40206=CARTESIAN_POINT('',(-7.91283647796508,-3.93687099541924,0.00275879756119139));
#40207=CARTESIAN_POINT('',(-8.09616352203492,-3.93651676133011,0.00290543094219859));
#40208=CARTESIAN_POINT('',(-27.25,-3.933,-4.81653586104654E-16));
#40209=CARTESIAN_POINT('Ctrl Pts',(-7.91283647796508,-3.93687099541924,
0.00275879756119139));
#40210=CARTESIAN_POINT('Ctrl Pts',(-7.92153300835178,-3.93823823749687,
0.174197263911898));
#40211=CARTESIAN_POINT('Ctrl Pts',(-7.93022953873848,-3.92800924152857,
0.345471489671227));
#40212=CARTESIAN_POINT('Ctrl Pts',(-7.93892606912519,-3.90562996449843,
0.515143122817789));
#40213=CARTESIAN_POINT('Ctrl Pts',(-8.0050837863679,-3.73538254213334,1.80589787565366));
#40214=CARTESIAN_POINT('Ctrl Pts',(-8.07124150361061,-2.86197325404654,
3.00390728327072));
#40215=CARTESIAN_POINT('Ctrl Pts',(-8.13739922085332,-1.68516941052714,
3.56083163241368));
#40216=CARTESIAN_POINT('Ctrl Pts',(-8.20355693809603,-0.508365567007741,
4.11775598155664));
#40217=CARTESIAN_POINT('Ctrl Pts',(-8.26971465533874,0.971832831944265,
4.03359527222549));
#40218=CARTESIAN_POINT('Ctrl Pts',(-8.33587237258145,2.07792562607827,3.34687062030512));
#40219=CARTESIAN_POINT('Ctrl Pts',(-8.40203008982416,3.18401842021227,2.66014596838474));
#40220=CARTESIAN_POINT('Ctrl Pts',(-8.46818780706687,3.91600560952826,1.37085737387514));
#40221=CARTESIAN_POINT('Ctrl Pts',(-8.53434552430958,3.93885005413059,0.0691238573130398));
#40222=CARTESIAN_POINT('Ctrl Pts',(-8.60050324155228,3.96169449873291,-1.23260965924906));
#40223=CARTESIAN_POINT('Ctrl Pts',(-8.666660958795,3.27539619862157,-2.54678809786367));
#40224=CARTESIAN_POINT('Ctrl Pts',(-8.73281867603771,2.1940800769382,-3.27190013181289));
#40225=CARTESIAN_POINT('Ctrl Pts',(-8.79897639328041,1.11276395525483,-3.99701216576211));
#40226=CARTESIAN_POINT('Ctrl Pts',(-8.86513411052312,-0.363569988000565,
-4.13305779504593));
#40227=CARTESIAN_POINT('Ctrl Pts',(-8.93129182776583,-1.55919038881141,
-3.61776770785694));
#40228=CARTESIAN_POINT('Ctrl Pts',(-8.99744954500854,-2.75481078962223,
-3.10247762066796));
#40229=CARTESIAN_POINT('Ctrl Pts',(-9.06360726225126,-3.66971764798851,
-1.93585181700621));
#40230=CARTESIAN_POINT('Ctrl Pts',(-9.12976497949396,-3.88514984134968,
-0.651865451481312));
#40231=CARTESIAN_POINT('Ctrl Pts',(-9.14078881231767,-3.92104721785293,
-0.437915339062323));
#40232=CARTESIAN_POINT('Ctrl Pts',(-9.15181264514137,-3.93752338799502,
-0.220706661602113));
#40233=CARTESIAN_POINT('Ctrl Pts',(-9.16283647796508,-3.93560336451511,
-0.00320692409599477));
#40234=CARTESIAN_POINT('Ctrl Pts',(-9.34616352203492,-3.93598498577306,
-0.00309328146845306));
#40235=CARTESIAN_POINT('Ctrl Pts',(-9.33581615001875,-3.93774645397904,
-0.207195104157573));
#40236=CARTESIAN_POINT('Ctrl Pts',(-9.32546877800259,-3.92324134568439,
-0.411045973741836));
#40237=CARTESIAN_POINT('Ctrl Pts',(-9.31512140598642,-3.89159701236423,
-0.612200612441036));
#40238=CARTESIAN_POINT('Ctrl Pts',(-9.24896368874371,-3.68927348008389,
-1.89831767562679));
#40239=CARTESIAN_POINT('Ctrl Pts',(-9.182805971501,-2.78631454692713,-3.0742153558314));
#40240=CARTESIAN_POINT('Ctrl Pts',(-9.11664825425829,-1.59601266230262,
-3.60167467690866));
#40241=CARTESIAN_POINT('Ctrl Pts',(-9.05049053701558,-0.405710777678086,
-4.12913399798593));
#40242=CARTESIAN_POINT('Ctrl Pts',(-8.98433281977287,1.0719340584143,-4.00815495993591));
#40243=CARTESIAN_POINT('Ctrl Pts',(-8.91817510253016,2.16059047448068,-3.29411075984077));
#40244=CARTESIAN_POINT('Ctrl Pts',(-8.85201738528746,3.249246890547,-2.58006655974566));
#40245=CARTESIAN_POINT('Ctrl Pts',(-8.78585966804475,3.94891488658736,-1.27295719760559));
#40246=CARTESIAN_POINT('Ctrl Pts',(-8.71970195080204,3.93935010902385,0.0289415799351118));
#40247=CARTESIAN_POINT('Ctrl Pts',(-8.65354423355933,3.92978533146034,1.33084035747585));
#40248=CARTESIAN_POINT('Ctrl Pts',(-8.58738651631661,3.21098778029283,2.62752855041718));
#40249=CARTESIAN_POINT('Ctrl Pts',(-8.5212287990739,2.1119575790511,3.32550027526747));
#40250=CARTESIAN_POINT('Ctrl Pts',(-8.45507108183119,1.01292737780934,4.02347200011778));
#40251=CARTESIAN_POINT('Ctrl Pts',(-8.38891336458848,-0.466335473506701,
4.12272725687701));
#40252=CARTESIAN_POINT('Ctrl Pts',(-8.32275564734577,-1.64875902323899,
3.57783601913271));
#40253=CARTESIAN_POINT('Ctrl Pts',(-8.25659793010306,-2.83118257297127,
3.0329447813884));
#40254=CARTESIAN_POINT('Ctrl Pts',(-8.19044021286035,-3.71676682111984,
1.84390704914054));
#40255=CARTESIAN_POINT('Ctrl Pts',(-8.12428249561764,-3.90017186834352,
0.554956118893427));
#40256=CARTESIAN_POINT('Ctrl Pts',(-8.1149095044234,-3.92615604621803,0.372342113717156));
#40257=CARTESIAN_POINT('Ctrl Pts',(-8.10553651322916,-3.93804592913002,
0.187722628912043));
#40258=CARTESIAN_POINT('Ctrl Pts',(-8.09616352203492,-3.93651676133011,
0.00290543094219859));
#40259=CARTESIAN_POINT('Origin',(-27.25,0.,0.));
#40260=CARTESIAN_POINT('',(-6.66283647796508,-3.92707662061414,0.0014756693134238));
#40261=CARTESIAN_POINT('',(-6.84616352203492,-3.92693618395205,0.00127148827395828));
#40262=CARTESIAN_POINT('',(-27.25,-3.933,-4.81653586104654E-16));
#40263=CARTESIAN_POINT('Ctrl Pts',(-6.66283647796508,-3.92707662061414,
0.0014756693134238));
#40264=CARTESIAN_POINT('Ctrl Pts',(-6.69125337156219,-3.92897796572974,
0.565237947566541));
#40265=CARTESIAN_POINT('Ctrl Pts',(-6.7196702651593,-3.81563262730524,1.12827119920084));
#40266=CARTESIAN_POINT('Ctrl Pts',(-6.74808715875641,-3.58326313671216,
1.63693101554719));
#40267=CARTESIAN_POINT('Ctrl Pts',(-6.81424487599912,-3.04228088606765,
2.82114814989274));
#40268=CARTESIAN_POINT('Ctrl Pts',(-6.88040259324183,-1.85617505344194,
3.71065547367904));
#40269=CARTESIAN_POINT('Ctrl Pts',(-6.94656031048454,-0.567836978435915,
3.8983174604557));
#40270=CARTESIAN_POINT('Ctrl Pts',(-7.01271802772725,0.720501096570151,
4.08597944723238));
#40271=CARTESIAN_POINT('Ctrl Pts',(-7.07887574496995,2.11107141395647,3.57179609699945));
#40272=CARTESIAN_POINT('Ctrl Pts',(-7.14503346221267,2.96739739495242,2.59111376766883));
#40273=CARTESIAN_POINT('Ctrl Pts',(-7.21119117945538,3.82372337594836,1.61043143833821));
#40274=CARTESIAN_POINT('Ctrl Pts',(-7.27734889669809,4.14580502055382,0.1632501299099));
#40275=CARTESIAN_POINT('Ctrl Pts',(-7.3435066139408,3.78622265449433,-1.0880422175491));
#40276=CARTESIAN_POINT('Ctrl Pts',(-7.40966433118351,3.42664028843486,-2.33933456500806));
#40277=CARTESIAN_POINT('Ctrl Pts',(-7.47582204842623,2.38539391171046,-3.39473795149777));
#40278=CARTESIAN_POINT('Ctrl Pts',(-7.54197976566894,1.13907138415888,-3.77118472609928));
#40279=CARTESIAN_POINT('Ctrl Pts',(-7.60813748291165,-0.1072511433927,-4.14763150070078));
#40280=CARTESIAN_POINT('Ctrl Pts',(-7.67429520015435,-1.5586498217715,-3.84512166341409));
#40281=CARTESIAN_POINT('Ctrl Pts',(-7.74045291739706,-2.5508063826392,-3.00211669574342));
#40282=CARTESIAN_POINT('Ctrl Pts',(-7.79791410425306,-3.41254248706492,
-2.26992598562329));
#40283=CARTESIAN_POINT('Ctrl Pts',(-7.85537529110907,-3.92783712225298,
-1.12999844138859));
#40284=CARTESIAN_POINT('Ctrl Pts',(-7.91283647796508,-3.93687099541924,
0.00275879756119139));
#40285=CARTESIAN_POINT('Ctrl Pts',(-8.09616352203492,-3.93651676133011,
0.00290543094219859));
#40286=CARTESIAN_POINT('Ctrl Pts',(-8.03937879598645,-3.92725254963928,
-1.1167791754208));
#40287=CARTESIAN_POINT('Ctrl Pts',(-7.98259406993798,-3.42546314938591,
-2.24372053308702));
#40288=CARTESIAN_POINT('Ctrl Pts',(-7.92580934388951,-2.58129701731398,
-2.97594062523454));
#40289=CARTESIAN_POINT('Ctrl Pts',(-7.8596516266468,-1.59779127276193,-3.82902231086908));
#40290=CARTESIAN_POINT('Ctrl Pts',(-7.79349390940409,-0.149553937359015,
-4.1463215538918));
#40291=CARTESIAN_POINT('Ctrl Pts',(-7.72733619216138,1.10054369575526,-3.78260762837605));
#40292=CARTESIAN_POINT('Ctrl Pts',(-7.66117847491867,2.35064132886953,-3.4188937028603));
#40293=CARTESIAN_POINT('Ctrl Pts',(-7.59502075767596,3.40259925969511,-2.3741666088061));
#40294=CARTESIAN_POINT('Ctrl Pts',(-7.52886304043325,3.77492685345232,-1.12660736177254));
#40295=CARTESIAN_POINT('Ctrl Pts',(-7.46270532319054,4.14725444720951,0.120951885260985));
#40296=CARTESIAN_POINT('Ctrl Pts',(-7.39654760594783,3.83995170389831,1.57134328527392));
#40297=CARTESIAN_POINT('Ctrl Pts',(-7.33038988870512,2.99367386134789,2.56070961032244));
#40298=CARTESIAN_POINT('Ctrl Pts',(-7.26423217146242,2.14739601879745,3.55007593537099));
#40299=CARTESIAN_POINT('Ctrl Pts',(-7.19807445421971,0.762143077007797,
4.07841718545519));
#40300=CARTESIAN_POINT('Ctrl Pts',(-7.131916736977,-0.528042196028415,3.90390680418073));
#40301=CARTESIAN_POINT('Ctrl Pts',(-7.06575901973429,-1.81822746906463,
3.72939642290628));
#40302=CARTESIAN_POINT('Ctrl Pts',(-6.99960130249158,-3.01334507334736,
2.85203441027317));
#40303=CARTESIAN_POINT('Ctrl Pts',(-6.93344358524887,-3.56637890009438,
1.67339727425315));
#40304=CARTESIAN_POINT('Ctrl Pts',(-6.90435023084422,-3.80957969041612,
1.15508271713341));
#40305=CARTESIAN_POINT('Ctrl Pts',(-6.87525687643957,-3.92861002670579,
0.578505562252523));
#40306=CARTESIAN_POINT('Ctrl Pts',(-6.84616352203492,-3.92693618395205,
0.00127148827395828));
#40307=CARTESIAN_POINT('Origin',(-27.25,0.,0.));
#40308=CARTESIAN_POINT('',(-5.41283647796509,-3.93146821322483,-0.00353098110087657));
#40309=CARTESIAN_POINT('',(-5.59616352203493,-3.9318578232019,-0.00356758979283532));
#40310=CARTESIAN_POINT('',(-27.25,-3.933,-4.81653586104654E-16));
#40311=CARTESIAN_POINT('Ctrl Pts',(-5.41283647796509,-3.93146821322483,
-0.00353098110087657));
#40312=CARTESIAN_POINT('Ctrl Pts',(-5.46097373477261,-3.9231618876001,0.948778731502717));
#40313=CARTESIAN_POINT('Ctrl Pts',(-5.50911099158013,-3.57517179997445,
1.90652852351159));
#40314=CARTESIAN_POINT('Ctrl Pts',(-5.55724824838764,-2.94634760568305,
2.61502459708094));
#40315=CARTESIAN_POINT('Ctrl Pts',(-5.62340596563035,-2.0821194381401,3.58875027260494));
#40316=CARTESIAN_POINT('Ctrl Pts',(-5.68956368287305,-0.687436696378754,
4.09167211074258));
#40317=CARTESIAN_POINT('Ctrl Pts',(-5.75572140011577,0.599341746962865,
3.89359824929388));
#40318=CARTESIAN_POINT('Ctrl Pts',(-5.82187911735848,1.88612019030448,3.69552438784518));
#40319=CARTESIAN_POINT('Ctrl Pts',(-5.88803683460119,3.06499433522633,2.79645482681015));
#40320=CARTESIAN_POINT('Ctrl Pts',(-5.95419455184391,3.59638285089867,1.60790181487245));
#40321=CARTESIAN_POINT('Ctrl Pts',(-6.02035226908662,4.127771366571,0.419348802934788));
#40322=CARTESIAN_POINT('Ctrl Pts',(-6.08650998632932,4.01167425299381,-1.0586876599056));
#40323=CARTESIAN_POINT('Ctrl Pts',(-6.15266770357203,3.30123020634185,-2.1496969510498));
#40324=CARTESIAN_POINT('Ctrl Pts',(-6.21882542081474,2.59078615968987,-3.24070624219403));
#40325=CARTESIAN_POINT('Ctrl Pts',(-6.28498313805745,1.28599517996311,-3.94468836164213));
#40326=CARTESIAN_POINT('Ctrl Pts',(-6.35114085530016,-0.0159281307202408,
-3.93942434261913));
#40327=CARTESIAN_POINT('Ctrl Pts',(-6.41729857254287,-1.31785144140355,
-3.93416032359614));
#40328=CARTESIAN_POINT('Ctrl Pts',(-6.48345628978557,-2.61690708304341,
-3.21965016610209));
#40329=CARTESIAN_POINT('Ctrl Pts',(-6.54961400702828,-3.31850556953169,
-2.12293161490267));
#40330=CARTESIAN_POINT('Ctrl Pts',(-6.58735483067388,-3.71874466259825,
-1.49728938970574));
#40331=CARTESIAN_POINT('Ctrl Pts',(-6.62509565431948,-3.92455142093134,
-0.747263901705643));
#40332=CARTESIAN_POINT('Ctrl Pts',(-6.66283647796508,-3.92707662061414,
0.0014756693134238));
#40333=CARTESIAN_POINT('Ctrl Pts',(-6.84616352203492,-3.92693618395205,
0.00127148827395828));
#40334=CARTESIAN_POINT('Ctrl Pts',(-6.80909915919686,-3.92480374111665,
-0.734113399383333));
#40335=CARTESIAN_POINT('Ctrl Pts',(-6.77203479635879,-3.72676527488361,
-1.47056448382967));
#40336=CARTESIAN_POINT('Ctrl Pts',(-6.73497043352073,-3.33998801353544,
-2.08897031236778));
#40337=CARTESIAN_POINT('Ctrl Pts',(-6.66881271627802,-2.64961325101818,
-3.19278850356176));
#40338=CARTESIAN_POINT('Ctrl Pts',(-6.60265499903531,-1.35791367677233,
-3.92051262654278));
#40339=CARTESIAN_POINT('Ctrl Pts',(-6.5364972817926,-0.0561118385083373,
-3.93905678533495));
#40340=CARTESIAN_POINT('Ctrl Pts',(-6.47033956454989,1.24568999975573,-3.95760094412711));
#40341=CARTESIAN_POINT('Ctrl Pts',(-6.40418184730719,2.55759410203788,-3.26696513873041));
#40342=CARTESIAN_POINT('Ctrl Pts',(-6.33802413006447,3.27913012587421,-2.18325960758356));
#40343=CARTESIAN_POINT('Ctrl Pts',(-6.27186641282177,4.00066614971047,-1.09955407643679));
#40344=CARTESIAN_POINT('Ctrl Pts',(-6.20570869557906,4.13183409510091,0.377221180460019));
#40345=CARTESIAN_POINT('Ctrl Pts',(-6.13955097833635,3.61259721016315,1.57113280585333));
#40346=CARTESIAN_POINT('Ctrl Pts',(-6.07339326109364,3.09336032522536,2.76504443124672));
#40347=CARTESIAN_POINT('Ctrl Pts',(-6.00723554385092,1.92371860995926,3.6760924251366));
#40348=CARTESIAN_POINT('Ctrl Pts',(-5.94107782660821,0.639027628913517,
3.8872819020486));
#40349=CARTESIAN_POINT('Ctrl Pts',(-5.8749201093655,-0.645663352132228,
4.09847137896061));
#40350=CARTESIAN_POINT('Ctrl Pts',(-5.80876239212279,-2.04540359895766,
3.60980233889474));
#40351=CARTESIAN_POINT('Ctrl Pts',(-5.74260467488008,-2.91951937334548,
2.64494300982427));
#40352=CARTESIAN_POINT('Ctrl Pts',(-5.69379095726503,-3.56447573448,1.93303255114411));
#40353=CARTESIAN_POINT('Ctrl Pts',(-5.64497723964998,-3.92327908267579,
0.961881335847518));
#40354=CARTESIAN_POINT('Ctrl Pts',(-5.59616352203493,-3.9318578232019,-0.00356758979283532));
#40355=CARTESIAN_POINT('Origin',(-27.25,0.,0.));
#40356=CARTESIAN_POINT('',(-4.16283647796509,-3.93933553009238,0.000621493119071417));
#40357=CARTESIAN_POINT('',(-4.34616352203494,-3.93922419965025,0.000863830554008869));
#40358=CARTESIAN_POINT('',(-27.25,-3.933,-4.81653586104654E-16));
#40359=CARTESIAN_POINT('Ctrl Pts',(-4.16283647796509,-3.93933553009238,
0.000621493119071417));
#40360=CARTESIAN_POINT('Ctrl Pts',(-4.1645363807403,-3.93940906456347,0.0340770639088575));
#40361=CARTESIAN_POINT('Ctrl Pts',(-4.16623628351551,-3.93901973837612,
0.0675308795071106));
#40362=CARTESIAN_POINT('Ctrl Pts',(-4.16793618629071,-3.93816230537414,
0.100972693060727));
#40363=CARTESIAN_POINT('Ctrl Pts',(-4.23409390353343,-3.90479227331878,
1.40247891884733));
#40364=CARTESIAN_POINT('Ctrl Pts',(-4.30025162077614,-3.16240332696561,
2.68580622394492));
#40365=CARTESIAN_POINT('Ctrl Pts',(-4.36640933801885,-2.05079357198834,
3.36356412049544));
#40366=CARTESIAN_POINT('Ctrl Pts',(-4.43256705526156,-0.939183817011137,
4.04132201704592));
#40367=CARTESIAN_POINT('Ctrl Pts',(-4.49872477250427,0.541646746590158,
4.11351050504943));
#40368=CARTESIAN_POINT('Ctrl Pts',(-4.56488248974698,1.71390860469547,3.54708826403145));
#40369=CARTESIAN_POINT('Ctrl Pts',(-4.63104020698969,2.88617046280078,2.98066602301347));
#40370=CARTESIAN_POINT('Ctrl Pts',(-4.69719792423241,3.74986361541014,1.77563305297397));
#40371=CARTESIAN_POINT('Ctrl Pts',(-4.76335564147512,3.90966791844257,0.483543814157597));
#40372=CARTESIAN_POINT('Ctrl Pts',(-4.82951335871783,4.069472221475,-0.808545424658813));
#40373=CARTESIAN_POINT('Ctrl Pts',(-4.89567107596053,3.52538767493053,-2.18769093225205));
#40374=CARTESIAN_POINT('Ctrl Pts',(-4.96182879320324,2.52644668226425,-3.02264536789066));
#40375=CARTESIAN_POINT('Ctrl Pts',(-5.02798651044595,1.527505689598,-3.85759980352923));
#40376=CARTESIAN_POINT('Ctrl Pts',(-5.09414422768866,0.0737082508099615,
-4.14836316721312));
#40377=CARTESIAN_POINT('Ctrl Pts',(-5.16030194493137,-1.16952943056686,
-3.76185044461622));
#40378=CARTESIAN_POINT('Ctrl Pts',(-5.22645966217409,-2.41276711194375,
-3.3753377220193));
#40379=CARTESIAN_POINT('Ctrl Pts',(-5.2926173794168,-3.44544503590944,-2.3115489131415));
#40380=CARTESIAN_POINT('Ctrl Pts',(-5.35877509665951,-3.79489720122999,
-1.05738975224741));
#40381=CARTESIAN_POINT('Ctrl Pts',(-5.37679555709471,-3.89008320796671,
-0.715773891237398));
#40382=CARTESIAN_POINT('Ctrl Pts',(-5.3948160175299,-3.93457773425301,-0.360033628658111));
#40383=CARTESIAN_POINT('Ctrl Pts',(-5.41283647796509,-3.93146821322483,
-0.00353098110087657));
#40384=CARTESIAN_POINT('Ctrl Pts',(-5.59616352203493,-3.9318578232019,-0.00356758979283532));
#40385=CARTESIAN_POINT('Ctrl Pts',(-5.57881952240727,-3.93490593508029,
-0.34660120052666));
#40386=CARTESIAN_POINT('Ctrl Pts',(-5.56147552277961,-3.89373988480933,
-0.688914924782032));
#40387=CARTESIAN_POINT('Ctrl Pts',(-5.54413152315195,-3.80548566654496,
-1.01862443430826));
#40388=CARTESIAN_POINT('Ctrl Pts',(-5.47797380590924,-3.46884488340641,
-2.27628293129547));
#40389=CARTESIAN_POINT('Ctrl Pts',(-5.41181608866654,-2.44707201517901,
-3.35055030719482));
#40390=CARTESIAN_POINT('Ctrl Pts',(-5.34565837142382,-1.20784172112326,
-3.74972469298905));
#40391=CARTESIAN_POINT('Ctrl Pts',(-5.27950065418112,0.0313885729323832,
-4.14889907878324));
#40392=CARTESIAN_POINT('Ctrl Pts',(-5.21334293693841,1.48807629281634,-3.87298047447244));
#40393=CARTESIAN_POINT('Ctrl Pts',(-5.1471852196957,2.49548232805611,-3.04825931428975));
#40394=CARTESIAN_POINT('Ctrl Pts',(-5.08102750245299,3.50288836329594,-2.22353815410701));
#40395=CARTESIAN_POINT('Ctrl Pts',(-5.01486978521028,4.06101271389155,-0.850014438052321));
#40396=CARTESIAN_POINT('Ctrl Pts',(-4.94871206796757,3.91439682990473,0.443637638205326));
#40397=CARTESIAN_POINT('Ctrl Pts',(-4.88255435072487,3.76778094591791,1.73728971446297));
#40398=CARTESIAN_POINT('Ctrl Pts',(-4.81639663348215,2.91642482734867,2.95107015092358));
#40399=CARTESIAN_POINT('Ctrl Pts',(-4.75023891623944,1.7500018493998,3.52942069236006));
#40400=CARTESIAN_POINT('Ctrl Pts',(-4.68408119899673,0.583578871450859,
4.10777123379658));
#40401=CARTESIAN_POINT('Ctrl Pts',(-4.61792348175402,-0.897910965877739,
4.05069188020889));
#40402=CARTESIAN_POINT('Ctrl Pts',(-4.5517657645113,-2.01637639847237,3.384308366267));
#40403=CARTESIAN_POINT('Ctrl Pts',(-4.48560804726859,-3.13484183106693,
2.71792485232515));
#40404=CARTESIAN_POINT('Ctrl Pts',(-4.41945033002589,-3.89028285892757,
1.44223717802918));
#40405=CARTESIAN_POINT('Ctrl Pts',(-4.35329261278318,-3.93692731033631,
0.141139100778367));
#40406=CARTESIAN_POINT('Ctrl Pts',(-4.35091624920043,-3.93860276378731,
0.0944040830477024));
#40407=CARTESIAN_POINT('Ctrl Pts',(-4.34853988561769,-3.93936371164798,
0.0476362802326757));
#40408=CARTESIAN_POINT('Ctrl Pts',(-4.34616352203494,-3.93922419965025,
0.000863830554008869));
#40409=CARTESIAN_POINT('Origin',(-27.25,0.,0.));
#40410=CARTESIAN_POINT('',(-2.91283647796509,-3.92964797513088,0.00314259250936713));
#40411=CARTESIAN_POINT('',(-3.09616352203493,-3.9293213278247,0.00302737416568081));
#40412=CARTESIAN_POINT('',(-27.25,-3.933,-4.81653586104654E-16));
#40413=CARTESIAN_POINT('Ctrl Pts',(-2.91283647796509,-3.92964797513088,
0.00314259250936713));
#40414=CARTESIAN_POINT('Ctrl Pts',(-2.93425674395071,-3.93282742473341,
0.427401276174971));
#40415=CARTESIAN_POINT('Ctrl Pts',(-2.95567700993633,-3.86952908002031,
0.850736746834505));
#40416=CARTESIAN_POINT('Ctrl Pts',(-2.97709727592195,-3.7357245118254,1.25047143256818));
#40417=CARTESIAN_POINT('Ctrl Pts',(-3.04325499316466,-3.32246144616761,
2.48507488374048));
#40418=CARTESIAN_POINT('Ctrl Pts',(-3.10941271040737,-2.23662642002933,
3.49454606427628));
#40419=CARTESIAN_POINT('Ctrl Pts',(-3.17557042765008,-0.97521532047094,
3.81684074856203));
#40420=CARTESIAN_POINT('Ctrl Pts',(-3.24172814489279,0.286195779087454,
4.13913543284778));
#40421=CARTESIAN_POINT('Ctrl Pts',(-3.3078858621355,1.72318295206596,3.77425362088349));
#40422=CARTESIAN_POINT('Ctrl Pts',(-3.37404357937821,2.67802389252845,2.88920509315637));
#40423=CARTESIAN_POINT('Ctrl Pts',(-3.44020129662092,3.63286483299093,2.00415656542924));
#40424=CARTESIAN_POINT('Ctrl Pts',(-3.50635901386363,4.10555954093739,0.598941321939292));
#40425=CARTESIAN_POINT('Ctrl Pts',(-3.57251673110634,3.87975154828102,-0.683260987411258));
#40426=CARTESIAN_POINT('Ctrl Pts',(-3.63867444834905,3.65394355562464,-1.96546329676181));
#40427=CARTESIAN_POINT('Ctrl Pts',(-3.70483216559175,2.72963286236543,-3.12465267197295));
#40428=CARTESIAN_POINT('Ctrl Pts',(-3.77098988283446,1.52988472539395,-3.63025765599397));
#40429=CARTESIAN_POINT('Ctrl Pts',(-3.83714760007717,0.330136588422467,
-4.13586264001499));
#40430=CARTESIAN_POINT('Ctrl Pts',(-3.90330531731989,-1.14504899226128,
-3.98788323284587));
#40431=CARTESIAN_POINT('Ctrl Pts',(-3.9694630345626,-2.22046622372429,-3.25405095602352));
#40432=CARTESIAN_POINT('Ctrl Pts',(-4.0339208490301,-3.26825093078253,-2.53907428026934));
#40433=CARTESIAN_POINT('Ctrl Pts',(-4.09837866349759,-3.93654721104028,
-1.26796457328689));
#40434=CARTESIAN_POINT('Ctrl Pts',(-4.16283647796509,-3.93933553009238,
0.000621493119071417));
#40435=CARTESIAN_POINT('Ctrl Pts',(-4.34616352203494,-3.93922419965025,
0.000863830554008869));
#40436=CARTESIAN_POINT('Ctrl Pts',(-4.28238216837498,-3.93547971200863,
-1.2545038985929));
#40437=CARTESIAN_POINT('Ctrl Pts',(-4.21860081471501,-3.28306189041179,
-2.51321913568449));
#40438=CARTESIAN_POINT('Ctrl Pts',(-4.15481946105504,-2.25354393302045,
-3.23123144326866));
#40439=CARTESIAN_POINT('Ctrl Pts',(-4.08866174381234,-1.1856682293391,-3.9759954298592));
#40440=CARTESIAN_POINT('Ctrl Pts',(-4.02250402656963,0.287931052980419,
-4.13901492283474));
#40441=CARTESIAN_POINT('Ctrl Pts',(-3.95634630932692,1.49277422283225,-3.64567442693553));
#40442=CARTESIAN_POINT('Ctrl Pts',(-3.89018859208421,2.69761739268421,-3.15233393103625));
#40443=CARTESIAN_POINT('Ctrl Pts',(-3.8240308748415,3.63370445006837,-2.00263344626206));
#40444=CARTESIAN_POINT('Ctrl Pts',(-3.75787315759879,3.87257991587189,-0.722801261257757));
#40445=CARTESIAN_POINT('Ctrl Pts',(-3.69171544035608,4.11145538167539,0.557030923746436));
#40446=CARTESIAN_POINT('Ctrl Pts',(-3.62555772311337,3.65311925589831,1.96699480898077));
#40447=CARTESIAN_POINT('Ctrl Pts',(-3.55940000587066,2.70735609581649,2.86173721461466));
#40448=CARTESIAN_POINT('Ctrl Pts',(-3.49324228862795,1.76159293573465,3.75647962024858));
#40449=CARTESIAN_POINT('Ctrl Pts',(-3.42708457138524,0.328402741348056,
4.13600054628211));
#40450=CARTESIAN_POINT('Ctrl Pts',(-3.36092685414253,-0.936230363935897,
3.82658982223686));
#40451=CARTESIAN_POINT('Ctrl Pts',(-3.29476913689982,-2.20086346921985,
3.51717909819162));
#40452=CARTESIAN_POINT('Ctrl Pts',(-3.22861141965711,-3.29693948540113,
2.51883672406761));
#40453=CARTESIAN_POINT('Ctrl Pts',(-3.16245370241439,-3.722774613227,1.28851304686882));
#40454=CARTESIAN_POINT('Ctrl Pts',(-3.14035697562124,-3.86500386282424,
0.877584023086522));
#40455=CARTESIAN_POINT('Ctrl Pts',(-3.11826024882808,-3.93246338668909,
0.440775977735576));
#40456=CARTESIAN_POINT('Ctrl Pts',(-3.09616352203493,-3.9293213278247,0.00302737416568081));
#40457=CARTESIAN_POINT('Origin',(-27.25,0.,0.));
#40458=CARTESIAN_POINT('',(-1.66283647796509,-3.92810494057017,-0.00240077655339843));
#40459=CARTESIAN_POINT('',(-1.84616352203496,-3.92834846924785,-0.00256498101517192));
#40460=CARTESIAN_POINT('',(-27.25,-3.933,-4.81653586104654E-16));
#40461=CARTESIAN_POINT('Ctrl Pts',(-1.66283647796509,-3.92810494057017,
-0.00240077655339843));
#40462=CARTESIAN_POINT('Ctrl Pts',(-1.70397710716111,-3.92354275555459,
0.813259782426832));
#40463=CARTESIAN_POINT('Ctrl Pts',(-1.74511773635714,-3.67602106528321,
1.63145161923944));
#40464=CARTESIAN_POINT('Ctrl Pts',(-1.78625836555316,-3.20534629633937,
2.29019815317242));
#40465=CARTESIAN_POINT('Ctrl Pts',(-1.85241608279587,-2.44846024754571,
3.34951999093285));
#40466=CARTESIAN_POINT('Ctrl Pts',(-1.91857380003859,-1.11451276938518,
3.99652515830297));
#40467=CARTESIAN_POINT('Ctrl Pts',(-1.9847315172813,0.185965708862303,3.93506573455426));
#40468=CARTESIAN_POINT('Ctrl Pts',(-2.05088923452401,1.48644418710979,3.87360631080555));
#40469=CARTESIAN_POINT('Ctrl Pts',(-2.11704695176672,2.75345366544434,3.10368229593785));
#40470=CARTESIAN_POINT('Ctrl Pts',(-2.18320466900943,3.40705712250568,1.97769894516902));
#40471=CARTESIAN_POINT('Ctrl Pts',(-2.24936238625214,4.06066057956705,0.851715594400124));
#40472=CARTESIAN_POINT('Ctrl Pts',(-2.31552010349485,4.10085801535535,-0.630327092269794));
#40473=CARTESIAN_POINT('Ctrl Pts',(-2.38167782073757,3.50925872819166,-1.79008694485165));
#40474=CARTESIAN_POINT('Ctrl Pts',(-2.44783553798027,2.91765944102804,-2.94984679743337));
#40475=CARTESIAN_POINT('Ctrl Pts',(-2.51399325522299,1.69426343091233,-3.78732381592697));
#40476=CARTESIAN_POINT('Ctrl Pts',(-2.58015097246569,0.399025891082152,
-3.91919609647393));
#40477=CARTESIAN_POINT('Ctrl Pts',(-2.6463086897084,-0.896211648748102,
-4.0510683770209));
#40478=CARTESIAN_POINT('Ctrl Pts',(-2.71246640695111,-2.26329071829293,
-3.47733591962131));
#40479=CARTESIAN_POINT('Ctrl Pts',(-2.77862412419382,-3.07648470047672,
-2.4606018300171));
#40480=CARTESIAN_POINT('Ctrl Pts',(-2.82336157545091,-3.62638617315059,
-1.77306160537151));
#40481=CARTESIAN_POINT('Ctrl Pts',(-2.868099026708,-3.92300751269621,-0.882945945963138));
#40482=CARTESIAN_POINT('Ctrl Pts',(-2.91283647796509,-3.92964797513088,
0.00314259250936713));
#40483=CARTESIAN_POINT('Ctrl Pts',(-3.09616352203493,-3.9293213278247,0.00302737416568081));
#40484=CARTESIAN_POINT('Ctrl Pts',(-3.05210253158537,-3.92305604578036,
-0.869845663626177));
#40485=CARTESIAN_POINT('Ctrl Pts',(-3.00804154113582,-3.63607483546347,
-1.74645841465561));
#40486=CARTESIAN_POINT('Ctrl Pts',(-2.96398055068627,-3.10142389777848,
-2.42909178207749));
#40487=CARTESIAN_POINT('Ctrl Pts',(-2.89782283344356,-2.29864381503363,
-3.45406795355147));
#40488=CARTESIAN_POINT('Ctrl Pts',(-2.83166511620085,-0.937489410073432,
-4.04171531622592));
#40489=CARTESIAN_POINT('Ctrl Pts',(-2.76550739895814,0.359026369870962,
-3.92306223857118));
#40490=CARTESIAN_POINT('Ctrl Pts',(-2.69934968171543,1.65554214981543,-3.80440916091644));
#40491=CARTESIAN_POINT('Ctrl Pts',(-2.63319196447272,2.88741930474417,-2.97945564293242));
#40492=CARTESIAN_POINT('Ctrl Pts',(-2.56703424723,3.49081711581239,-1.82579060500368));
#40493=CARTESIAN_POINT('Ctrl Pts',(-2.50087652998729,4.09421492688058,-0.672125567075004));
#40494=CARTESIAN_POINT('Ctrl Pts',(-2.43471881274459,4.06913339408844,0.8102509907982));
#40495=CARTESIAN_POINT('Ctrl Pts',(-2.36856109550188,3.42705147522404,1.94284242960063));
#40496=CARTESIAN_POINT('Ctrl Pts',(-2.30240337825917,2.78496955635964,3.07543386840307));
#40497=CARTESIAN_POINT('Ctrl Pts',(-2.23624566101646,1.52588725142289,3.85824018813459));
#40498=CARTESIAN_POINT('Ctrl Pts',(-2.17008794377375,0.226099966689285,
3.93296294841805));
#40499=CARTESIAN_POINT('Ctrl Pts',(-2.10393022653105,-1.07368731804432,
4.00768570870152));
#40500=CARTESIAN_POINT('Ctrl Pts',(-2.03777250928834,-2.41417958257486,
3.37432490953694));
#40501=CARTESIAN_POINT('Ctrl Pts',(-1.97161479204563,-3.18182539675517,
2.32277727332773));
#40502=CARTESIAN_POINT('Ctrl Pts',(-1.92979770204207,-3.66704035640476,
1.65811313467455));
#40503=CARTESIAN_POINT('Ctrl Pts',(-1.88798061203852,-3.92338745106363,
0.826371887481848));
#40504=CARTESIAN_POINT('Ctrl Pts',(-1.84616352203496,-3.92834846924785,
-0.00256498101517192));
#40505=CARTESIAN_POINT('Origin',(-27.25,0.,0.));
#40506=CARTESIAN_POINT('',(-0.41283647796511,-3.93929521061115,-0.00160796147817999));
#40507=CARTESIAN_POINT('',(-0.596163522034944,-3.93875600852084,-0.00157175874070594));
#40508=CARTESIAN_POINT('',(-27.25,-3.933,-4.81653586104654E-16));
#40509=CARTESIAN_POINT('Ctrl Pts',(-0.41283647796511,-3.93929521061115,
-0.00160796147817999));
#40510=CARTESIAN_POINT('Ctrl Pts',(-0.473697470371537,-3.93274620403603,
1.19707520163202));
#40511=CARTESIAN_POINT('Ctrl Pts',(-0.534558462777964,-3.34481231109049,
2.40115562852338));
#40512=CARTESIAN_POINT('Ctrl Pts',(-0.59541945518439,-2.39319605116334,
3.12878034020633));
#40513=CARTESIAN_POINT('Ctrl Pts',(-0.661577172427097,-1.35876074279041,
3.91973014287904));
#40514=CARTESIAN_POINT('Ctrl Pts',(-0.727734889669808,0.105414000682263,
4.14768369252194));
#40515=CARTESIAN_POINT('Ctrl Pts',(-0.793892606912517,1.33061187712945,
3.70791565939382));
#40516=CARTESIAN_POINT('Ctrl Pts',(-0.860050324155229,2.55580975357671,
3.26814762626567));
#40517=CARTESIAN_POINT('Ctrl Pts',(-0.926208041397931,3.54203076299841,
2.16065801036661));
#40518=CARTESIAN_POINT('Ctrl Pts',(-0.992365758640646,3.83711969094379,
0.892555614996963));
#40519=CARTESIAN_POINT('Ctrl Pts',(-1.05852347588335,4.13220861888915,-0.375546780372539));
#40520=CARTESIAN_POINT('Ctrl Pts',(-1.12468119312606,3.73616546535818,-1.80426195521246));
#40521=CARTESIAN_POINT('Ctrl Pts',(-1.19083891036877,2.83065587439165,-2.73975879600272));
#40522=CARTESIAN_POINT('Ctrl Pts',(-1.25699662761148,1.92514628342501,-3.67525563679308));
#40523=CARTESIAN_POINT('Ctrl Pts',(-1.32315434485419,0.510170255022601,
-4.1175341435337));
#40524=CARTESIAN_POINT('Ctrl Pts',(-1.38931206209691,-0.76683039427974,
-3.86410473867316));
#40525=CARTESIAN_POINT('Ctrl Pts',(-1.45546977933961,-2.04383104358194,
-3.61067533381264));
#40526=CARTESIAN_POINT('Ctrl Pts',(-1.52162749658232,-3.18285631378417,
-2.66153801735112));
#40527=CARTESIAN_POINT('Ctrl Pts',(-1.58778521382502,-3.66245663917197,
-1.45115010504507));
#40528=CARTESIAN_POINT('Ctrl Pts',(-1.61280230187171,-3.84381422022983,
-0.993450198899252));
#40529=CARTESIAN_POINT('Ctrl Pts',(-1.6378193899184,-3.93087914666402,-0.498393483008929));
#40530=CARTESIAN_POINT('Ctrl Pts',(-1.66283647796509,-3.92810494057017,
-0.00240077655339843));
#40531=CARTESIAN_POINT('Ctrl Pts',(-1.84616352203496,-3.92834846924785,
-0.00256498101517192));
#40532=CARTESIAN_POINT('Ctrl Pts',(-1.8218228947958,-3.93123614733207,-0.485067310066915));
#40533=CARTESIAN_POINT('Ctrl Pts',(-1.79748226755664,-3.84895176851133,
-0.966619488238375));
#40534=CARTESIAN_POINT('Ctrl Pts',(-1.77314164031748,-3.67705446577845,
-1.41371880629667));
#40535=CARTESIAN_POINT('Ctrl Pts',(-1.70698392307477,-3.20983835679131,
-2.62893277645775));
#40536=CARTESIAN_POINT('Ctrl Pts',(-1.64082620583206,-2.08060677498703,
-3.589626243526));
#40537=CARTESIAN_POINT('Ctrl Pts',(-1.57466848858935,-0.806233729792193,
-3.85607466381471));
#40538=CARTESIAN_POINT('Ctrl Pts',(-1.50851077134664,0.468139315402641,
-4.12252308410342));
#40539=CARTESIAN_POINT('Ctrl Pts',(-1.44235305410394,1.88765382398794,-3.69472645761258));
#40540=CARTESIAN_POINT('Ctrl Pts',(-1.37619533686123,2.80261298269254,-2.76850354687877));
#40541=CARTESIAN_POINT('Ctrl Pts',(-1.31003761961852,3.71757214139709,-1.84228063614501));
#40542=CARTESIAN_POINT('Ctrl Pts',(-1.2438799023758,4.12797595022095,-0.41763144116817));
#40543=CARTESIAN_POINT('Ctrl Pts',(-1.17772218513309,3.84592575036428,0.853392939764376));
#40544=CARTESIAN_POINT('Ctrl Pts',(-1.11156446789038,3.5638755505076,2.124417320697));
#40545=CARTESIAN_POINT('Ctrl Pts',(-1.04540675064768,2.58937134197042,3.24181688758541));
#40546=CARTESIAN_POINT('Ctrl Pts',(-0.979249033404965,1.36855410729865,
3.69410247152038));
#40547=CARTESIAN_POINT('Ctrl Pts',(-0.913091316162255,0.147736872626877,
4.14638805545535));
#40548=CARTESIAN_POINT('Ctrl Pts',(-0.846933598919547,-1.3193933881794,
3.93355965643683));
#40549=CARTESIAN_POINT('Ctrl Pts',(-0.780775881676838,-2.36151226423397,
3.15311740810728));
#40550=CARTESIAN_POINT('Ctrl Pts',(-0.719238428462872,-3.33085256573394,
2.42717899389947));
#40551=CARTESIAN_POINT('Ctrl Pts',(-0.657700975248911,-3.93247174430637,
1.21013937735618));
#40552=CARTESIAN_POINT('Ctrl Pts',(-0.596163522034944,-3.93875600852084,
-0.00157175874070594));
#40553=CARTESIAN_POINT('Origin',(-56.8777734492732,0.,0.));
#40554=CARTESIAN_POINT('',(-0.00277344927320074,-3.2279083752853,-0.00131758399470729));
#40555=CARTESIAN_POINT('',(-8.88178419700125E-15,-3.22275,1.66140794472856E-12));
#40556=CARTESIAN_POINT('',(-56.8777734492732,-3.22275,1.66140794472856E-12));
#40557=CARTESIAN_POINT('',(0.,-3.22243683749934,-0.044926504729961));
#40558=CARTESIAN_POINT('Ctrl Pts',(-0.00277344927320076,-3.2279083752853,
-0.00131758399470763));
#40559=CARTESIAN_POINT('Ctrl Pts',(-0.00184896618213632,-3.22798989038041,
-0.01623752199351));
#40560=CARTESIAN_POINT('Ctrl Pts',(-0.000924483091071884,-3.2279614830524,
-0.0311564395318102));
#40561=CARTESIAN_POINT('Ctrl Pts',(-7.44426764155703E-15,-3.22782252806242,
-0.046072952734026));
#40562=CARTESIAN_POINT('Origin',(0.,0.,0.));
#40563=CARTESIAN_POINT('Origin',(-56.8777734492732,0.,0.));
#40564=CARTESIAN_POINT('',(-1.2527734492732,-3.21873892632151,-0.0019672267056687));
#40565=CARTESIAN_POINT('',(-1.00622655072698,-3.22746654626507,-0.00128791901194192));
#40566=CARTESIAN_POINT('',(-56.8777734492732,-3.22275,1.66140794472856E-12));
#40567=CARTESIAN_POINT('Ctrl Pts',(-1.2527734492732,-3.21873892632151,-0.00196722670566859));
#40568=CARTESIAN_POINT('Ctrl Pts',(-1.2277563612265,-3.22101214592218,-0.40838993067981));
#40569=CARTESIAN_POINT('Ctrl Pts',(-1.13658155593709,-2.96100577144116,
-1.88680273286147));
#40570=CARTESIAN_POINT('Ctrl Pts',(-0.979249033404971,-0.741409307439854,
-3.73636822239283));
#40571=CARTESIAN_POINT('Ctrl Pts',(-0.780775881676852,2.73693851524025,
-2.64914239661277));
#40572=CARTESIAN_POINT('Ctrl Pts',(-0.58230272994871,3.7105068394527,0.862979517739233));
#40573=CARTESIAN_POINT('Ctrl Pts',(-0.383829578220586,1.28614089123481,
3.58545256094235));
#40574=CARTESIAN_POINT('Ctrl Pts',(-0.190653151328746,-2.21709352745839,
3.04004312499088));
#40575=CARTESIAN_POINT('Ctrl Pts',(-0.0636344416796209,-3.22254203637332,
0.980898577691776));
#40576=CARTESIAN_POINT('Ctrl Pts',(-0.00277344927320076,-3.2279083752853,
-0.00131758399470763));
#40577=CARTESIAN_POINT('',(-8.88178419700125E-15,-1.09131022003147,3.03235215074946));
#40578=CARTESIAN_POINT('Origin',(0.,0.,0.));
#40579=CARTESIAN_POINT('Ctrl Pts',(-1.00622655072698,-3.22746654626507,
-0.00128791901194189));
#40580=CARTESIAN_POINT('Ctrl Pts',(-1.0016062866982,-3.22785316632397,-0.0758347258874285));
#40581=CARTESIAN_POINT('Ctrl Pts',(-0.930828305426712,-3.19164983838238,
-1.21744274340176));
#40582=CARTESIAN_POINT('Ctrl Pts',(-0.793892606912507,-1.8372343102454,
-3.33679471955611));
#40583=CARTESIAN_POINT('Ctrl Pts',(-0.59541945518438,1.80537864589007,-3.35297192389334));
#40584=CARTESIAN_POINT('Ctrl Pts',(-0.396946303456254,3.79975239553181,
-0.301770123854898));
#40585=CARTESIAN_POINT('Ctrl Pts',(-0.198473151728127,2.30693671058513,
3.02973452897375));
#40586=CARTESIAN_POINT('Ctrl Pts',(-0.0661577172427008,-0.082916802787829,
3.39526186154233));
#40587=CARTESIAN_POINT('Ctrl Pts',(8.88178419700125E-15,-1.09131022003164,
3.0323521507494));
#40588=CARTESIAN_POINT('Origin',(-56.8777734492732,0.,0.));
#40589=CARTESIAN_POINT('',(-2.50277344927319,-3.2200033083786,0.00257508009463239));
#40590=CARTESIAN_POINT('',(-2.25622655072698,-3.21893847680358,-0.00210177792008243));
#40591=CARTESIAN_POINT('',(-56.8777734492732,-3.22275,1.66140794472856E-12));
#40592=CARTESIAN_POINT('Ctrl Pts',(-2.50277344927319,-3.2200033083786,0.00257508009463239));
#40593=CARTESIAN_POINT('Ctrl Pts',(-2.45803599801609,-3.21456202937765,
-0.723497088062683));
#40594=CARTESIAN_POINT('Ctrl Pts',(-2.34714082951628,-2.61207673716788,
-2.53146408727085));
#40595=CARTESIAN_POINT('Ctrl Pts',(-2.17008794377376,0.385834726766185,
-3.78962036336862));
#40596=CARTESIAN_POINT('Ctrl Pts',(-1.97161479204564,3.39323327108378,-1.73090254387995));
#40597=CARTESIAN_POINT('Ctrl Pts',(-1.77314164031749,3.29441840747864,1.91231108576612));
#40598=CARTESIAN_POINT('Ctrl Pts',(-1.57466848858938,0.179807578872998,
3.80496754565549));
#40599=CARTESIAN_POINT('Ctrl Pts',(-1.40121242490793,-2.68602209988967,
2.41495284019006));
#40600=CARTESIAN_POINT('Ctrl Pts',(-1.29391407846921,-3.21500061415274,
0.666395363289895));
#40601=CARTESIAN_POINT('Ctrl Pts',(-1.2527734492732,-3.21873892632151,-0.00196722670566859));
#40602=CARTESIAN_POINT('Ctrl Pts',(-2.25622655072698,-3.21893847680358,
-0.00210177792008253));
#40603=CARTESIAN_POINT('Ctrl Pts',(-2.23188592348779,-3.22130467679004,
-0.397470295833488));
#40604=CARTESIAN_POINT('Ctrl Pts',(-2.14138757900589,-2.97061933829329,
-1.86455399408909));
#40605=CARTESIAN_POINT('Ctrl Pts',(-1.98473151728128,-0.779568879692582,
-3.72858958741861));
#40606=CARTESIAN_POINT('Ctrl Pts',(-1.78625836555316,2.7099356073734,-2.67696366978096));
#40607=CARTESIAN_POINT('Ctrl Pts',(-1.58778521382502,3.71880583993438,0.825163098419798));
#40608=CARTESIAN_POINT('Ctrl Pts',(-1.3893120620969,1.32324257672849,3.57199715958687));
#40609=CARTESIAN_POINT('Ctrl Pts',(-1.19545917439755,-2.19935562265448,
3.06099349809352));
#40610=CARTESIAN_POINT('Ctrl Pts',(-1.06776400394091,-3.22231714059518,
0.99160352870076));
#40611=CARTESIAN_POINT('Ctrl Pts',(-1.00622655072698,-3.22746654626507,
-0.00128791901194189));
#40612=CARTESIAN_POINT('Origin',(-56.8777734492732,0.,0.));
#40613=CARTESIAN_POINT('',(-3.75277344927319,-3.22794141357874,0.00050925933183513));
#40614=CARTESIAN_POINT('',(-3.50622655072697,-3.2197356494399,0.0024806687263787));
#40615=CARTESIAN_POINT('',(-56.8777734492732,-3.22275,1.66140794472856E-12));
#40616=CARTESIAN_POINT('Ctrl Pts',(-3.75277344927319,-3.22794141357874,
0.000509259331835047));
#40617=CARTESIAN_POINT('Ctrl Pts',(-3.68831563480568,-3.22565662964174,
-1.03898622643229));
#40618=CARTESIAN_POINT('Ctrl Pts',(-3.55770010309546,-2.1159939982431,-3.14958145779129));
#40619=CARTESIAN_POINT('Ctrl Pts',(-3.36092685414253,1.47930384451711,-3.51023441585637));
#40620=CARTESIAN_POINT('Ctrl Pts',(-3.16245370241441,3.75147950180274,-0.66067106043193));
#40621=CARTESIAN_POINT('Ctrl Pts',(-2.96398055068628,2.58948341482026,2.79368243000086));
#40622=CARTESIAN_POINT('Ctrl Pts',(-2.76550739895815,-0.942973039578199,
3.69064876067085));
#40623=CARTESIAN_POINT('Ctrl Pts',(-2.61177169848712,-3.0105454903401,1.76848309786626));
#40624=CARTESIAN_POINT('Ctrl Pts',(-2.5241937152588,-3.22260858964133,0.350218017491745));
#40625=CARTESIAN_POINT('Ctrl Pts',(-2.50277344927319,-3.2200033083786,0.00257508009463239));
#40626=CARTESIAN_POINT('Ctrl Pts',(-3.50622655072697,-3.2197356494399,0.00248066872637863));
#40627=CARTESIAN_POINT('Ctrl Pts',(-3.46216556027738,-3.21460179800166,
-0.712762550837853));
#40628=CARTESIAN_POINT('Ctrl Pts',(-3.35194685258509,-2.6263582225274,-2.50961126578718));
#40629=CARTESIAN_POINT('Ctrl Pts',(-3.17557042765007,0.347156461294124,
-3.7933583964979));
#40630=CARTESIAN_POINT('Ctrl Pts',(-2.97709727592195,3.37540367795816,-1.76542632168304));
#40631=CARTESIAN_POINT('Ctrl Pts',(-2.77862412419381,3.31374730129506,1.87860804283756));
#40632=CARTESIAN_POINT('Ctrl Pts',(-2.58015097246569,0.218623351459381,
3.80293227389407));
#40633=CARTESIAN_POINT('Ctrl Pts',(-2.40601844797674,-2.67249830937439,
2.43692429754177));
#40634=CARTESIAN_POINT('Ctrl Pts',(-2.29804364073051,-3.21487335568621,
0.677139588199134));
#40635=CARTESIAN_POINT('Ctrl Pts',(-2.25622655072698,-3.21893847680358,
-0.00210177792008253));
#40636=CARTESIAN_POINT('Origin',(-56.8777734492732,0.,0.));
#40637=CARTESIAN_POINT('',(-5.00277344927319,-3.2214948345208,-0.00289333062281008));
#40638=CARTESIAN_POINT('',(-4.75622655072696,-3.22785018800479,0.000707833695615633));
#40639=CARTESIAN_POINT('',(-56.8777734492732,-3.22275,1.66140794472856E-12));
#40640=CARTESIAN_POINT('Ctrl Pts',(-5.00277344927319,-3.2214948345208,-0.00289333062280996));
#40641=CARTESIAN_POINT('Ctrl Pts',(-4.98475298883799,-3.22404281542441,
-0.295016114100004));
#40642=CARTESIAN_POINT('Ctrl Pts',(-4.90057481116007,-3.05373173874959,
-1.65667814746345));
#40643=CARTESIAN_POINT('Ctrl Pts',(-4.75023891623944,-1.13086255544314,
-3.6374764880366));
#40644=CARTESIAN_POINT('Ctrl Pts',(-4.55176576451131,2.44291753292778,-2.92271094241356));
#40645=CARTESIAN_POINT('Ctrl Pts',(-4.35329261278319,3.78040683298627,0.467556932945782));
#40646=CARTESIAN_POINT('Ctrl Pts',(-4.15481946105505,1.65724351676092,3.42981475460483));
#40647=CARTESIAN_POINT('Ctrl Pts',(-3.95634630932692,-1.98299042591341,
3.25235827122354));
#40648=CARTESIAN_POINT('Ctrl Pts',(-3.8223309720663,-3.21526690679691,1.12218908818911));
#40649=CARTESIAN_POINT('Ctrl Pts',(-3.75447335204839,-3.22800166865545,
0.0279231776543737));
#40650=CARTESIAN_POINT('Ctrl Pts',(-3.75277344927319,-3.22794141357874,
0.000509259331835047));
#40651=CARTESIAN_POINT('Ctrl Pts',(-4.75622655072696,-3.22785018800479,
0.000707833695615589));
#40652=CARTESIAN_POINT('Ctrl Pts',(-4.69244519706697,-3.22478190741881,
-1.02795637914702));
#40653=CARTESIAN_POINT('Ctrl Pts',(-4.56250612616426,-2.1356649716347,-3.12919892137489));
#40654=CARTESIAN_POINT('Ctrl Pts',(-4.36640933801884,1.44342026140034,-3.52514147306206));
#40655=CARTESIAN_POINT('Ctrl Pts',(-4.16793618629072,3.74454502431787,-0.698904068557403));
#40656=CARTESIAN_POINT('Ctrl Pts',(-3.96946303456259,2.61784574945316,2.7671227133945));
#40657=CARTESIAN_POINT('Ctrl Pts',(-3.77098988283447,-0.905276827937616,
3.70007547035483));
#40658=CARTESIAN_POINT('Ctrl Pts',(-3.61657772155592,-3.00153291000458,
1.7907359329079));
#40659=CARTESIAN_POINT('Ctrl Pts',(-3.52832327752009,-3.22231029225817,
0.361177417303153));
#40660=CARTESIAN_POINT('Ctrl Pts',(-3.50622655072697,-3.2197356494399,0.00248066872637863));
#40661=CARTESIAN_POINT('Origin',(-56.8777734492732,0.,0.));
#40662=CARTESIAN_POINT('',(-6.25277344927318,-3.21789630792886,0.0012091821211443));
#40663=CARTESIAN_POINT('',(-6.00622655072697,-3.22181408586928,-0.00292332824735064));
#40664=CARTESIAN_POINT('',(-56.8777734492732,-3.22275,1.66140794472856E-12));
#40665=CARTESIAN_POINT('Ctrl Pts',(-6.25277344927318,-3.21789630792886,
0.00120918212114421));
#40666=CARTESIAN_POINT('Ctrl Pts',(-6.21503262562757,-3.21582712733459,
-0.612317502979839));
#40667=CARTESIAN_POINT('Ctrl Pts',(-6.11113408473924,-2.75156807830961,
-2.30422559493896));
#40668=CARTESIAN_POINT('Ctrl Pts',(-5.94107782660823,-0.0154015163207855,
-3.80917945408937));
#40669=CARTESIAN_POINT('Ctrl Pts',(-5.74260467488009,3.19208523418617,-2.07862386640746));
#40670=CARTESIAN_POINT('Ctrl Pts',(-5.54413152315197,3.47747956887825,1.55474151163881));
#40671=CARTESIAN_POINT('Ctrl Pts',(-5.34565837142383,0.57952636479995,3.76486845887453));
#40672=CARTESIAN_POINT('Ctrl Pts',(-5.16520568013092,-2.53764694845794,
2.64081745748553));
#40673=CARTESIAN_POINT('Ctrl Pts',(-5.0509107060807,-3.21468852612825,0.777441306115686));
#40674=CARTESIAN_POINT('Ctrl Pts',(-5.00277344927319,-3.2214948345208,-0.00289333062280996));
#40675=CARTESIAN_POINT('Ctrl Pts',(-6.00622655072697,-3.22181408586928,
-0.00292332824735106));
#40676=CARTESIAN_POINT('Ctrl Pts',(-5.98888255109927,-3.22431174733808,
-0.284009412405685));
#40677=CARTESIAN_POINT('Ctrl Pts',(-5.90538083422887,-3.06191100119738,
-1.63444269098198));
#40678=CARTESIAN_POINT('Ctrl Pts',(-5.75572140011576,-1.16790816827868,
-3.62575163696693));
#40679=CARTESIAN_POINT('Ctrl Pts',(-5.55724824838763,2.41297691887338,-2.94747804273184));
#40680=CARTESIAN_POINT('Ctrl Pts',(-5.35877509665951,3.78497939857008,0.428970131116378));
#40681=CARTESIAN_POINT('Ctrl Pts',(-5.16030194493137,1.69214344806,3.41273130701552));
#40682=CARTESIAN_POINT('Ctrl Pts',(-4.96182879320323,-1.94971114633403,
3.27241667179486));
#40683=CARTESIAN_POINT('Ctrl Pts',(-4.8271369951351,-3.20998195595637,1.14424004540375));
#40684=CARTESIAN_POINT('Ctrl Pts',(-4.75860291430968,-3.22796450590223,
0.0390337711987965));
#40685=CARTESIAN_POINT('Ctrl Pts',(-4.75622655072696,-3.22785018800479,
0.000707833695615589));
#40686=CARTESIAN_POINT('Origin',(-56.8777734492732,0.,0.));
#40687=CARTESIAN_POINT('',(-7.50277344927318,-3.22592194266142,0.00226059365463134));
#40688=CARTESIAN_POINT('',(-7.25622655072695,-3.21778123234973,0.00104187359324354));
#40689=CARTESIAN_POINT('',(-56.8777734492732,-3.22275,1.66140794472856E-12));
#40690=CARTESIAN_POINT('Ctrl Pts',(-7.50277344927318,-3.22592194266142,
0.00226059365463134));
#40691=CARTESIAN_POINT('Ctrl Pts',(-7.44531226241716,-3.21851947260152,
-0.925935031015119));
#40692=CARTESIAN_POINT('Ctrl Pts',(-7.32169335831845,-2.31013732855039,
-2.93544523349847));
#40693=CARTESIAN_POINT('Ctrl Pts',(-7.131916736977,1.10141150988432,-3.6465021604372));
#40694=CARTESIAN_POINT('Ctrl Pts',(-6.93344358524887,3.6610429062145,-1.05206946493042));
#40695=CARTESIAN_POINT('Ctrl Pts',(-6.73497043352074,2.86928957276539,2.50544660046798));
#40696=CARTESIAN_POINT('Ctrl Pts',(-6.5364972817926,-0.549063204013273,
3.76943164391853));
#40697=CARTESIAN_POINT('Ctrl Pts',(-6.3757649537101,-2.91035052847904,1.99860958833013));
#40698=CARTESIAN_POINT('Ctrl Pts',(-6.28119034287028,-3.2194542941915,0.463163131330338));
#40699=CARTESIAN_POINT('Ctrl Pts',(-6.25277344927318,-3.21789630792886,
0.00120918212114421));
#40700=CARTESIAN_POINT('Ctrl Pts',(-7.25622655072695,-3.21778123234973,
0.0010418735932435));
#40701=CARTESIAN_POINT('Ctrl Pts',(-7.21916218788886,-3.21603388168955,
-0.601541814863301));
#40702=CARTESIAN_POINT('Ctrl Pts',(-7.11594010780805,-2.76410687756682,
-2.28213517941486));
#40703=CARTESIAN_POINT('Ctrl Pts',(-6.94656031048453,-0.0542566740194617,
-3.80882404895191));
#40704=CARTESIAN_POINT('Ctrl Pts',(-6.74808715875641,3.17071582455421,-2.11107687744781));
#40705=CARTESIAN_POINT('Ctrl Pts',(-6.54961400702828,3.49315785049429,1.51918815623972));
#40706=CARTESIAN_POINT('Ctrl Pts',(-6.35114085530014,0.617900155701453,
3.75876094213507));
#40707=CARTESIAN_POINT('Ctrl Pts',(-6.17001170319971,-2.52230457329154,
2.66247123123546));
#40708=CARTESIAN_POINT('Ctrl Pts',(-6.05504026834198,-3.21478455725691,
0.788177746023009));
#40709=CARTESIAN_POINT('Ctrl Pts',(-6.00622655072697,-3.22181408586928,
-0.00292332824735106));
#40710=CARTESIAN_POINT('Origin',(-56.8777734492732,0.,0.));
#40711=CARTESIAN_POINT('',(-8.75277344927317,-3.22488322984771,-0.00262779420977039));
#40712=CARTESIAN_POINT('',(-8.50622655072697,-3.22563167876346,0.00238074690490087));
#40713=CARTESIAN_POINT('',(-56.8777734492732,-3.22275,1.66140794472856E-12));
#40714=CARTESIAN_POINT('Ctrl Pts',(-8.75277344927317,-3.22488322984771,
-0.0026277942097702));
#40715=CARTESIAN_POINT('Ctrl Pts',(-8.74174961644946,-3.22645652139871,
-0.180849833123689));
#40716=CARTESIAN_POINT('Ctrl Pts',(-8.66456806638304,-3.13193301652771,
-1.42697228178268));
#40717=CARTESIAN_POINT('Ctrl Pts',(-8.52122879907392,-1.50764057830064,
-3.49815740166747));
#40718=CARTESIAN_POINT('Ctrl Pts',(-8.32275564734576,2.12153960142961,-3.1637248678963));
#40719=CARTESIAN_POINT('Ctrl Pts',(-8.12428249561765,3.80862415267616,0.0668384906429997));
#40720=CARTESIAN_POINT('Ctrl Pts',(-7.92580934388952,2.00922543843686,3.23621668893135));
#40721=CARTESIAN_POINT('Ctrl Pts',(-7.72733619216139,-1.62945449308302,
3.44310374156095));
#40722=CARTESIAN_POINT('Ctrl Pts',(-7.58632422728927,-3.15489729953755,
1.35073438181086));
#40723=CARTESIAN_POINT('Ctrl Pts',(-7.51146997965987,-3.22704227813193,
0.142739443751509));
#40724=CARTESIAN_POINT('Ctrl Pts',(-7.50277344927318,-3.22592194266142,
0.00226059365463134));
#40725=CARTESIAN_POINT('Ctrl Pts',(-8.50622655072697,-3.22563167876345,
0.00238074690490067));
#40726=CARTESIAN_POINT('Ctrl Pts',(-8.44944182467846,-3.2180404664003,-0.915102997096774));
#40727=CARTESIAN_POINT('Ctrl Pts',(-8.32649938138723,-2.32782638712261,
-2.91438608798932));
#40728=CARTESIAN_POINT('Ctrl Pts',(-8.13739922085333,1.06415762040292,-3.65754739976015));
#40729=CARTESIAN_POINT('Ctrl Pts',(-7.93892606912516,3.65012056591666,-1.08935957187082));
#40730=CARTESIAN_POINT('Ctrl Pts',(-7.74045291739707,2.89469728902442,2.47604766260028));
#40731=CARTESIAN_POINT('Ctrl Pts',(-7.54197976566891,-0.510584113075111,
3.77483619327098));
#40732=CARTESIAN_POINT('Ctrl Pts',(-7.38057097677889,-2.89982523894728,
2.02084194588588));
#40733=CARTESIAN_POINT('Ctrl Pts',(-7.28531990513157,-3.21915280029623,
0.474034782800556));
#40734=CARTESIAN_POINT('Ctrl Pts',(-7.25622655072695,-3.21778123234973,
0.0010418735932435));
#40735=CARTESIAN_POINT('Origin',(-56.8777734492732,0.,0.));
#40736=CARTESIAN_POINT('',(-10.0027734492732,-3.21757454106912,-0.000618869751645723));
#40737=CARTESIAN_POINT('',(-9.75622655072694,-3.22519593513859,-0.00253467400071289));
#40738=CARTESIAN_POINT('',(-56.8777734492732,-3.22275,1.66140794472856E-12));
#40739=CARTESIAN_POINT('Ctrl Pts',(-10.0027734492732,-3.21757454106912,
-0.000618869751645747));
#40740=CARTESIAN_POINT('Ctrl Pts',(-9.97202925323905,-3.21843235789835,
-0.500530984194887));
#40741=CARTESIAN_POINT('Ctrl Pts',(-9.87512733996222,-2.87350040501786,
-2.07507144870353));
#40742=CARTESIAN_POINT('Ctrl Pts',(-9.71206770944269,-0.416464461400303,
-3.78637592858529));
#40743=CARTESIAN_POINT('Ctrl Pts',(-9.51359455771457,2.95543310591665,-2.40322709635013));
#40744=CARTESIAN_POINT('Ctrl Pts',(-9.31512140598641,3.62187388543242,1.17987917949349));
#40745=CARTESIAN_POINT('Ctrl Pts',(-9.11664825425831,0.972785963491132,
3.6829027667608));
#40746=CARTESIAN_POINT('Ctrl Pts',(-8.92919893535388,-2.37020743770456,
2.86276287115722));
#40747=CARTESIAN_POINT('Ctrl Pts',(-8.80790733369217,-3.21701467125132,
0.888720383101256));
#40748=CARTESIAN_POINT('Ctrl Pts',(-8.75277344927317,-3.22488322984771,
-0.0026277942097702));
#40749=CARTESIAN_POINT('Ctrl Pts',(-9.75622655072694,-3.22519593513859,
-0.0025346740007132));
#40750=CARTESIAN_POINT('Ctrl Pts',(-9.74587917871075,-3.22663930449054,
-0.169778291868378));
#40751=CARTESIAN_POINT('Ctrl Pts',(-9.66937408945183,-3.1387605467685,-1.40480258922794));
#40752=CARTESIAN_POINT('Ctrl Pts',(-9.52671128295022,-1.54324543714212,
-3.48259643704148));
#40753=CARTESIAN_POINT('Ctrl Pts',(-9.3282381312221,2.0891572291558,-3.18520117016493));
#40754=CARTESIAN_POINT('Ctrl Pts',(-9.12976497949396,3.80910767480012,0.0279847160571414));
#40755=CARTESIAN_POINT('Ctrl Pts',(-8.93129182776584,2.0421322300825,3.21555288829343));
#40756=CARTESIAN_POINT('Ctrl Pts',(-8.73281867603769,-1.59424790270054,
3.45954593079627));
#40757=CARTESIAN_POINT('Ctrl Pts',(-8.59113025035809,-3.14837458608671,
1.37288362723526));
#40758=CARTESIAN_POINT('Ctrl Pts',(-8.51559954192117,-3.22688469822105,
0.153822299092808));
#40759=CARTESIAN_POINT('Ctrl Pts',(-8.50622655072697,-3.22563167876345,
0.00238074690490067));
#40760=CARTESIAN_POINT('Origin',(-56.8777734492732,0.,0.));
#40761=CARTESIAN_POINT('',(-11.2527734492732,-3.22261253269744,0.00294729705999707));
#40762=CARTESIAN_POINT('',(-11.0062265507269,-3.2176463632475,-0.000794354628363692));
#40763=CARTESIAN_POINT('',(-56.8777734492732,-3.22275,1.66140794472856E-12));
#40764=CARTESIAN_POINT('Ctrl Pts',(-11.2527734492732,-3.22261253269744,
0.00294729705999697));
#40765=CARTESIAN_POINT('Ctrl Pts',(-11.2023088900286,-3.21512743946722,
-0.814391719427845));
#40766=CARTESIAN_POINT('Ctrl Pts',(-11.0856866135414,-2.48411033802337,
-2.71515413077375));
#40767=CARTESIAN_POINT('Ctrl Pts',(-10.9029066198115,0.711270052496804,
-3.74221595216));
#40768=CARTESIAN_POINT('Ctrl Pts',(-10.7044334680833,3.52989055571641,-1.43176743392344));
#40769=CARTESIAN_POINT('Ctrl Pts',(-10.5059603163552,3.11718555708669,2.18934682562397));
#40770=CARTESIAN_POINT('Ctrl Pts',(-10.3074871646271,-0.14904734152245,
3.80629350026567));
#40771=CARTESIAN_POINT('Ctrl Pts',(-10.1397582089331,-2.79402367672853,
2.22815779781535));
#40772=CARTESIAN_POINT('Ctrl Pts',(-10.0381869704818,-3.21658644190266,
0.57521821662457));
#40773=CARTESIAN_POINT('Ctrl Pts',(-10.0027734492732,-3.21757454106912,
-0.000618869751645747));
#40774=CARTESIAN_POINT('Ctrl Pts',(-11.0062265507269,-3.2176463632475,-0.000794354628363692));
#40775=CARTESIAN_POINT('Ctrl Pts',(-10.9761588155003,-3.21872454724075,
-0.489679676012747));
#40776=CARTESIAN_POINT('Ctrl Pts',(-10.879933363031,-2.88439762842973,-2.05285499893439));
#40777=CARTESIAN_POINT('Ctrl Pts',(-10.717550193319,-0.45506613045934,-3.78193062330111));
#40778=CARTESIAN_POINT('Ctrl Pts',(-10.5190770415909,2.93076486464135,-2.43324921262453));
#40779=CARTESIAN_POINT('Ctrl Pts',(-10.3206038898627,3.63372082507465,1.1428724285645));
#40780=CARTESIAN_POINT('Ctrl Pts',(-10.1221307381346,1.01030318175698,3.67278802866238));
#40781=CARTESIAN_POINT('Ctrl Pts',(-9.93400495842269,-2.35297576150677,
2.88395492681478));
#40782=CARTESIAN_POINT('Ctrl Pts',(-9.81203689595346,-3.21741087225541,
0.899522779380902));
#40783=CARTESIAN_POINT('Ctrl Pts',(-9.75622655072694,-3.22519593513859,
-0.0025346740007132));
#40784=CARTESIAN_POINT('Origin',(-56.8777734492732,0.,0.));
#40785=CARTESIAN_POINT('',(-12.5027734492732,-3.22751844495433,-0.00117408986154981));
#40786=CARTESIAN_POINT('',(-12.2562265507269,-3.22228269638671,0.00294601968564429));
#40787=CARTESIAN_POINT('',(-56.8777734492732,-3.22275,1.66140794472856E-12));
#40788=CARTESIAN_POINT('Ctrl Pts',(-12.5027734492732,-3.22751844495433,
-0.00117408986154978));
#40789=CARTESIAN_POINT('Ctrl Pts',(-12.4987462440609,-3.22782301707217,
-0.0661425850922179));
#40790=CARTESIAN_POINT('Ctrl Pts',(-12.428561321606,-3.19659648953803,-1.19809562747136));
#40791=CARTESIAN_POINT('Ctrl Pts',(-12.2922186819084,-1.86765162909789,
-3.31993414279675));
#40792=CARTESIAN_POINT('Ctrl Pts',(-12.0937455301802,1.77656732297672,-3.36955395669975));
#40793=CARTESIAN_POINT('Ctrl Pts',(-11.8952723784521,3.7944844943374,-0.334623284325299));
#40794=CARTESIAN_POINT('Ctrl Pts',(-11.696799226724,2.33886209856671,3.00662757987545));
#40795=CARTESIAN_POINT('Ctrl Pts',(-11.4983260749959,-1.2577968605525,3.59555731114996));
#40796=CARTESIAN_POINT('Ctrl Pts',(-11.3503174825123,-3.08130730766144,
1.58019933119097));
#40797=CARTESIAN_POINT('Ctrl Pts',(-11.2684666072713,-3.22494020091553,
0.2571183532596));
#40798=CARTESIAN_POINT('Ctrl Pts',(-11.2527734492732,-3.22261253269744,
0.00294729705999697));
#40799=CARTESIAN_POINT('Ctrl Pts',(-12.2562265507269,-3.22228269638671,
0.00294601968564401));
#40800=CARTESIAN_POINT('Ctrl Pts',(-12.2064384522899,-3.21496785738077,
-0.803647489328101));
#40801=CARTESIAN_POINT('Ctrl Pts',(-12.0904926366102,-2.49989067661973,
-2.69359488486215));
#40802=CARTESIAN_POINT('Ctrl Pts',(-11.9083891036878,0.673060134005079,
-3.74927652735391));
#40803=CARTESIAN_POINT('Ctrl Pts',(-11.7099159519597,3.51510189157322,-1.46769994018271));
#40804=CARTESIAN_POINT('Ctrl Pts',(-11.5114428002315,3.1393559572694,2.15743565283212));
#40805=CARTESIAN_POINT('Ctrl Pts',(-11.3129696485034,-0.110213061344868,
3.80761572426406));
#40806=CARTESIAN_POINT('Ctrl Pts',(-11.1445642320019,-2.78188136687003,
2.25028698315051));
#40807=CARTESIAN_POINT('Ctrl Pts',(-11.0423165327431,-3.2163522304958,0.58600948422847));
#40808=CARTESIAN_POINT('Ctrl Pts',(-11.0062265507269,-3.2176463632475,-0.000794354628363692));
#40809=CARTESIAN_POINT('Origin',(-56.8777734492732,0.,0.));
#40810=CARTESIAN_POINT('',(-13.7527734492732,-3.21913376994867,-0.00221167296974806));
#40811=CARTESIAN_POINT('',(-13.5062265507269,-3.22767212133845,-0.000986736498302387));
#40812=CARTESIAN_POINT('',(-56.8777734492732,-3.22275,1.66140794472856E-12));
#40813=CARTESIAN_POINT('Ctrl Pts',(-13.7527734492732,-3.21913376994867,
-0.00221167296974831));
#40814=CARTESIAN_POINT('Ctrl Pts',(-13.7290258808505,-3.22157097183896,
-0.387887941665459));
#40815=CARTESIAN_POINT('Ctrl Pts',(-13.6391205951852,-2.97894141443826,
-1.84504509362306));
#40816=CARTESIAN_POINT('Ctrl Pts',(-13.4830575922771,-0.812895766645905,
-3.72146285655909));
#40817=CARTESIAN_POINT('Ctrl Pts',(-13.284584440549,2.68591262275001,-2.70110323814768));
#40818=CARTESIAN_POINT('Ctrl Pts',(-13.0861112888209,3.72598813738973,0.791895018427709));
#40819=CARTESIAN_POINT('Ctrl Pts',(-12.8876381370928,1.35522688587594,3.55997828757123));
#40820=CARTESIAN_POINT('Ctrl Pts',(-12.6931921905769,-2.18285564035938,
3.07915168903474));
#40821=CARTESIAN_POINT('Ctrl Pts',(-12.5649039613036,-3.22281959782984,
1.00114033461412));
#40822=CARTESIAN_POINT('Ctrl Pts',(-12.5027734492732,-3.22751844495433,
-0.00117408986154978));
#40823=CARTESIAN_POINT('Ctrl Pts',(-13.5062265507269,-3.22767212133845,
-0.0009867364983027));
#40824=CARTESIAN_POINT('Ctrl Pts',(-13.5028758063222,-3.22788966329458,
-0.0550354332043843));
#40825=CARTESIAN_POINT('Ctrl Pts',(-13.4333673446748,-3.20216558835672,
-1.1760201796722));
#40826=CARTESIAN_POINT('Ctrl Pts',(-13.2977011657847,-1.9014197600839,-3.30071012336989));
#40827=CARTESIAN_POINT('Ctrl Pts',(-13.0992280140566,1.74210332689385,-3.38750061564265));
#40828=CARTESIAN_POINT('Ctrl Pts',(-12.9007548623284,3.79087359697976,-0.373311926243645));
#40829=CARTESIAN_POINT('Ctrl Pts',(-12.7022817106003,2.36940978052417,2.98261323582365));
#40830=CARTESIAN_POINT('Ctrl Pts',(-12.5038085588722,-1.22105449849256,
3.60820042878236));
#40831=CARTESIAN_POINT('Ctrl Pts',(-12.3551235055811,-3.07345562513412,
1.60242275642856));
#40832=CARTESIAN_POINT('Ctrl Pts',(-12.2725961695326,-3.22468771143873,
0.268142496116896));
#40833=CARTESIAN_POINT('Ctrl Pts',(-12.2562265507269,-3.22228269638671,
0.00294601968564401));
#40834=CARTESIAN_POINT('Origin',(-56.8777734492732,0.,0.));
#40835=CARTESIAN_POINT('',(-15.0027734492732,-3.21951085124981,0.00239014585722026));
#40836=CARTESIAN_POINT('',(-14.7562265507269,-3.21937116695345,-0.0023282602058064));
#40837=CARTESIAN_POINT('',(-56.8777734492732,-3.22275,1.66140794472856E-12));
#40838=CARTESIAN_POINT('Ctrl Pts',(-15.0027734492732,-3.21951085124981,
0.00239014585722008));
#40839=CARTESIAN_POINT('Ctrl Pts',(-14.9593055176401,-3.21465332639279,
-0.703350054867812));
#40840=CARTESIAN_POINT('Ctrl Pts',(-14.8496798687644,-2.63873730532825,
-2.49042930614228));
#40841=CARTESIAN_POINT('Ctrl Pts',(-14.6738965026459,0.313218324198597,
-3.79631131515394));
#40842=CARTESIAN_POINT('Ctrl Pts',(-14.4754233509178,3.35948111786941,-1.79554224090064));
#40843=CARTESIAN_POINT('Ctrl Pts',(-14.2769501991897,3.33041428366469,1.84889859628423));
#40844=CARTESIAN_POINT('Ctrl Pts',(-14.0784770474615,0.252626126046346,
3.80082430015101));
#40845=CARTESIAN_POINT('Ctrl Pts',(-13.903751464156,-2.66048884593533,2.45616432920152));
#40846=CARTESIAN_POINT('Ctrl Pts',(-13.7951835980932,-3.21478123612154,
0.686557284789165));
#40847=CARTESIAN_POINT('Ctrl Pts',(-13.7527734492732,-3.21913376994867,
-0.00221167296974831));
#40848=CARTESIAN_POINT('Ctrl Pts',(-14.7562265507269,-3.21937116695345,
-0.00232826020580643));
#40849=CARTESIAN_POINT('Ctrl Pts',(-14.7331554431118,-3.22187553896581,
-0.376948878832709));
#40850=CARTESIAN_POINT('Ctrl Pts',(-14.643926618254,-2.98830157339018,-1.82279076916866));
#40851=CARTESIAN_POINT('Ctrl Pts',(-14.4885400761535,-0.850814645052164,
-3.71297708884916));
#40852=CARTESIAN_POINT('Ctrl Pts',(-14.2900669244253,2.6582198935355,-2.72836057370837));
#40853=CARTESIAN_POINT('Ctrl Pts',(-14.0915937726972,3.73387198132893,0.753846436352181));
#40854=CARTESIAN_POINT('Ctrl Pts',(-13.8931206209691,1.39147028998462,3.54596881749461));
#40855=CARTESIAN_POINT('Ctrl Pts',(-13.6979982136457,-2.1636578828704,3.09971074376555));
#40856=CARTESIAN_POINT('Ctrl Pts',(-13.5690335235649,-3.22359447467857,
1.01211203080251));
#40857=CARTESIAN_POINT('Ctrl Pts',(-13.5062265507269,-3.22767212133845,
-0.0009867364983027));
#40858=CARTESIAN_POINT('Origin',(-56.8777734492732,0.,0.));
#40859=CARTESIAN_POINT('',(-16.2527734492731,-3.22774822845993,0.000878740854861755));
#40860=CARTESIAN_POINT('',(-16.0062265507269,-3.21926592552825,0.00227844397724913));
#40861=CARTESIAN_POINT('',(-56.8777734492732,-3.22275,1.66140794472856E-12));
#40862=CARTESIAN_POINT('Ctrl Pts',(-16.2527734492731,-3.22774822845993,
0.000878740854861754));
#40863=CARTESIAN_POINT('Ctrl Pts',(-16.1895851544297,-3.22404919134472,
-1.01830685280946));
#40864=CARTESIAN_POINT('Ctrl Pts',(-16.0602391423435,-2.15275090221681,
-3.11126884796112));
#40865=CARTESIAN_POINT('Ctrl Pts',(-15.8647354130147,1.41183724821851,-3.53790911481943));
#40866=CARTESIAN_POINT('Ctrl Pts',(-15.6662622612865,3.73814511142124,-0.732363602411441));
#40867=CARTESIAN_POINT('Ctrl Pts',(-15.4677891095585,2.64248749510294,2.7436007651268));
#40868=CARTESIAN_POINT('Ctrl Pts',(-15.2693159578303,-0.872150850636688,
3.70802349155361));
#40869=CARTESIAN_POINT('Ctrl Pts',(-15.1143107377352,-2.99351493580881,
1.81024609645543));
#40870=CARTESIAN_POINT('Ctrl Pts',(-15.0254632348828,-3.22204642617731,
0.370778823417696));
#40871=CARTESIAN_POINT('Ctrl Pts',(-15.0027734492732,-3.21951085124981,
0.00239014585722008));
#40872=CARTESIAN_POINT('Ctrl Pts',(-16.0062265507269,-3.21926592552825,
0.00227844397724927));
#40873=CARTESIAN_POINT('Ctrl Pts',(-15.9634350799014,-3.21472983079245,
-0.692611678211759));
#40874=CARTESIAN_POINT('Ctrl Pts',(-15.8544858918332,-2.65269578681809,
-2.46852391928997));
#40875=CARTESIAN_POINT('Ctrl Pts',(-15.6793789865222,0.274477321913715,
-3.79930870321287));
#40876=CARTESIAN_POINT('Ctrl Pts',(-15.4809058347941,3.34099059953505,-1.82971752912093));
#40877=CARTESIAN_POINT('Ctrl Pts',(-15.282432683066,3.34910080337457,1.81483008333833));
#40878=CARTESIAN_POINT('Ctrl Pts',(-15.0839595313379,0.291383706511294,
3.79804949390259));
#40879=CARTESIAN_POINT('Ctrl Pts',(-14.9085574872248,-2.64662678665883,
2.47808446093996));
#40880=CARTESIAN_POINT('Ctrl Pts',(-14.7993131603545,-3.2146941093514,0.697297116369363));
#40881=CARTESIAN_POINT('Ctrl Pts',(-14.7562265507269,-3.21937116695345,
-0.00232826020580643));
#40882=CARTESIAN_POINT('Origin',(-56.8777734492732,0.,0.));
#40883=CARTESIAN_POINT('',(-17.5027734492731,-3.22209836681519,-0.00294005213236294));
#40884=CARTESIAN_POINT('',(-17.2562265507269,-3.22760793986041,0.00106918008988845));
#40885=CARTESIAN_POINT('',(-56.8777734492732,-3.22275,1.66140794472856E-12));
#40886=CARTESIAN_POINT('Ctrl Pts',(-17.5027734492732,-3.22209836681519,
-0.00294005213236352));
#40887=CARTESIAN_POINT('Ctrl Pts',(-17.486022508462,-3.22454236991077,-0.274353756782468));
#40888=CARTESIAN_POINT('Ctrl Pts',(-17.4031138504082,-3.06897092992912,
-1.61495252967173));
#40889=CARTESIAN_POINT('Ctrl Pts',(-17.2540474751116,-1.2002865876007,-3.61516215788525));
#40890=CARTESIAN_POINT('Ctrl Pts',(-17.0555743233835,2.38652121163826,-2.96893951211207));
#40891=CARTESIAN_POINT('Ctrl Pts',(-16.8571011716553,3.78866443554566,0.395103929379446));
#40892=CARTESIAN_POINT('Ctrl Pts',(-16.6586280199273,1.72259587914657,3.39746210535554));
#40893=CARTESIAN_POINT('Ctrl Pts',(-16.4601548681991,-1.92036802451838,
3.28972217224905));
#40894=CARTESIAN_POINT('Ctrl Pts',(-16.3248700113144,-3.20525340772958,
1.1635806507222));
#40895=CARTESIAN_POINT('Ctrl Pts',(-16.2557428716724,-3.22792205818097,
0.04877356913509));
#40896=CARTESIAN_POINT('Ctrl Pts',(-16.2527734492731,-3.22774822845993,
0.000878740854861754));
#40897=CARTESIAN_POINT('Ctrl Pts',(-17.2562265507269,-3.22760793986041,
0.00106918008988849));
#40898=CARTESIAN_POINT('Ctrl Pts',(-17.193714716691,-3.22325142349043,-1.00732234075576));
#40899=CARTESIAN_POINT('Ctrl Pts',(-17.0650451654124,-2.17205757669084,
-3.09074945429766));
#40900=CARTESIAN_POINT('Ctrl Pts',(-16.870217896891,1.37567491389401,-3.55212653967123));
#40901=CARTESIAN_POINT('Ctrl Pts',(-16.6717447451629,3.73047995257294,-0.770456842402849));
#40902=CARTESIAN_POINT('Ctrl Pts',(-16.4732715934348,2.67033633643725,2.7165029491714));
#40903=CARTESIAN_POINT('Ctrl Pts',(-16.2747984417066,-0.834281340932724,
3.71672692926525));
#40904=CARTESIAN_POINT('Ctrl Pts',(-16.119116760804,-2.98423536114668,1.83250028631888));
#40905=CARTESIAN_POINT('Ctrl Pts',(-16.0295927971441,-3.22174285621849,
0.381722606907516));
#40906=CARTESIAN_POINT('Ctrl Pts',(-16.0062265507269,-3.21926592552825,
0.00227844397724927));
#40907=CARTESIAN_POINT('Origin',(-56.8777734492732,0.,0.));
#40908=CARTESIAN_POINT('',(-18.7527734492731,-3.21769487768588,0.000892040993440023));
#40909=CARTESIAN_POINT('',(-18.5062265507269,-3.22242620475109,-0.00294804637601787));
#40910=CARTESIAN_POINT('',(-56.8777734492732,-3.22275,1.66140794472856E-12));
#40911=CARTESIAN_POINT('Ctrl Pts',(-18.7527734492731,-3.21769487768588,
0.000892040993440008));
#40912=CARTESIAN_POINT('Ctrl Pts',(-18.7163021452516,-3.21622499493547,
-0.592089635668959));
#40913=CARTESIAN_POINT('Ctrl Pts',(-18.6136731239874,-2.77496559282729,
-2.26275470710555));
#40914=CARTESIAN_POINT('Ctrl Pts',(-18.4448863854804,-0.088316809298266,
-3.80818663688835));
#40915=CARTESIAN_POINT('Ctrl Pts',(-18.2464132337523,3.15170977273075,-2.13934822519688));
#40916=CARTESIAN_POINT('Ctrl Pts',(-18.0479400820241,3.50660436488545,1.48788815048238));
#40917=CARTESIAN_POINT('Ctrl Pts',(-17.849466930296,0.651490054412623,3.7530848683691));
#40918=CARTESIAN_POINT('Ctrl Pts',(-17.667744719379,-2.50870676080208,2.68142439262922));
#40919=CARTESIAN_POINT('Ctrl Pts',(-17.5521802257047,-3.2148897977024,0.797592668823855));
#40920=CARTESIAN_POINT('Ctrl Pts',(-17.5027734492732,-3.22209836681519,
-0.00294005213236352));
#40921=CARTESIAN_POINT('Ctrl Pts',(-18.5062265507269,-3.22242620475109,
-0.00294804637601842));
#40922=CARTESIAN_POINT('Ctrl Pts',(-18.4901520707233,-3.22479872987954,
-0.263333526885802));
#40923=CARTESIAN_POINT('Ctrl Pts',(-18.407919873477,-3.07689763924138,-1.59272602597641));
#40924=CARTESIAN_POINT('Ctrl Pts',(-18.2595299589879,-1.23710096689095,
-3.6027303007957));
#40925=CARTESIAN_POINT('Ctrl Pts',(-18.0610568072598,2.35611197454017,-2.99312892906109));
#40926=CARTESIAN_POINT('Ctrl Pts',(-17.8625836555317,3.79249750493022,0.356436667098387));
#40927=CARTESIAN_POINT('Ctrl Pts',(-17.6641105038036,1.75716239414189,3.37971370727872));
#40928=CARTESIAN_POINT('Ctrl Pts',(-17.4656373520754,-1.88671087539651,
3.30913984219684));
#40929=CARTESIAN_POINT('Ctrl Pts',(-17.3296760343832,-3.19975019779073,
1.18565042945036));
#40930=CARTESIAN_POINT('Ctrl Pts',(-17.2598724339337,-3.22786202534867,
0.0598816876481213));
#40931=CARTESIAN_POINT('Ctrl Pts',(-17.2562265507269,-3.22760793986041,
0.00106918008988849));
#40932=CARTESIAN_POINT('Origin',(-56.8777734492732,0.,0.));
#40933=CARTESIAN_POINT('',(-20.0027734492731,-3.22536883419238,0.00247717968785189));
#40934=CARTESIAN_POINT('',(-19.7562265507269,-3.21761277853822,0.000718109111264298));
#40935=CARTESIAN_POINT('',(-56.8777734492732,-3.22275,1.66140794472856E-12));
#40936=CARTESIAN_POINT('Ctrl Pts',(-20.0027734492731,-3.22536883419238,
0.00247717968785173));
#40937=CARTESIAN_POINT('Ctrl Pts',(-19.9465817820412,-3.2176490068956,-0.905617113904481));
#40938=CARTESIAN_POINT('Ctrl Pts',(-19.8242323975665,-2.34317999425177,
-2.89587764470511));
#40939=CARTESIAN_POINT('Ctrl Pts',(-19.6357252958492,1.03140566167082,-3.66691800852612));
#40940=CARTESIAN_POINT('Ctrl Pts',(-19.437252144121,3.64023257295061,-1.12195906120018));
#40941=CARTESIAN_POINT('Ctrl Pts',(-19.2387789923929,2.9167249089872,2.45006145340748));
#40942=CARTESIAN_POINT('Ctrl Pts',(-19.0403058406648,-0.476805360925414,
3.77925150895946));
#40943=CARTESIAN_POINT('Ctrl Pts',(-18.8783039929582,-2.89047297318496,
2.04032844964183));
#40944=CARTESIAN_POINT('Ctrl Pts',(-18.7824598624943,-3.21889131274313,
0.483559155818458));
#40945=CARTESIAN_POINT('Ctrl Pts',(-18.7527734492731,-3.21769487768588,
0.000892040993440008));
#40946=CARTESIAN_POINT('Ctrl Pts',(-19.7562265507269,-3.21761277853822,
0.000718109111264124));
#40947=CARTESIAN_POINT('Ctrl Pts',(-19.7204317075129,-3.21645311094604,
-0.581302092212425));
#40948=CARTESIAN_POINT('Ctrl Pts',(-19.6184791470562,-2.78719884611832,
-2.24063383593941));
#40949=CARTESIAN_POINT('Ctrl Pts',(-19.4503688693567,-0.12715804379987,
-3.80708750286241));
#40950=CARTESIAN_POINT('Ctrl Pts',(-19.2518957176286,3.12972303941186,-2.17138622062695));
#40951=CARTESIAN_POINT('Ctrl Pts',(-19.0534225659005,3.52159918511936,1.4520411846503));
#40952=CARTESIAN_POINT('Ctrl Pts',(-18.8549494141723,0.689739899217004,
3.74624389141739));
#40953=CARTESIAN_POINT('Ctrl Pts',(-18.6725507424478,-2.49302790386833,
2.70300609504122));
#40954=CARTESIAN_POINT('Ctrl Pts',(-18.556309787966,-3.21503413117626,0.808334669522118));
#40955=CARTESIAN_POINT('Ctrl Pts',(-18.5062265507269,-3.22242620475109,
-0.00294804637601842));
#40956=CARTESIAN_POINT('Origin',(-56.8777734492732,0.,0.));
#40957=CARTESIAN_POINT('',(-21.2527734492731,-3.22546356093439,-0.00244372236887117));
#40958=CARTESIAN_POINT('',(-21.0062265507269,-3.22506038431272,0.00257670913582225));
#40959=CARTESIAN_POINT('',(-56.8777734492732,-3.22275,1.66140794472856E-12));
#40960=CARTESIAN_POINT('Ctrl Pts',(-21.2527734492731,-3.22546356093439,
-0.00244372236887114));
#40961=CARTESIAN_POINT('Ctrl Pts',(-21.2430191360735,-3.22679134021169,
-0.160067793553129));
#40962=CARTESIAN_POINT('Ctrl Pts',(-21.1671071056311,-3.1446431200358,-1.38537302685204));
#40963=CARTESIAN_POINT('Ctrl Pts',(-21.0250373579461,-1.57432862205077,
-3.46865603800252));
#40964=CARTESIAN_POINT('Ctrl Pts',(-20.8265642062179,2.06058850407911,-3.20375722192501));
#40965=CARTESIAN_POINT('Ctrl Pts',(-20.6280910544898,3.80920573593449,-0.00608124192798155));
#40966=CARTESIAN_POINT('Ctrl Pts',(-20.4296179027617,2.07080731049629,3.19716161664916));
#40967=CARTESIAN_POINT('Ctrl Pts',(-20.2311447510336,-1.56324548898088,
3.47366504737583));
#40968=CARTESIAN_POINT('Ctrl Pts',(-20.0888632665374,-3.14255397345149,
1.39230915019779));
#40969=CARTESIAN_POINT('Ctrl Pts',(-20.0127394992839,-3.22673800846152,
0.163535101444709));
#40970=CARTESIAN_POINT('Ctrl Pts',(-20.0027734492731,-3.22536883419238,
0.00247717968785173));
#40971=CARTESIAN_POINT('Ctrl Pts',(-21.0062265507269,-3.22506038431272,
0.00257670913582222));
#40972=CARTESIAN_POINT('Ctrl Pts',(-20.9507113443025,-3.21723391237169,
-0.894808353614492));
#40973=CARTESIAN_POINT('Ctrl Pts',(-20.8290384206354,-2.36051683312814,
-2.87471529474172));
#40974=CARTESIAN_POINT('Ctrl Pts',(-20.6412077797255,0.993947162456761,
-3.67724808257454));
#40975=CARTESIAN_POINT('Ctrl Pts',(-20.4427346279974,3.62859839939353,-1.15903325166825));
#40976=CARTESIAN_POINT('Ctrl Pts',(-20.2442614762692,2.94156519346794,2.42018152937583));
#40977=CARTESIAN_POINT('Ctrl Pts',(-20.0457883245411,-0.438229862995021,
3.78391847292371));
#40978=CARTESIAN_POINT('Ctrl Pts',(-19.883110016027,-2.87966204308117,2.06254890030518));
#40979=CARTESIAN_POINT('Ctrl Pts',(-19.7865894247556,-3.21859646327756,
0.494415090804314));
#40980=CARTESIAN_POINT('Ctrl Pts',(-19.7562265507269,-3.21761277853822,
0.000718109111264124));
#40981=CARTESIAN_POINT('Origin',(-56.8777734492732,0.,0.));
#40982=CARTESIAN_POINT('',(-22.5027734492731,-3.21772419204198,-0.000945844158032132));
#40983=CARTESIAN_POINT('',(-22.2562265507269,-3.22575963611168,-0.00232963559445576));
#40984=CARTESIAN_POINT('',(-56.8777734492732,-3.22275,1.66140794472856E-12));
#40985=CARTESIAN_POINT('Ctrl Pts',(-22.5027734492731,-3.21772419204198,
-0.000945844158032338));
#40986=CARTESIAN_POINT('Ctrl Pts',(-22.4732987728631,-3.21898439121486,
-0.480159460729692));
#40987=CARTESIAN_POINT('Ctrl Pts',(-22.3776663792103,-2.89382542886802,
-2.03337186564838));
#40988=CARTESIAN_POINT('Ctrl Pts',(-22.2158762683149,-0.488869742173803,
-3.77770984795902));
#40989=CARTESIAN_POINT('Ctrl Pts',(-22.0174031165867,2.90888721456023,-2.45936180606832));
#40990=CARTESIAN_POINT('Ctrl Pts',(-21.8189299648586,3.64379633223308,1.11033040550302));
#40991=CARTESIAN_POINT('Ctrl Pts',(-21.6204568131305,1.04310854511736,3.66360613102486));
#40992=CARTESIAN_POINT('Ctrl Pts',(-21.431737974602,-2.33771495359402,2.9024904986763));
#40993=CARTESIAN_POINT('Ctrl Pts',(-21.3091768533162,-3.21778580141147,
0.909002731313567));
#40994=CARTESIAN_POINT('Ctrl Pts',(-21.2527734492731,-3.22546356093439,
-0.00244372236887114));
#40995=CARTESIAN_POINT('Ctrl Pts',(-22.2562265507269,-3.22575963611168,
-0.00232963559445581));
#40996=CARTESIAN_POINT('Ctrl Pts',(-22.2471486983348,-3.22695472404273,
-0.148987392685038));
#40997=CARTESIAN_POINT('Ctrl Pts',(-22.1719131286999,-3.15123563559383,
-1.36321886650731));
#40998=CARTESIAN_POINT('Ctrl Pts',(-22.0305198418224,-1.60962907726382,
-3.45241635035243));
#40999=CARTESIAN_POINT('Ctrl Pts',(-21.8320466900942,2.02780095034114,-3.22460970170803));
#41000=CARTESIAN_POINT('Ctrl Pts',(-21.6335735383662,3.80894540192439,-0.0449371529252134));
#41001=CARTESIAN_POINT('Ctrl Pts',(-21.435100386638,2.1033125106639,3.17587167641245));
#41002=CARTESIAN_POINT('Ctrl Pts',(-21.2366272349099,-1.52773060133581,
3.48943027331057));
#41003=CARTESIAN_POINT('Ctrl Pts',(-21.0936692896062,-3.13579716094896,
1.41447418339441));
#41004=CARTESIAN_POINT('Ctrl Pts',(-21.0168690615452,-3.22656075362891,
0.174609398079968));
#41005=CARTESIAN_POINT('Ctrl Pts',(-21.0062265507269,-3.22506038431272,
0.00257670913582222));
#41006=CARTESIAN_POINT('Origin',(-56.8777734492732,0.,0.));
#41007=CARTESIAN_POINT('',(-23.7527734492731,-3.22199650686841,0.00293511691597435));
#41008=CARTESIAN_POINT('',(-23.5062265507269,-3.21782926820092,-0.00111537477188062));
#41009=CARTESIAN_POINT('',(-56.8777734492732,-3.22275,1.66140794472856E-12));
#41010=CARTESIAN_POINT('Ctrl Pts',(-23.7527734492731,-3.22199650686841,
0.00293511691597463));
#41011=CARTESIAN_POINT('Ctrl Pts',(-23.7035784096527,-3.21484998616783,
-0.794231051178209));
#41012=CARTESIAN_POINT('Ctrl Pts',(-23.5882256527895,-2.51357736811805,
-2.67466106277306));
#41013=CARTESIAN_POINT('Ctrl Pts',(-23.4067151786836,0.639503469586358,
-3.7551458869885));
#41014=CARTESIAN_POINT('Ctrl Pts',(-23.2082420269555,3.50183579684358,-1.4990768399667));
#41015=CARTESIAN_POINT('Ctrl Pts',(-23.0097688752274,3.15852445469445,2.12927419307066));
#41016=CARTESIAN_POINT('Ctrl Pts',(-22.8112957234992,-0.0761571601507046,
3.80844921288671));
#41017=CARTESIAN_POINT('Ctrl Pts',(-22.6422972481812,-2.77110315051519,
2.26967547266405));
#41018=CARTESIAN_POINT('Ctrl Pts',(-22.5394564901058,-3.21615579695349,
0.595464865147483));
#41019=CARTESIAN_POINT('Ctrl Pts',(-22.5027734492731,-3.21772419204198,
-0.000945844158032338));
#41020=CARTESIAN_POINT('Ctrl Pts',(-23.5062265507269,-3.21782926820092,
-0.00111537477188048));
#41021=CARTESIAN_POINT('Ctrl Pts',(-23.4774283351244,-3.21928393819887,
-0.469292530410071));
#41022=CARTESIAN_POINT('Ctrl Pts',(-23.3824724022791,-2.90443597318009,
-2.01114266715587));
#41023=CARTESIAN_POINT('Ctrl Pts',(-23.2213587521912,-0.527379242599795,
-3.77252641568339));
#41024=CARTESIAN_POINT('Ctrl Pts',(-23.022885600463,2.88364878803355,-2.48890620350118));
#41025=CARTESIAN_POINT('Ctrl Pts',(-22.8244124487349,3.65493269060604,1.0731036528189));
#41026=CARTESIAN_POINT('Ctrl Pts',(-22.6259392970067,1.08042526501054,3.65277506415067));
#41027=CARTESIAN_POINT('Ctrl Pts',(-22.4365439976708,-2.32013180474122,
2.9235810681689));
#41028=CARTESIAN_POINT('Ctrl Pts',(-22.3133064155775,-3.21824514318517,
0.91982734519994));
#41029=CARTESIAN_POINT('Ctrl Pts',(-22.2562265507269,-3.22575963611168,
-0.00232963559445581));
#41030=CARTESIAN_POINT('Origin',(-56.8777734492732,0.,0.));
#41031=CARTESIAN_POINT('',(-25.0027734492731,-3.22778696626011,-0.000818109748633706));
#41032=CARTESIAN_POINT('',(-24.7562265507269,-3.22167406644033,0.00291166086733255));
#41033=CARTESIAN_POINT('',(-56.8777734492732,-3.22275,1.66140794472856E-12));
#41034=CARTESIAN_POINT('Ctrl Pts',(-25.0027734492731,-3.22778696626011,
-0.000818109748633739));
#41035=CARTESIAN_POINT('Ctrl Pts',(-25.000015763685,-3.22793832383972,-0.0452963360147774));
#41036=CARTESIAN_POINT('Ctrl Pts',(-24.9311003608541,-3.2069519157609,-1.15667469946367));
#41037=CARTESIAN_POINT('Ctrl Pts',(-24.7960272407805,-1.93086202407817,
-3.28357384021623));
#41038=CARTESIAN_POINT('Ctrl Pts',(-24.5975540890524,1.71173930615894,-3.40294488170616));
#41039=CARTESIAN_POINT('Ctrl Pts',(-24.3990809373243,3.78738359192001,-0.407198781720557));
#41040=CARTESIAN_POINT('Ctrl Pts',(-24.2006077855962,2.3959886047388,2.9613044298318));
#41041=CARTESIAN_POINT('Ctrl Pts',(-24.002134633868,-1.18873758023125,3.6189761377392));
#41042=CARTESIAN_POINT('Ctrl Pts',(-23.8528565217603,-3.06646226142991,
1.62191059947188));
#41043=CARTESIAN_POINT('Ctrl Pts',(-23.7697361268954,-3.22446066032168,
0.277801705602104));
#41044=CARTESIAN_POINT('Ctrl Pts',(-23.7527734492731,-3.22199650686841,
0.00293511691597463));
#41045=CARTESIAN_POINT('Ctrl Pts',(-24.7562265507269,-3.22167406644033,
0.00291166086733272));
#41046=CARTESIAN_POINT('Ctrl Pts',(-24.7077079719139,-3.21473953966774,
-0.783493160315694));
#41047=CARTESIAN_POINT('Ctrl Pts',(-24.5930316758583,-2.52902034751673,
-2.65302825184713));
#41048=CARTESIAN_POINT('Ctrl Pts',(-24.41219766256,0.601165393915808,-3.76147372604303));
#41049=CARTESIAN_POINT('Ctrl Pts',(-24.2137245108318,3.48636199609287,-1.53471966650373));
#41050=CARTESIAN_POINT('Ctrl Pts',(-24.0152513591037,3.18007992525289,2.09694446553971));
#41051=CARTESIAN_POINT('Ctrl Pts',(-23.8167782073755,-0.0373046849413855,
3.80902780024449));
#41052=CARTESIAN_POINT('Ctrl Pts',(-23.64710327125,-2.7586563104495,2.29177527391161));
#41053=CARTESIAN_POINT('Ctrl Pts',(-23.5435860523671,-3.21594214620264,
0.606243964965262));
#41054=CARTESIAN_POINT('Ctrl Pts',(-23.5062265507269,-3.21782926820092,
-0.00111537477188048));
#41055=CARTESIAN_POINT('Origin',(-56.8777734492732,0.,0.));
#41056=CARTESIAN_POINT('',(-26.2527734492731,-3.21959007219934,-0.00242327538640936));
#41057=CARTESIAN_POINT('',(-26.0062265507269,-3.22789335144083,-0.000621618279896263));
#41058=CARTESIAN_POINT('',(-56.8777734492732,-3.22275,1.66140794472856E-12));
#41059=CARTESIAN_POINT('Ctrl Pts',(-26.2527734492731,-3.21959007219934,
-0.00242327538640976));
#41060=CARTESIAN_POINT('Ctrl Pts',(-26.2302954004745,-3.2221409144289,-0.367351620292292));
#41061=CARTESIAN_POINT('Ctrl Pts',(-26.1416596344333,-2.99639014349327,
-1.80328044297311));
#41062=CARTESIAN_POINT('Ctrl Pts',(-25.9868661511494,-0.883985791987881,
-3.70521989087602));
#41063=CARTESIAN_POINT('Ctrl Pts',(-25.7883929994212,2.63371395382021,-2.75202400600582));
#41064=CARTESIAN_POINT('Ctrl Pts',(-25.5899198476931,3.74046442819159,0.720424306650572));
#41065=CARTESIAN_POINT('Ctrl Pts',(-25.3914466959649,1.42312627862469,3.53338321092794));
#41066=CARTESIAN_POINT('Ctrl Pts',(-25.195731229825,-2.14666794500629,3.11767679330578));
#41067=CARTESIAN_POINT('Ctrl Pts',(-25.0661734809277,-3.22430720940184,
1.02174986004855));
#41068=CARTESIAN_POINT('Ctrl Pts',(-25.0027734492731,-3.22778696626011,
-0.000818109748633739));
#41069=CARTESIAN_POINT('Ctrl Pts',(-26.0062265507269,-3.22789335144083,
-0.000621618279895882));
#41070=CARTESIAN_POINT('Ctrl Pts',(-26.0041453259463,-3.22798218375112,
-0.0341863611775746));
#41071=CARTESIAN_POINT('Ctrl Pts',(-25.9359063839229,-3.21230194639243,
-1.13461799097082));
#41072=CARTESIAN_POINT('Ctrl Pts',(-25.8015097246568,-1.9642559671063,-3.26370692897528));
#41073=CARTESIAN_POINT('Ctrl Pts',(-25.6030365729288,1.67693807707542,-3.4202285169574));
#41074=CARTESIAN_POINT('Ctrl Pts',(-25.4045634212006,3.78303274977641,-0.445811211919431));
#41075=CARTESIAN_POINT('Ctrl Pts',(-25.2060902694725,2.42607098893233,2.93670971994425));
#41076=CARTESIAN_POINT('Ctrl Pts',(-25.0076171177444,-1.15175992694511,
3.63091358933775));
#41077=CARTESIAN_POINT('Ctrl Pts',(-24.8576625448291,-3.05835901460307,
1.64414342660099));
#41078=CARTESIAN_POINT('Ctrl Pts',(-24.7738656891567,-3.2241951435345,0.288812522806601));
#41079=CARTESIAN_POINT('Ctrl Pts',(-24.7562265507269,-3.22167406644033,
0.00291166086733272));
#41080=CARTESIAN_POINT('Origin',(-56.8777734492732,0.,0.));
#41081=CARTESIAN_POINT('',(-27.5027734492731,-3.21906218437362,0.00217345376617098));
#41082=CARTESIAN_POINT('',(-27.2562265507269,-3.21985095291246,-0.00252303240216523));
#41083=CARTESIAN_POINT('',(-56.8777734492732,-3.22275,1.66140794472856E-12));
#41084=CARTESIAN_POINT('Ctrl Pts',(-27.5027734492731,-3.21906218437362,
0.00217345376617089));
#41085=CARTESIAN_POINT('Ctrl Pts',(-27.4605750372641,-3.21481218592836,
-0.683195035194659));
#41086=CARTESIAN_POINT('Ctrl Pts',(-27.3522189080125,-2.66479263286037,
-2.44929786227344));
#41087=CARTESIAN_POINT('Ctrl Pts',(-27.1777050615181,0.240489146638442,
-3.80161153861474));
#41088=CARTESIAN_POINT('Ctrl Pts',(-26.9792319097899,3.32449393969521,-1.85952288641721));
#41089=CARTESIAN_POINT('Ctrl Pts',(-26.7807587580619,3.36519699902431,1.78480656597217));
#41090=CARTESIAN_POINT('Ctrl Pts',(-26.5822856063336,0.325338009741355,
3.79529188595517));
#41091=CARTESIAN_POINT('Ctrl Pts',(-26.4062905034042,-2.634332868274,2.49728024707007));
#41092=CARTESIAN_POINT('Ctrl Pts',(-26.2964531177173,-3.21463323880872,
0.706710744840075));
#41093=CARTESIAN_POINT('Ctrl Pts',(-26.2527734492731,-3.21959007219934,
-0.00242327538640976));
#41094=CARTESIAN_POINT('Ctrl Pts',(-27.2562265507269,-3.21985095291246,
-0.00252303240216523));
#41095=CARTESIAN_POINT('Ctrl Pts',(-27.2344249627358,-3.22244081034009,
-0.356396858653335));
#41096=CARTESIAN_POINT('Ctrl Pts',(-27.1464656575021,-3.00548259499999,
-1.78102692704359));
#41097=CARTESIAN_POINT('Ctrl Pts',(-26.9923486350256,-0.921735281371103,
-3.69600980702566));
#41098=CARTESIAN_POINT('Ctrl Pts',(-26.7938754832976,2.60550451902449,-2.77874623236759));
#41099=CARTESIAN_POINT('Ctrl Pts',(-26.5954023315693,3.74761847355685,0.682231778217214));
#41100=CARTESIAN_POINT('Ctrl Pts',(-26.3969291798413,1.45909486194852,3.51868251002977));
#41101=CARTESIAN_POINT('Ctrl Pts',(-26.2005372528937,-2.12710644928032,
3.13810092564533));
#41102=CARTESIAN_POINT('Ctrl Pts',(-26.070303043189,-3.22515839320196,1.0327655560849));
#41103=CARTESIAN_POINT('Ctrl Pts',(-26.0062265507269,-3.22789335144083,
-0.000621618279895882));
#41104=CARTESIAN_POINT('Origin',(-56.8777734492732,0.,0.));
#41105=CARTESIAN_POINT('',(-28.7527734492731,-3.22746554720106,0.00123150883681248));
#41106=CARTESIAN_POINT('',(-28.5062265507269,-3.21884251806067,0.00204608467250691));
#41107=CARTESIAN_POINT('',(-56.8777734492732,-3.22275,1.66140794472856E-12));
#41108=CARTESIAN_POINT('Ctrl Pts',(-28.7527734492731,-3.22746554720106,
0.00123150883681244));
#41109=CARTESIAN_POINT('Ctrl Pts',(-28.6908546740537,-3.22258522547558,
-0.997710618875136));
#41110=CARTESIAN_POINT('Ctrl Pts',(-28.5627781815916,-2.18882495849549,
-3.07270221306961));
#41111=CARTESIAN_POINT('Ctrl Pts',(-28.3685439718869,1.34385328587831,-3.56428725921659));
#41112=CARTESIAN_POINT('Ctrl Pts',(-28.1700708201588,3.72344069482658,-0.803787728376804));
#41113=CARTESIAN_POINT('Ctrl Pts',(-27.9715976684306,2.69452331250517,2.69251359115343));
#41114=CARTESIAN_POINT('Ctrl Pts',(-27.7731245167025,-0.801009325330438,
3.72403939035468));
#41115=CARTESIAN_POINT('Ctrl Pts',(-27.6168497769833,-2.97598203878223,
1.85201076842463));
#41116=CARTESIAN_POINT('Ctrl Pts',(-27.5267327545069,-3.22147523749922,
0.391310201877));
#41117=CARTESIAN_POINT('Ctrl Pts',(-27.5027734492731,-3.21906218437362,
0.00217345376617089));
#41118=CARTESIAN_POINT('Ctrl Pts',(-28.5062265507269,-3.21884251806067,
0.00204608467250695));
#41119=CARTESIAN_POINT('Ctrl Pts',(-28.4647045995254,-3.21492241651639,
-0.672451064148926));
#41120=CARTESIAN_POINT('Ctrl Pts',(-28.3570249310813,-2.67843067685807,
-2.42734436139883));
#41121=CARTESIAN_POINT('Ctrl Pts',(-28.1831875453944,0.201697865006982,
-3.80386676867179));
#41122=CARTESIAN_POINT('Ctrl Pts',(-27.9847143936663,3.30535260103752,-1.89333795329003));
#41123=CARTESIAN_POINT('Ctrl Pts',(-27.7862412419381,3.38322793010033,1.75038658459866));
#41124=CARTESIAN_POINT('Ctrl Pts',(-27.5877680902101,0.364035370925649,
3.79177566204397));
#41125=CARTESIAN_POINT('Ctrl Pts',(-27.4110965264729,-2.62014813522317,
2.51914926709635));
#41126=CARTESIAN_POINT('Ctrl Pts',(-27.3005826799786,-3.21458179312233,
0.717446227746891));
#41127=CARTESIAN_POINT('Ctrl Pts',(-27.2562265507269,-3.21985095291246,
-0.00252303240216523));
#41128=CARTESIAN_POINT('Origin',(-56.8777734492732,0.,0.));
#41129=CARTESIAN_POINT('',(-30.0027734492731,-3.22271626523272,-0.002945234897088));
#41130=CARTESIAN_POINT('',(-29.7562265507269,-3.22728206048765,0.00141062354910213));
#41131=CARTESIAN_POINT('',(-56.8777734492732,-3.22275,1.66140794472856E-12));
#41132=CARTESIAN_POINT('Ctrl Pts',(-30.0027734492731,-3.22271626523272,
-0.00294523489708803));
#41133=CARTESIAN_POINT('Ctrl Pts',(-29.987292028086,-3.22501767013846,-0.253666310298777));
#41134=CARTESIAN_POINT('Ctrl Pts',(-29.9056528896563,-3.08373759365553,
-1.57324436536649));
#41135=CARTESIAN_POINT('Ctrl Pts',(-29.7578560339838,-1.26927074168613,
-3.59152295057115));
#41136=CARTESIAN_POINT('Ctrl Pts',(-29.5593828822556,2.32925028389996,-3.01408003130834));
#41137=CARTESIAN_POINT('Ctrl Pts',(-29.3609097305275,3.79553357470212,0.322506129381382));
#41138=CARTESIAN_POINT('Ctrl Pts',(-29.1624365787994,1.78731695127927,3.36386436050109));
#41139=CARTESIAN_POINT('Ctrl Pts',(-28.9639634270713,-1.85704185655309,
3.32588046435669));
#41140=CARTESIAN_POINT('Ctrl Pts',(-28.8274090505625,-3.19482911305915,
1.20500740939856));
#41141=CARTESIAN_POINT('Ctrl Pts',(-28.7570123912965,-3.22779965266062,
0.0696188073427509));
#41142=CARTESIAN_POINT('Ctrl Pts',(-28.7527734492731,-3.22746554720106,
0.00123150883681244));
#41143=CARTESIAN_POINT('Ctrl Pts',(-29.7562265507269,-3.22728206048765,
0.00141062354910211));
#41144=CARTESIAN_POINT('Ctrl Pts',(-29.694984236315,-3.22186222518609,-0.986767058927104));
#41145=CARTESIAN_POINT('Ctrl Pts',(-29.5675842046605,-2.20776927460923,
-3.05205235830958));
#41146=CARTESIAN_POINT('Ctrl Pts',(-29.3740264557631,1.30742541749708,-3.57780983287773));
#41147=CARTESIAN_POINT('Ctrl Pts',(-29.1755533040351,3.71504773171258,-0.841727256093824));
#41148=CARTESIAN_POINT('Ctrl Pts',(-28.9770801523069,2.72184832452091,2.66488763756686));
#41149=CARTESIAN_POINT('Ctrl Pts',(-28.7786070005788,-0.762980147188692,
3.732016307246));
#41150=CARTESIAN_POINT('Ctrl Pts',(-28.6216558000521,-2.96643236631015,
1.87426426718019));
#41151=CARTESIAN_POINT('Ctrl Pts',(-28.5308623167682,-3.22116838911703,
0.402238114985581));
#41152=CARTESIAN_POINT('Ctrl Pts',(-28.5062265507269,-3.21884251806067,
0.00204608467250695));
#41153=CARTESIAN_POINT('Origin',(-56.8777734492732,0.,0.));
#41154=CARTESIAN_POINT('',(-31.2527734492731,-3.21755572586831,0.000563448608700447));
#41155=CARTESIAN_POINT('',(-31.0062265507269,-3.22304863623215,-0.00293073635939056));
#41156=CARTESIAN_POINT('',(-56.8777734492732,-3.22275,1.66140794472856E-12));
#41157=CARTESIAN_POINT('Ctrl Pts',(-31.2527734492731,-3.21755572586831,
0.000563448608700487));
#41158=CARTESIAN_POINT('Ctrl Pts',(-31.2175716648756,-3.21666178478838,
-0.571839069851177));
#41159=CARTESIAN_POINT('Ctrl Pts',(-31.1162121632355,-2.7977911693512,-2.22122822227451));
#41160=CARTESIAN_POINT('Ctrl Pts',(-30.9486949443525,-0.16119973612574,
-3.80579820343283));
#41161=CARTESIAN_POINT('Ctrl Pts',(-30.7502217926245,3.11017927930475,-2.19928856014008));
#41162=CARTESIAN_POINT('Ctrl Pts',(-30.5517486408963,3.53444406784637,1.42048951120562));
#41163=CARTESIAN_POINT('Ctrl Pts',(-30.3532754891682,0.723214987379329,
3.73992585517541));
#41164=CARTESIAN_POINT('Ctrl Pts',(-30.1702837586271,-2.4791338182994,2.72189388402554));
#41165=CARTESIAN_POINT('Ctrl Pts',(-30.0534497453287,-3.21518293383258,
0.817755609742787));
#41166=CARTESIAN_POINT('Ctrl Pts',(-30.0027734492731,-3.22271626523272,
-0.00294523489708803));
#41167=CARTESIAN_POINT('Ctrl Pts',(-31.0062265507269,-3.22304863623215,
-0.00293073635939122));
#41168=CARTESIAN_POINT('Ctrl Pts',(-30.9914215903473,-3.22525997788838,
-0.242633256256471));
#41169=CARTESIAN_POINT('Ctrl Pts',(-30.9104589127251,-3.09141502618626,
-1.551028275585));
#41170=CARTESIAN_POINT('Ctrl Pts',(-30.7633385178601,-1.30584039539486,
-3.57838864355298));
#41171=CARTESIAN_POINT('Ctrl Pts',(-30.5648653661319,2.29838356734553,-3.03768289982842));
#41172=CARTESIAN_POINT('Ctrl Pts',(-30.3663922144039,3.79862574454081,0.283772577015008));
#41173=CARTESIAN_POINT('Ctrl Pts',(-30.1679190626757,1.82153737945105,3.34545751696486));
#41174=CARTESIAN_POINT('Ctrl Pts',(-29.9694459109477,-1.82301916741003,
3.34465028632439));
#41175=CARTESIAN_POINT('Ctrl Pts',(-29.8322150736313,-3.18910491711469,
1.2270956905746));
#41176=CARTESIAN_POINT('Ctrl Pts',(-29.7611419535577,-3.22771706484762,
0.080723291995476));
#41177=CARTESIAN_POINT('Ctrl Pts',(-29.7562265507269,-3.22728206048765,
0.00141062354910211));
#41178=CARTESIAN_POINT('Origin',(-56.8777734492732,0.,0.));
#41179=CARTESIAN_POINT('',(-32.5027734492731,-3.22478385912128,0.00265457541594172));
#41180=CARTESIAN_POINT('',(-32.2562265507269,-3.21750741052827,0.00038513969681353));
#41181=CARTESIAN_POINT('',(-56.8777734492732,-3.22275,1.66140794472856E-12));
#41182=CARTESIAN_POINT('Ctrl Pts',(-32.5027734492731,-3.22478385912128,
0.00265457541594166));
#41183=CARTESIAN_POINT('Ctrl Pts',(-32.4478513016652,-3.21689735745027,
-0.885341341109883));
#41184=CARTESIAN_POINT('Ctrl Pts',(-32.3267714368147,-2.37556273920755,
-2.85611887470812));
#41185=CARTESIAN_POINT('Ctrl Pts',(-32.1395338547213,0.961021826073252,
-3.68599001219353));
#41186=CARTESIAN_POINT('Ctrl Pts',(-31.9410607029932,3.61808817488804,-1.19143748426638));
#41187=CARTESIAN_POINT('Ctrl Pts',(-31.7425875512651,2.96309132998079,2.39377841296397));
#41188=CARTESIAN_POINT('Ctrl Pts',(-31.5441143995369,-0.404372779207533,
3.78768636183299));
#41189=CARTESIAN_POINT('Ctrl Pts',(-31.3808430322063,-2.87005783900842,
2.08202372962302));
#41190=CARTESIAN_POINT('Ctrl Pts',(-31.2837293821183,-3.21834184454131,
0.503925827112667));
#41191=CARTESIAN_POINT('Ctrl Pts',(-31.2527734492731,-3.21755572586831,
0.000563448608700487));
#41192=CARTESIAN_POINT('Ctrl Pts',(-32.2562265507269,-3.21750741052827,
0.000385139696813461));
#41193=CARTESIAN_POINT('Ctrl Pts',(-32.2217012271369,-3.21690860986362,
-0.561038684184639));
#41194=CARTESIAN_POINT('Ctrl Pts',(-32.1210181863043,-2.80972226202356,
-2.19908042246798));
#41195=CARTESIAN_POINT('Ctrl Pts',(-31.9541774282289,-0.200012812968363,
-3.80395574332859));
#41196=CARTESIAN_POINT('Ctrl Pts',(-31.7557042765008,3.08758327993605,-2.23089979873894));
#41197=CARTESIAN_POINT('Ctrl Pts',(-31.5572311247726,3.54874993145618,1.38436207205476));
#41198=CARTESIAN_POINT('Ctrl Pts',(-31.3587579730445,0.761326868309329,
3.73235392509128));
#41199=CARTESIAN_POINT('Ctrl Pts',(-31.1750897816959,-2.4631155885873,2.74339848566718));
#41200=CARTESIAN_POINT('Ctrl Pts',(-31.05757930759,-3.21537833604205,0.828505816538859));
#41201=CARTESIAN_POINT('Ctrl Pts',(-31.0062265507269,-3.22304863623215,
-0.00293073635939122));
#41202=CARTESIAN_POINT('Origin',(-56.8777734492732,0.,0.));
#41203=CARTESIAN_POINT('',(-33.7527734492731,-3.22601040418458,-0.00222081755632452));
#41204=CARTESIAN_POINT('',(-33.5062265507269,-3.22446233910715,0.00273246397124949));
#41205=CARTESIAN_POINT('',(-56.8777734492732,-3.22275,1.66140794472856E-12));
#41206=CARTESIAN_POINT('Ctrl Pts',(-33.7527734492731,-3.22601040418458,
-0.00222081755632462));
#41207=CARTESIAN_POINT('Ctrl Pts',(-33.7442886556975,-3.22708935468399,
-0.139269568694677));
#41208=CARTESIAN_POINT('Ctrl Pts',(-33.6696461448792,-3.15691350318655,
-1.34380329108049));
#41209=CARTESIAN_POINT('Ctrl Pts',(-33.5288459168183,-1.64043970914924,
-3.43788348854727));
#41210=CARTESIAN_POINT('Ctrl Pts',(-33.3303727650901,1.99888224657508,-3.24261546972602));
#41211=CARTESIAN_POINT('Ctrl Pts',(-33.131899613362,3.80839132946346,-0.0789987458582374));
#41212=CARTESIAN_POINT('Ctrl Pts',(-32.9334264616339,2.13163027743554,3.15693485528285));
#41213=CARTESIAN_POINT('Ctrl Pts',(-32.7349533099058,-1.49646358995037,
3.50295333170919));
#41214=CARTESIAN_POINT('Ctrl Pts',(-32.5914023057855,-3.12976997368095,
1.43391316872666));
#41215=CARTESIAN_POINT('Ctrl Pts',(-32.5140090189079,-3.22639722171832,
0.184314258988555));
#41216=CARTESIAN_POINT('Ctrl Pts',(-32.5027734492731,-3.22478385912128,
0.00265457541594166));
#41217=CARTESIAN_POINT('Ctrl Pts',(-33.5062265507269,-3.22446233910715,
0.00273246397124952));
#41218=CARTESIAN_POINT('Ctrl Pts',(-33.4519808639265,-3.21654358931584,
-0.874552402068785));
#41219=CARTESIAN_POINT('Ctrl Pts',(-33.3315774598834,-2.392549869961,-2.83485900261666));
#41220=CARTESIAN_POINT('Ctrl Pts',(-33.1450163385977,0.923372444839,-3.6956011352236));
#41221=CARTESIAN_POINT('Ctrl Pts',(-32.9465431868696,3.60574643173899,-1.22828217139039));
#41222=CARTESIAN_POINT('Ctrl Pts',(-32.7480700351414,2.98735507926837,2.36342845310018));
#41223=CARTESIAN_POINT('Ctrl Pts',(-32.5495968834133,-0.365715011353638,
3.79161403007012));
#41224=CARTESIAN_POINT('Ctrl Pts',(-32.3856490552751,-2.85895781632522,
2.10422941420904));
#41225=CARTESIAN_POINT('Ctrl Pts',(-32.2878589443796,-3.21805603676474,
0.514766398334013));
#41226=CARTESIAN_POINT('Ctrl Pts',(-32.2562265507269,-3.21750741052827,
0.000385139696813461));
#41227=CARTESIAN_POINT('Origin',(-56.8777734492732,0.,0.));
#41228=CARTESIAN_POINT('',(-35.0027734492731,-3.21793583222462,-0.00126067022288214));
#41229=CARTESIAN_POINT('',(-34.7562265507269,-3.22628460838897,-0.0020870326190342));
#41230=CARTESIAN_POINT('',(-56.8777734492732,-3.22275,1.66140794472856E-12));
#41231=CARTESIAN_POINT('Ctrl Pts',(-35.0027734492731,-3.21793583222462,
-0.00126067022288179));
#41232=CARTESIAN_POINT('Ctrl Pts',(-34.9745682924871,-3.21954919455613,
-0.459758487032632));
#41233=CARTESIAN_POINT('Ctrl Pts',(-34.8802054184584,-2.91361395473245,
-1.99164958121414));
#41234=CARTESIAN_POINT('Ctrl Pts',(-34.719684827187,-0.56109586298945,-3.76765932015034));
#41235=CARTESIAN_POINT('Ctrl Pts',(-34.521211675459,2.86127528031798,-2.51459521402966));
#41236=CARTESIAN_POINT('Ctrl Pts',(-34.3227385237307,3.66438340819573,1.04037471995407));
#41237=CARTESIAN_POINT('Ctrl Pts',(-34.1242653720026,1.1130488505117,3.64296686459735));
#41238=CARTESIAN_POINT('Ctrl Pts',(-33.9342770138501,-2.30456177240892,
2.9420251518518));
#41239=CARTESIAN_POINT('Ctrl Pts',(-33.8104463729402,-3.21867655106971,
0.929328322994788));
#41240=CARTESIAN_POINT('Ctrl Pts',(-33.7527734492731,-3.22601040418458,
-0.00222081755632462));
#41241=CARTESIAN_POINT('Ctrl Pts',(-34.7562265507269,-3.22628460838897,
-0.0020870326190342));
#41242=CARTESIAN_POINT('Ctrl Pts',(-34.7484182179588,-3.22723246148271,
-0.128181329246406));
#41243=CARTESIAN_POINT('Ctrl Pts',(-34.674452167948,-3.16327403099888,-1.32166548379005));
#41244=CARTESIAN_POINT('Ctrl Pts',(-34.5343284006946,-1.67542282389703,
-3.42097102935977));
#41245=CARTESIAN_POINT('Ctrl Pts',(-34.3358552489665,1.96570152728694,-3.26283648505036));
#41246=CARTESIAN_POINT('Ctrl Pts',(-34.1373820972383,3.80738723472595,-0.117842553434008));
#41247=CARTESIAN_POINT('Ctrl Pts',(-33.9389089455102,2.16372197368752,3.13502657773993));
#41248=CARTESIAN_POINT('Ctrl Pts',(-33.740435793782,-1.46065342046419,3.51803581673643));
#41249=CARTESIAN_POINT('Ctrl Pts',(-33.5962083288543,-3.12277599809849,
1.45609309127958));
#41250=CARTESIAN_POINT('Ctrl Pts',(-33.5181385811692,-3.22620124950064,
0.195379006899928));
#41251=CARTESIAN_POINT('Ctrl Pts',(-33.5062265507269,-3.22446233910715,
0.00273246397124952));
#41252=CARTESIAN_POINT('Origin',(-56.8777734492732,0.,0.));
#41253=CARTESIAN_POINT('',(-36.2527734492731,-3.22139608804363,0.00288158050599253));
#41254=CARTESIAN_POINT('',(-36.0062265507269,-3.21807312213843,-0.0014220418686986));
#41255=CARTESIAN_POINT('',(-56.8777734492732,-3.22275,1.66140794472856E-12));
#41256=CARTESIAN_POINT('Ctrl Pts',(-36.2527734492731,-3.22139608804363,
0.00288158050599251));
#41257=CARTESIAN_POINT('Ctrl Pts',(-36.2048479292767,-3.2146635292965,-0.774081151249586));
#41258=CARTESIAN_POINT('Ctrl Pts',(-36.0907646920376,-2.54241255560425,
-2.63403211011377));
#41259=CARTESIAN_POINT('Ctrl Pts',(-35.9105237375558,0.567502522785501,
-3.76669964382771));
#41260=CARTESIAN_POINT('Ctrl Pts',(-35.7120505858277,3.472497692532,-1.5658368674736));
#41261=CARTESIAN_POINT('Ctrl Pts',(-35.5135774340996,3.19870582288421,2.06842122857658));
#41262=CARTESIAN_POINT('Ctrl Pts',(-35.3151042823714,-0.00323906886257519,
3.80920921302736));
#41263=CARTESIAN_POINT('Ctrl Pts',(-35.1448362874292,-2.74760962933859,
2.31113643119006));
#41264=CARTESIAN_POINT('Ctrl Pts',(-35.0407260097298,-3.21576490894666,
0.61568913948014));
#41265=CARTESIAN_POINT('Ctrl Pts',(-35.0027734492731,-3.21793583222462,
-0.00126067022288179));
#41266=CARTESIAN_POINT('Ctrl Pts',(-36.0062265507269,-3.21807312213843,
-0.0014220418686987));
#41267=CARTESIAN_POINT('Ctrl Pts',(-35.9786978547484,-3.21985374816276,
-0.448875666670094));
#41268=CARTESIAN_POINT('Ctrl Pts',(-35.8850114415272,-2.92394127391821,
-1.96941039752039));
#41269=CARTESIAN_POINT('Ctrl Pts',(-35.7251673110634,-0.599499081901595,
-3.76173966049661));
#41270=CARTESIAN_POINT('Ctrl Pts',(-35.5266941593352,2.83547591786548,-2.54365106525228));
#41271=CARTESIAN_POINT('Ctrl Pts',(-35.3282210076071,3.67480510407022,1.0029416082971));
#41272=CARTESIAN_POINT('Ctrl Pts',(-35.1297478558789,1.15015139627886,3.6314234382941));
#41273=CARTESIAN_POINT('Ctrl Pts',(-34.9390830369189,-2.28662470261192,
2.96300846018566));
#41274=CARTESIAN_POINT('Ctrl Pts',(-34.8145759352015,-3.21920157975339,
0.940178725324924));
#41275=CARTESIAN_POINT('Ctrl Pts',(-34.7562265507269,-3.22628460838897,
-0.0020870326190342));
#41276=CARTESIAN_POINT('Origin',(-56.8777734492732,0.,0.));
#41277=CARTESIAN_POINT('',(-37.5027734492731,-3.22796415037744,-0.00044646271146332));
#41278=CARTESIAN_POINT('',(-37.2562265507269,-3.2210849165079,0.00283661979922523));
#41279=CARTESIAN_POINT('',(-56.8777734492732,-3.22275,1.66140794472856E-12));
#41280=CARTESIAN_POINT('Ctrl Pts',(-37.5027734492731,-3.22796415037744,
-0.000446462711463694));
#41281=CARTESIAN_POINT('Ctrl Pts',(-37.501285283309,-3.22801075358026,-0.0244452988629991));
#41282=CARTESIAN_POINT('Ctrl Pts',(-37.4336394001022,-3.2168973996266,-1.11528905868563));
#41283=CARTESIAN_POINT('Ctrl Pts',(-37.2998357996528,-1.99336480079335,
-3.24601018038109));
#41284=CARTESIAN_POINT('Ctrl Pts',(-37.1013626479246,1.64628397471009,-3.43508870260906));
#41285=CARTESIAN_POINT('Ctrl Pts',(-36.9028894961965,3.77889469710683,-0.479625049760291));
#41286=CARTESIAN_POINT('Ctrl Pts',(-36.7044163444683,2.45223703403194,2.9148960271512));
#41287=CARTESIAN_POINT('Ctrl Pts',(-36.5059431927402,-1.11924265385457,
3.64106868954325));
#41288=CARTESIAN_POINT('Ctrl Pts',(-36.3553955610085,-3.05114365842598,
1.66363885049783));
#41289=CARTESIAN_POINT('Ctrl Pts',(-36.2710056465194,-3.22395734015022,
0.2984597563813));
#41290=CARTESIAN_POINT('Ctrl Pts',(-36.2527734492731,-3.22139608804363,
0.00288158050599251));
#41291=CARTESIAN_POINT('Ctrl Pts',(-37.2562265507269,-3.2210849165079,0.00283661979922505));
#41292=CARTESIAN_POINT('Ctrl Pts',(-37.208977491538,-3.21459943825884,-0.763347069727803));
#41293=CARTESIAN_POINT('Ctrl Pts',(-37.0955707151064,-2.55752111380778,
-2.61233066684471));
#41294=CARTESIAN_POINT('Ctrl Pts',(-36.9160062214322,0.529050339993744,
-3.77229242772965));
#41295=CARTESIAN_POINT('Ctrl Pts',(-36.717533069704,3.45634442597985,-1.60117695198001));
#41296=CARTESIAN_POINT('Ctrl Pts',(-36.5190599179759,3.21963846421469,2.03568479443731));
#41297=CARTESIAN_POINT('Ctrl Pts',(-36.3205867662477,0.0356173628047984,
3.80904395170505));
#41298=CARTESIAN_POINT('Ctrl Pts',(-36.1496423104981,-2.73485489133519,
2.33320322322453));
#41299=CARTESIAN_POINT('Ctrl Pts',(-36.0448555719911,-3.21557449886142,
0.626457157376317));
#41300=CARTESIAN_POINT('Ctrl Pts',(-36.0062265507269,-3.21807312213843,
-0.0014220418686987));
#41301=CARTESIAN_POINT('Origin',(-56.8777734492732,0.,0.));
#41302=CARTESIAN_POINT('',(-38.7527734492731,-3.22008925450213,-0.0026026082531262));
#41303=CARTESIAN_POINT('',(-38.5062265507269,-3.22801732889799,-0.000244327765261954));
#41304=CARTESIAN_POINT('',(-56.8777734492732,-3.22275,1.66140794472856E-12));
#41305=CARTESIAN_POINT('Ctrl Pts',(-38.7527734492731,-3.22008925450213,
-0.00260260825312667));
#41306=CARTESIAN_POINT('Ctrl Pts',(-38.7315649200986,-3.22270124067416,
-0.346785967826072));
#41307=CARTESIAN_POINT('Ctrl Pts',(-38.6441986736814,-3.01333795851248,
-1.76151821125225));
#41308=CARTESIAN_POINT('Ctrl Pts',(-38.4906747100216,-0.954751856070833,
-3.68761904397796));
#41309=CARTESIAN_POINT('Ctrl Pts',(-38.2922015582933,2.58055008692402,-2.80193621787794));
#41310=CARTESIAN_POINT('Ctrl Pts',(-38.0937284065653,3.7535699214344,0.648689575284357));
#41311=CARTESIAN_POINT('Ctrl Pts',(-37.895255254837,1.4905041270395,3.50549322741577));
#41312=CARTESIAN_POINT('Ctrl Pts',(-37.6982702690731,-2.10979678019673,
3.15594586387091));
#41313=CARTESIAN_POINT('Ctrl Pts',(-37.5674430005517,-3.22593896750995,
1.04244391550343));
#41314=CARTESIAN_POINT('Ctrl Pts',(-37.5027734492731,-3.22796415037744,
-0.000446462711463694));
#41315=CARTESIAN_POINT('Ctrl Pts',(-38.5062265507269,-3.22801732889799,
-0.000244327765261728));
#41316=CARTESIAN_POINT('Ctrl Pts',(-38.5054148455703,-3.22803159826031,
-0.0133336695831677));
#41317=CARTESIAN_POINT('Ctrl Pts',(-38.438445423171,-3.22203104550765,-1.09325134200945));
#41318=CARTESIAN_POINT('Ctrl Pts',(-38.3053182835291,-2.02637231772134,
-3.22550765811006));
#41319=CARTESIAN_POINT('Ctrl Pts',(-38.1068451318009,1.6111582665074,-3.45170298009821));
#41320=CARTESIAN_POINT('Ctrl Pts',(-37.9083719800728,3.77380550466478,-0.518147117637242));
#41321=CARTESIAN_POINT('Ctrl Pts',(-37.7098988283447,2.48184309593248,2.88972996484555));
#41322=CARTESIAN_POINT('Ctrl Pts',(-37.5114256766165,-1.082043260835,3.65229610029575));
#41323=CARTESIAN_POINT('Ctrl Pts',(-37.3602015840773,-3.04278554668972,
1.6858795326344));
#41324=CARTESIAN_POINT('Ctrl Pts',(-37.2751352087807,-3.22368034788013,
0.30945659573954));
#41325=CARTESIAN_POINT('Ctrl Pts',(-37.2562265507269,-3.2210849165079,0.00283661979922505));
#41326=CARTESIAN_POINT('Origin',(-56.8777734492732,0.,0.));
#41327=CARTESIAN_POINT('',(-40.0027734492731,-3.21866195397384,0.00192812909354238));
#41328=CARTESIAN_POINT('',(-39.7562265507269,-3.2203708227658,-0.00268402097280518));
#41329=CARTESIAN_POINT('',(-56.8777734492732,-3.22275,1.66140794472856E-12));
#41330=CARTESIAN_POINT('Ctrl Pts',(-40.0027734492731,-3.21866195397384,
0.00192812909354245));
#41331=CARTESIAN_POINT('Ctrl Pts',(-39.9618445568882,-3.21503311819019,
-0.663028774388865));
#41332=CARTESIAN_POINT('Ctrl Pts',(-39.8547579472606,-2.69024800802762,
-2.40807795997689));
#41333=CARTESIAN_POINT('Ctrl Pts',(-39.6815136203903,0.16767183512014,-3.80551855545168));
#41334=CARTESIAN_POINT('Ctrl Pts',(-39.4830404686621,3.28828840795416,-1.92282205788625));
#41335=CARTESIAN_POINT('Ctrl Pts',(-39.284567316934,3.39874644404531,1.72006044349292));
#41336=CARTESIAN_POINT('Ctrl Pts',(-39.0860941652058,0.397930664244868,
3.78836858114853));
#41337=CARTESIAN_POINT('Ctrl Pts',(-38.9088295426523,-2.60756993467388,
2.53829833231303));
#41338=CARTESIAN_POINT('Ctrl Pts',(-38.7977226373413,-3.21455343178135,
0.726856866852839));
#41339=CARTESIAN_POINT('Ctrl Pts',(-38.7527734492731,-3.22008925450213,
-0.00260260825312667));
#41340=CARTESIAN_POINT('Ctrl Pts',(-39.7562265507269,-3.2203708227658,-0.00268402097280518));
#41341=CARTESIAN_POINT('Ctrl Pts',(-39.7356944823599,-3.22299454943295,
-0.335815833202966));
#41342=CARTESIAN_POINT('Ctrl Pts',(-39.6490046967502,-3.02216610517768,
-1.73926753296821));
#41343=CARTESIAN_POINT('Ctrl Pts',(-39.4961571938978,-0.992318122077262,
-3.67768801927938));
#41344=CARTESIAN_POINT('Ctrl Pts',(-39.2976840421697,2.55183428468159,-2.82811354193527));
#41345=CARTESIAN_POINT('Ctrl Pts',(-39.0992108904416,3.7599915464262,0.610367097210888));
#41346=CARTESIAN_POINT('Ctrl Pts',(-38.9007377387134,1.52618470788745,3.4901066831781));
#41347=CARTESIAN_POINT('Ctrl Pts',(-38.7030762921419,-2.08986966660851,
3.17622859575436));
#41348=CARTESIAN_POINT('Ctrl Pts',(-38.571572562813,-3.22686857936123,1.05350811141649));
#41349=CARTESIAN_POINT('Ctrl Pts',(-38.5062265507269,-3.22801732889799,
-0.000244327765261728));
#41350=CARTESIAN_POINT('Origin',(-56.8777734492732,0.,0.));
#41351=CARTESIAN_POINT('',(-41.2527734492731,-3.22710433633706,0.00156176513451752));
#41352=CARTESIAN_POINT('',(-41.0062265507269,-3.21846982119328,0.00178688758337556));
#41353=CARTESIAN_POINT('',(-56.8777734492732,-3.22275,1.66140794472856E-12));
#41354=CARTESIAN_POINT('Ctrl Pts',(-41.2527734492731,-3.22710433633706,
0.00156176513451766));
#41355=CARTESIAN_POINT('Ctrl Pts',(-41.1921241936778,-3.22126058887623,
-0.977189372262004));
#41356=CARTESIAN_POINT('Ctrl Pts',(-41.0653172208397,-2.2242198704757,-3.03389349971977));
#41357=CARTESIAN_POINT('Ctrl Pts',(-40.8723525307591,1.27537683100426,-3.58935917109407));
#41358=CARTESIAN_POINT('Ctrl Pts',(-40.6738793790308,3.70737171949489,-0.874917283901245));
#41359=CARTESIAN_POINT('Ctrl Pts',(-40.4754062273029,2.74557164665491,2.64043967044588));
#41360=CARTESIAN_POINT('Ctrl Pts',(-40.2769330755746,-0.72957424780644,
3.73869051101015));
#41361=CARTESIAN_POINT('Ctrl Pts',(-40.1193888162315,-2.95794074349924,
1.89377317364348));
#41362=CARTESIAN_POINT('Ctrl Pts',(-40.0280022741309,-3.22089879101215,
0.411811716906847));
#41363=CARTESIAN_POINT('Ctrl Pts',(-40.0027734492731,-3.21866195397384,
0.00192812909354245));
#41364=CARTESIAN_POINT('Ctrl Pts',(-41.0062265507269,-3.21846982119328,
0.00178688758337563));
#41365=CARTESIAN_POINT('Ctrl Pts',(-40.9659741191495,-3.21517429251383,
-0.652277557928967));
#41366=CARTESIAN_POINT('Ctrl Pts',(-40.8595639703294,-2.70356885076125,
-2.3860805065197));
#41367=CARTESIAN_POINT('Ctrl Pts',(-40.6869961042666,0.128844490289695,
-3.80703080101488));
#41368=CARTESIAN_POINT('Ctrl Pts',(-40.4885229525384,3.26850326385081,-1.95626451093675));
#41369=CARTESIAN_POINT('Ctrl Pts',(-40.2900498008104,3.41611517854965,1.68530160785441));
#41370=CARTESIAN_POINT('Ctrl Pts',(-40.0915766490822,0.436553624420728,
3.78411222819291));
#41371=CARTESIAN_POINT('Ctrl Pts',(-39.9136355657211,-2.59305936995176,
2.56011184016511));
#41372=CARTESIAN_POINT('Ctrl Pts',(-39.8018521996026,-3.21454046853544,
0.737589916483859));
#41373=CARTESIAN_POINT('Ctrl Pts',(-39.7562265507269,-3.2203708227658,-0.00268402097280518));
#41374=CARTESIAN_POINT('Origin',(-56.8777734492732,0.,0.));
#41375=CARTESIAN_POINT('',(-42.5027734492731,-3.223340812517,-0.00290808097893776));
#41376=CARTESIAN_POINT('',(-42.2562265507269,-3.22688342116564,0.00172679050016274));
#41377=CARTESIAN_POINT('',(-56.8777734492732,-3.22275,1.66140794472856E-12));
#41378=CARTESIAN_POINT('Ctrl Pts',(-42.5027734492731,-3.223340812517,-0.00290808097893728));
#41379=CARTESIAN_POINT('Ctrl Pts',(-42.4885615477101,-3.22546598349143,
-0.232955127105204));
#41380=CARTESIAN_POINT('Ctrl Pts',(-42.4081919289044,-3.09803786246336,
-1.53155634344338));
#41381=CARTESIAN_POINT('Ctrl Pts',(-42.261664592856,-1.33778973609199,-3.56656752945834));
#41382=CARTESIAN_POINT('Ctrl Pts',(-42.0631914411278,2.27112573740255,-3.05811595677589));
#41383=CARTESIAN_POINT('Ctrl Pts',(-41.8647182893997,3.80101173467418,0.249790138013328));
#41384=CARTESIAN_POINT('Ctrl Pts',(-41.6662451376716,1.8513830112441,3.32903383369054));
#41385=CARTESIAN_POINT('Ctrl Pts',(-41.4677719859434,-1.7930351237828,3.36081989476688));
#41386=CARTESIAN_POINT('Ctrl Pts',(-41.3299480898107,-3.18398887201866,
1.24646872161016));
#41387=CARTESIAN_POINT('Ctrl Pts',(-41.2582819109205,-3.22763509402649,
0.0904567243517276));
#41388=CARTESIAN_POINT('Ctrl Pts',(-41.2527734492731,-3.22710433633706,
0.00156176513451766));
#41389=CARTESIAN_POINT('Ctrl Pts',(-42.2562265507269,-3.22688342116564,
0.00172679050016271));
#41390=CARTESIAN_POINT('Ctrl Pts',(-42.1962537559391,-3.22061008171567,
-0.96628254910302));
#41391=CARTESIAN_POINT('Ctrl Pts',(-42.0701232439086,-2.24280389648251,
-3.01311945076458));
#41392=CARTESIAN_POINT('Ctrl Pts',(-41.8778350146354,1.2386967785751,-3.60218193784014));
#41393=CARTESIAN_POINT('Ctrl Pts',(-41.6793618629072,3.69825402795075,-0.912689195345268));
#41394=CARTESIAN_POINT('Ctrl Pts',(-41.4808887111792,2.77236281533892,2.61229570352975));
#41395=CARTESIAN_POINT('Ctrl Pts',(-41.2824155594509,-0.691399338080392,
3.7459379837173));
#41396=CARTESIAN_POINT('Ctrl Pts',(-41.1241948393002,-2.94811754240371,
1.91602372979707));
#41397=CARTESIAN_POINT('Ctrl Pts',(-41.0321318363922,-3.22059072690044,
0.42272360222518));
#41398=CARTESIAN_POINT('Ctrl Pts',(-41.0062265507269,-3.21846982119328,
0.00178688758337563));
#41399=CARTESIAN_POINT('Origin',(-56.8777734492732,0.,0.));
#41400=CARTESIAN_POINT('',(-43.7527734492731,-3.21748022116968,0.000227641132840197));
#41401=CARTESIAN_POINT('',(-43.5062265507269,-3.22367341548636,-0.0028708798850563));
#41402=CARTESIAN_POINT('',(-56.8777734492732,-3.22275,1.66140794472856E-12));
#41403=CARTESIAN_POINT('Ctrl Pts',(-43.7527734492731,-3.21748022116968,
0.000227641132840434));
#41404=CARTESIAN_POINT('Ctrl Pts',(-43.7188411844997,-3.2171325373007,-0.551564014624385));
#41405=CARTESIAN_POINT('Ctrl Pts',(-43.6187512024836,-2.82005117109617,
-2.17965269821368));
#41406=CARTESIAN_POINT('Ctrl Pts',(-43.4525035032247,-0.234023586811988,
-3.80201502903332));
#41407=CARTESIAN_POINT('Ctrl Pts',(-43.2540303514966,3.06750897389918,-2.25842290442415));
#41408=CARTESIAN_POINT('Ctrl Pts',(-43.0555571997685,3.5609884751578,1.35257029391188));
#41409=CARTESIAN_POINT('Ctrl Pts',(-42.8570840480403,0.794674878034206,
3.72539624179777));
#41410=CARTESIAN_POINT('Ctrl Pts',(-42.6728227978752,-2.44892272596741,
2.76221643248652));
#41411=CARTESIAN_POINT('Ctrl Pts',(-42.5547192649528,-3.21557311589762,
0.837935165982687));
#41412=CARTESIAN_POINT('Ctrl Pts',(-42.5027734492731,-3.223340812517,-0.00290808097893728));
#41413=CARTESIAN_POINT('Ctrl Pts',(-43.5062265507269,-3.22367341548636,
-0.00287087988505616));
#41414=CARTESIAN_POINT('Ctrl Pts',(-43.4926911099714,-3.22569286306808,
-0.22191002267826));
#41415=CARTESIAN_POINT('Ctrl Pts',(-43.4129979519732,-3.10546925677265,
-1.50935200779924));
#41416=CARTESIAN_POINT('Ctrl Pts',(-43.2671470767323,-1.3741012622493,-3.55273558594484));
#41417=CARTESIAN_POINT('Ctrl Pts',(-43.0686739250041,2.23981285336136,-3.0811236269373));
#41418=CARTESIAN_POINT('Ctrl Pts',(-42.8702007732761,3.80336187175512,0.211004490552806));
#41419=CARTESIAN_POINT('Ctrl Pts',(-42.6717276215479,1.88524481156147,3.30997529039638));
#41420=CARTESIAN_POINT('Ctrl Pts',(-42.4732544698198,-1.75865936318237,
3.37893499002941));
#41421=CARTESIAN_POINT('Ctrl Pts',(-42.3347541128794,-3.17804089141674,
1.26857508589703));
#41422=CARTESIAN_POINT('Ctrl Pts',(-42.2624114731818,-3.22753038314513,
0.10155643362859));
#41423=CARTESIAN_POINT('Ctrl Pts',(-42.2562265507269,-3.22688342116564,
0.00172679050016271));
#41424=CARTESIAN_POINT('Origin',(-56.8777734492732,0.,0.));
#41425=CARTESIAN_POINT('',(-45.0027734492731,-3.22417653578848,0.00279102537114976));
#41426=CARTESIAN_POINT('',(-44.7562265507269,-3.21746616228897,4.72427012537802E-5));
#41427=CARTESIAN_POINT('',(-56.8777734492732,-3.22275,1.66140794472856E-12));
#41428=CARTESIAN_POINT('Ctrl Pts',(-45.0027734492731,-3.22417653578848,
0.00279102537114981));
#41429=CARTESIAN_POINT('Ctrl Pts',(-44.9491208212893,-3.21625964967102,
-0.865101307677308));
#41430=CARTESIAN_POINT('Ctrl Pts',(-44.8293104760627,-2.40729031540785,
-2.81617952915074));
#41431=CARTESIAN_POINT('Ctrl Pts',(-44.6433424135935,0.890285797212397,
-3.70371118197161));
#41432=CARTESIAN_POINT('Ctrl Pts',(-44.4448692618654,3.5946178274591,-1.26047927182198));
#41433=CARTESIAN_POINT('Ctrl Pts',(-44.2463961101372,3.00837184347797,2.33661810562801));
#41434=CARTESIAN_POINT('Ctrl Pts',(-44.0479229584092,-0.331792003801605,
3.79473311135223));
#41435=CARTESIAN_POINT('Ctrl Pts',(-43.8833820714544,-2.84909864975645,
2.12369000224508));
#41436=CARTESIAN_POINT('Ctrl Pts',(-43.7849989017424,-3.21781041634141,
0.524263861358598));
#41437=CARTESIAN_POINT('Ctrl Pts',(-43.7527734492731,-3.21748022116968,
0.000227641132840434));
#41438=CARTESIAN_POINT('Ctrl Pts',(-44.7562265507269,-3.21746616228897,
4.72427012538842E-5));
#41439=CARTESIAN_POINT('Ctrl Pts',(-44.722970746761,-3.21739546247406,-0.54074993855212));
#41440=CARTESIAN_POINT('Ctrl Pts',(-44.6235572255524,-2.83168351011836,
-2.15748135685122));
#41441=CARTESIAN_POINT('Ctrl Pts',(-44.4579859871011,-0.272794281860559,
-3.79942991807168));
#41442=CARTESIAN_POINT('Ctrl Pts',(-44.2595128353729,3.04431198941514,-2.28959580137133));
#41443=CARTESIAN_POINT('Ctrl Pts',(-44.0610396836448,3.57460013936063,1.31617562135035));
#41444=CARTESIAN_POINT('Ctrl Pts',(-43.8625665319167,0.832634827927634,
3.71709613352627));
#41445=CARTESIAN_POINT('Ctrl Pts',(-43.677628820944,-2.43256230338299,2.78363876634131));
#41446=CARTESIAN_POINT('Ctrl Pts',(-43.5588488272141,-3.21582232804,0.848696390202636));
#41447=CARTESIAN_POINT('Ctrl Pts',(-43.5062265507269,-3.22367341548636,
-0.00287087988505616));
#41448=CARTESIAN_POINT('Origin',(-56.8777734492732,0.,0.));
#41449=CARTESIAN_POINT('',(-46.2527734492731,-3.22651385010114,-0.00196162169800456));
#41450=CARTESIAN_POINT('',(-46.0062265507269,-3.22384686894452,0.00284660154848987));
#41451=CARTESIAN_POINT('',(-56.8777734492732,-3.22275,1.66140794472856E-12));
#41452=CARTESIAN_POINT('Ctrl Pts',(-46.2527734492731,-3.22651385010114,
-0.00196162169800482));
#41453=CARTESIAN_POINT('Ctrl Pts',(-46.2455581753216,-3.22734896786933,
-0.118457092701875));
#41454=CARTESIAN_POINT('Ctrl Pts',(-46.1721851841273,-3.16874982256624,
-1.30226456697049));
#41455=CARTESIAN_POINT('Ctrl Pts',(-46.0326544756905,-1.70594961134342,
-3.40585103076117));
#41456=CARTESIAN_POINT('Ctrl Pts',(-45.8341813239623,1.93644344289748,-3.28028537061014));
#41457=CARTESIAN_POINT('Ctrl Pts',(-45.6357081722341,3.80618123172504,-0.151887298493708));
#41458=CARTESIAN_POINT('Ctrl Pts',(-45.4372350205061,2.19167204898115,3.11555114705157));
#41459=CARTESIAN_POINT('Ctrl Pts',(-45.2387618687778,-1.42913327008184,
3.53095786105198));
#41460=CARTESIAN_POINT('Ctrl Pts',(-45.0939413450337,-3.11653952747685,
1.47554470212732));
#41461=CARTESIAN_POINT('Ctrl Pts',(-45.015278538532,-3.22602176446174,0.205075079288332));
#41462=CARTESIAN_POINT('Ctrl Pts',(-45.0027734492731,-3.22417653578848,
0.00279102537114981));
#41463=CARTESIAN_POINT('Ctrl Pts',(-46.0062265507269,-3.22384686894453,
0.00284660154848976));
#41464=CARTESIAN_POINT('Ctrl Pts',(-45.9532503835506,-3.21596457240548,
-0.854328906569246));
#41465=CARTESIAN_POINT('Ctrl Pts',(-45.8341164991316,-2.42393033646003,
-2.79482768367397));
#41466=CARTESIAN_POINT('Ctrl Pts',(-45.6488248974699,0.852459331624162,
-3.71259983171912));
#41467=CARTESIAN_POINT('Ctrl Pts',(-45.4503517457417,3.5815730376942,-1.29708095283833));
#41468=CARTESIAN_POINT('Ctrl Pts',(-45.2518785940136,3.03205016544447,2.30580923252167));
#41469=CARTESIAN_POINT('Ctrl Pts',(-45.0534054422855,-0.29306613324189,
3.79792004445863));
#41470=CARTESIAN_POINT('Ctrl Pts',(-44.8881880945232,-2.83770608863998,
2.14587792408869));
#41471=CARTESIAN_POINT('Ctrl Pts',(-44.7891284640037,-3.21753610975382,
0.535089546179736));
#41472=CARTESIAN_POINT('Ctrl Pts',(-44.7562265507269,-3.21746616228897,
4.72427012538842E-5));
#41473=CARTESIAN_POINT('Origin',(-56.8777734492732,0.,0.));
#41474=CARTESIAN_POINT('',(-47.5027734492731,-3.2182073643014,-0.00155924202532693));
#41475=CARTESIAN_POINT('',(-47.2562265507269,-3.22676077824252,-0.00180977931619031));
#41476=CARTESIAN_POINT('',(-56.8777734492732,-3.22275,1.66140794472856E-12));
#41477=CARTESIAN_POINT('Ctrl Pts',(-47.5027734492731,-3.21820736430141,
-0.00155924202532676));
#41478=CARTESIAN_POINT('Ctrl Pts',(-47.4758378121112,-3.22012238586887,
-0.439327612385657));
#41479=CARTESIAN_POINT('Ctrl Pts',(-47.3827444577066,-2.93287246486136,
-1.94990972203441));
#41480=CARTESIAN_POINT('Ctrl Pts',(-47.2234933860592,-0.633116354570043,
-3.75622802845598));
#41481=CARTESIAN_POINT('Ctrl Pts',(-47.025020234331,2.81261475191178,-2.56890707841041));
#41482=CARTESIAN_POINT('Ctrl Pts',(-46.826547082603,3.68362756861194,0.970037760059602));
#41483=CARTESIAN_POINT('Ctrl Pts',(-46.6280739308748,1.18258124809755,3.62099253131349));
#41484=CARTESIAN_POINT('Ctrl Pts',(-46.4368160530982,-2.27074334009362,
2.98135593498794));
#41485=CARTESIAN_POINT('Ctrl Pts',(-46.3117158925643,-3.2196916723122,0.949703933825722));
#41486=CARTESIAN_POINT('Ctrl Pts',(-46.2527734492731,-3.22651385010114,
-0.00196162169800482));
#41487=CARTESIAN_POINT('Ctrl Pts',(-47.2562265507269,-3.22676077824252,
-0.00180977931619085));
#41488=CARTESIAN_POINT('Ctrl Pts',(-47.2496877375829,-3.22747103515158,
-0.10736207527441));
#41489=CARTESIAN_POINT('Ctrl Pts',(-47.1769912071962,-3.17488133388419,
-1.28014382472976));
#41490=CARTESIAN_POINT('Ctrl Pts',(-47.0381369595668,-1.74060256508747,
-3.38827199807887));
#41491=CARTESIAN_POINT('Ctrl Pts',(-46.8396638078386,1.90288171805956,-3.29986751092048));
#41492=CARTESIAN_POINT('Ctrl Pts',(-46.6411906561105,3.80443374423865,-0.190704767250943));
#41493=CARTESIAN_POINT('Ctrl Pts',(-46.4427175043824,2.22333848041998,3.09303256110211));
#41494=CARTESIAN_POINT('Ctrl Pts',(-46.2442443526542,-1.39304094239042,
3.54535207777422));
#41495=CARTESIAN_POINT('Ctrl Pts',(-46.0987473681024,-3.10930527441843,
1.49773850278433));
#41496=CARTESIAN_POINT('Ctrl Pts',(-46.0194081007933,-3.22580814496742,
0.21612933750686));
#41497=CARTESIAN_POINT('Ctrl Pts',(-46.0062265507269,-3.22384686894453,
0.00284660154848976));
#41498=CARTESIAN_POINT('Origin',(-56.8777734492732,0.,0.));
#41499=CARTESIAN_POINT('',(-48.7527734492731,-3.22081842851865,0.00278806351307224));
#41500=CARTESIAN_POINT('',(-48.5062265507269,-3.21837549758788,-0.00171032771080215));
#41501=CARTESIAN_POINT('',(-56.8777734492732,-3.22275,1.66140794472856E-12));
#41502=CARTESIAN_POINT('Ctrl Pts',(-48.7527734492731,-3.22081842851865,
0.00278806351307209));
#41503=CARTESIAN_POINT('Ctrl Pts',(-48.7061174489008,-3.21456284440464,
-0.75393734371017));
#41504=CARTESIAN_POINT('Ctrl Pts',(-48.5933037312858,-2.57062144258657,
-2.59327646914024));
#41505=CARTESIAN_POINT('Ctrl Pts',(-48.414332296428,0.495293598847041,-3.77687298849846));
#41506=CARTESIAN_POINT('Ctrl Pts',(-48.2158591446999,3.44188699455041,-1.63202305036004));
#41507=CARTESIAN_POINT('Ctrl Pts',(-48.0173859929717,3.23771493607145,2.00681023340388));
#41508=CARTESIAN_POINT('Ctrl Pts',(-47.8189128412436,0.0696802094731201,
3.80857322216686));
#41509=CARTESIAN_POINT('Ctrl Pts',(-47.6473753266774,-2.72353680500992,
2.35253380852171));
#41510=CARTESIAN_POINT('Ctrl Pts',(-47.5419955293539,-3.21541882327584,
0.635893140329142));
#41511=CARTESIAN_POINT('Ctrl Pts',(-47.5027734492731,-3.21820736430141,
-0.00155924202532676));
#41512=CARTESIAN_POINT('Ctrl Pts',(-48.5062265507269,-3.21837549758788,
-0.0017103277108025));
#41513=CARTESIAN_POINT('Ctrl Pts',(-48.4799673743725,-3.22042966490226,
-0.428428751773469));
#41514=CARTESIAN_POINT('Ctrl Pts',(-48.3875504807753,-2.94292001229825,
-1.92766318074928));
#41515=CARTESIAN_POINT('Ctrl Pts',(-48.2289758699356,-0.671399218037883,
-3.74957431085067));
#41516=CARTESIAN_POINT('Ctrl Pts',(-48.0305027182074,2.78626390843014,-2.59746373509423));
#41517=CARTESIAN_POINT('Ctrl Pts',(-47.8320295664793,3.69333078266646,0.932412007837439));
#41518=CARTESIAN_POINT('Ctrl Pts',(-47.6335564147512,1.21945602247574,3.6087409759921));
#41519=CARTESIAN_POINT('Ctrl Pts',(-47.441622076167,-2.25244999498725,3.00222607590046));
#41520=CARTESIAN_POINT('Ctrl Pts',(-47.3158454548256,-3.22028487235349,
0.960583864842949));
#41521=CARTESIAN_POINT('Ctrl Pts',(-47.2562265507269,-3.22676077824252,
-0.00180977931619085));
#41522=CARTESIAN_POINT('Origin',(-56.8777734492732,0.,0.));
#41523=CARTESIAN_POINT('',(-50.0027734492731,-3.2280388681347,-6.59018652397875E-5));
#41524=CARTESIAN_POINT('',(-49.7562265507269,-3.2205221309114,0.00272251988370595));
#41525=CARTESIAN_POINT('',(-56.8777734492732,-3.22275,1.66140794472856E-12));
#41526=CARTESIAN_POINT('Ctrl Pts',(-50.0027734492731,-3.2280388681347,-6.59018652398626E-5));
#41527=CARTESIAN_POINT('Ctrl Pts',(-50.0025548029331,-3.22803992941049,
-0.00359167159406266));
#41528=CARTESIAN_POINT('Ctrl Pts',(-49.9361784393503,-3.22643794640511,
-1.07393913886435));
#41529=CARTESIAN_POINT('Ctrl Pts',(-49.8036443585249,-2.05513705304844,
-3.20725692790933));
#41530=CARTESIAN_POINT('Ctrl Pts',(-49.6051712067968,1.58022531640166,-3.46597364026232));
#41531=CARTESIAN_POINT('Ctrl Pts',(-49.4066980550686,3.7690209209745,-0.551875545371135));
#41532=CARTESIAN_POINT('Ctrl Pts',(-49.2082249033405,2.50758677259566,2.8674193792543));
#41533=CARTESIAN_POINT('Ctrl Pts',(-49.0097517516124,-1.04933754975442,
3.66182687025214));
#41534=CARTESIAN_POINT('Ctrl Pts',(-48.8579346002566,-3.03534529000393,
1.70538112699385));
#41535=CARTESIAN_POINT('Ctrl Pts',(-48.7722751661435,-3.22343319680733,
0.319091315453159));
#41536=CARTESIAN_POINT('Ctrl Pts',(-48.7527734492731,-3.22081842851865,
0.00278806351307209));
#41537=CARTESIAN_POINT('Ctrl Pts',(-49.7562265507269,-3.2205221309114,0.00272251988370574));
#41538=CARTESIAN_POINT('Ctrl Pts',(-49.7102470111621,-3.21454231443744,
-0.743204705410713));
#41539=CARTESIAN_POINT('Ctrl Pts',(-49.5981097543545,-2.5853985811797,-2.57151118715912));
#41540=CARTESIAN_POINT('Ctrl Pts',(-49.4198147803043,0.456741400770442,
-3.78172866771592));
#41541=CARTESIAN_POINT('Ctrl Pts',(-49.2213416285762,3.42506018203235,-1.66704744142366));
#41542=CARTESIAN_POINT('Ctrl Pts',(-49.022868476848,3.25801707681289,1.97367908980867));
#41543=CARTESIAN_POINT('Ctrl Pts',(-48.82439532512,0.108526357580573,3.80766417274334));
#41544=CARTESIAN_POINT('Ctrl Pts',(-48.6521813497462,-2.71047082998708,
2.37456382570328));
#41545=CARTESIAN_POINT('Ctrl Pts',(-48.5461250916152,-3.21525436852128,
0.646651306350763));
#41546=CARTESIAN_POINT('Ctrl Pts',(-48.5062265507269,-3.21837549758788,
-0.0017103277108025));
#41547=CARTESIAN_POINT('Origin',(-56.8777734492732,0.,0.));
#41548=CARTESIAN_POINT('',(-51.2527734492731,-3.22062593581149,-0.00274689833755447));
#41549=CARTESIAN_POINT('',(-51.0062265507269,-3.22803304482756,0.000137933179436404));
#41550=CARTESIAN_POINT('',(-56.8777734492732,-3.22275,1.66140794472856E-12));
#41551=CARTESIAN_POINT('Ctrl Pts',(-51.2527734492731,-3.22062593581149,
-0.00274689833755396));
#41552=CARTESIAN_POINT('Ctrl Pts',(-51.2328344397227,-3.22324839602356,
-0.326191645141541));
#41553=CARTESIAN_POINT('Ctrl Pts',(-51.1467377129296,-3.0297912547185,-1.71976224857695));
#41554=CARTESIAN_POINT('Ctrl Pts',(-50.9944832688937,-1.02516800960105,
-3.66866668622662));
#41555=CARTESIAN_POINT('Ctrl Pts',(-50.7960101171655,2.52644049755188,-2.85082162384731));
#41556=CARTESIAN_POINT('Ctrl Pts',(-50.5975369654374,3.76529981837076,0.576717135381059));
#41557=CARTESIAN_POINT('Ctrl Pts',(-50.3990638137093,1.55733573647028,3.47631854666922));
#41558=CARTESIAN_POINT('Ctrl Pts',(-50.2008093083212,-2.07223866782462,
3.1939466957081));
#41559=CARTESIAN_POINT('Ctrl Pts',(-50.0687125201758,-3.22771881000176,
1.06323101909589));
#41560=CARTESIAN_POINT('Ctrl Pts',(-50.0027734492731,-3.2280388681347,-6.59018652398626E-5));
#41561=CARTESIAN_POINT('Ctrl Pts',(-51.0062265507269,-3.22803304482756,
0.000137933179436442));
#41562=CARTESIAN_POINT('Ctrl Pts',(-50.9405266479517,-3.2273719077905,-1.05930734273043));
#41563=CARTESIAN_POINT('Ctrl Pts',(-50.8086690279337,-2.07936694243932,
-3.18680858367589));
#41564=CARTESIAN_POINT('Ctrl Pts',(-50.6106536906731,1.54478799997451,-3.48191247610533));
#41565=CARTESIAN_POINT('Ctrl Pts',(-50.412180538945,3.76319524430468,-0.590293130886969));
#41566=CARTESIAN_POINT('Ctrl Pts',(-50.2137073872169,2.53670566171588,2.84169118600161));
#41567=CARTESIAN_POINT('Ctrl Pts',(-50.0152342354887,-1.01193004948523,
3.67234012625855));
#41568=CARTESIAN_POINT('Ctrl Pts',(-49.8627406233254,-3.02672898098561,
1.72762799301611));
#41569=CARTESIAN_POINT('Ctrl Pts',(-49.7764047284048,-3.22314638075024,
0.330073603196574));
#41570=CARTESIAN_POINT('Ctrl Pts',(-49.7562265507269,-3.2205221309114,0.00272251988370574));
#41571=CARTESIAN_POINT('Origin',(-56.8777734492732,0.,0.));
#41572=CARTESIAN_POINT('',(-52.5027734492731,-3.21831359885928,0.00166126316387731));
#41573=CARTESIAN_POINT('',(-52.2562265507269,-3.22092507366678,-0.00280858089474589));
#41574=CARTESIAN_POINT('',(-56.8777734492732,-3.22275,1.66140794472856E-12));
#41575=CARTESIAN_POINT('Ctrl Pts',(-52.5027734492731,-3.21831359885928,
0.00166126316387728));
#41576=CARTESIAN_POINT('Ctrl Pts',(-52.4631140765123,-3.21531050958603,
-0.642846125141404));
#41577=CARTESIAN_POINT('Ctrl Pts',(-52.3572969865087,-2.71511064840447,
-2.36678331187106));
#41578=CARTESIAN_POINT('Ctrl Pts',(-52.1853221792625,0.0947938145258543,
-3.80802701948498));
#41579=CARTESIAN_POINT('Ctrl Pts',(-51.9868490275343,3.25087740482292,-1.98541860413584));
#41580=CARTESIAN_POINT('Ctrl Pts',(-51.7883758758062,3.43105052559699,1.65468502690142));
#41581=CARTESIAN_POINT('Ctrl Pts',(-51.5899027240781,0.47037738033959,3.78005636351393));
#41582=CARTESIAN_POINT('Ctrl Pts',(-51.4113685819003,-2.58019410180226,
2.57921047192559));
#41583=CARTESIAN_POINT('Ctrl Pts',(-51.2989921569654,-3.2145470620505,0.746999380148212));
#41584=CARTESIAN_POINT('Ctrl Pts',(-51.2527734492731,-3.22062593581149,
-0.00274689833755396));
#41585=CARTESIAN_POINT('Ctrl Pts',(-52.2562265507269,-3.22092507366678,
-0.00280858089474579));
#41586=CARTESIAN_POINT('Ctrl Pts',(-52.236964001984,-3.22353331455023,-0.31520661263699));
#41587=CARTESIAN_POINT('Ctrl Pts',(-52.1515437359983,-3.03835869510582,
-1.69751686651351));
#41588=CARTESIAN_POINT('Ctrl Pts',(-51.99996575277,-1.06253710715876,-3.65801790350669));
#41589=CARTESIAN_POINT('Ctrl Pts',(-51.8014926010418,2.49722875856415,-2.87644469098565));
#41590=CARTESIAN_POINT('Ctrl Pts',(-51.6030194493138,3.77098671823784,0.538278876876041));
#41591=CARTESIAN_POINT('Ctrl Pts',(-51.4045462975856,1.59271521326821,3.46025173262707));
#41592=CARTESIAN_POINT('Ctrl Pts',(-51.2060731458574,-2.04355643697909,
3.21464799167866));
#41593=CARTESIAN_POINT('Ctrl Pts',(-51.0732998969046,-3.22467120902133,
1.08172637814565));
#41594=CARTESIAN_POINT('Ctrl Pts',(-51.0066843651944,-3.22803765180699,
0.0075204307834513));
#41595=CARTESIAN_POINT('Ctrl Pts',(-51.0062265507269,-3.22803304482756,
0.000137933179436442));
#41596=CARTESIAN_POINT('Origin',(-56.8777734492732,0.,0.));
#41597=CARTESIAN_POINT('',(-53.7527734492731,-3.22663436289375,0.00208142861643813));
#41598=CARTESIAN_POINT('',(-53.5062265507269,-3.21814301605221,0.00152842760642868));
#41599=CARTESIAN_POINT('',(-56.8777734492732,-3.22275,1.66140794472856E-12));
#41600=CARTESIAN_POINT('Ctrl Pts',(-53.7527734492731,-3.22663436289375,
0.00208142861643813));
#41601=CARTESIAN_POINT('Ctrl Pts',(-53.6933937133019,-3.22001905440489,
-0.956459817829004));
#41602=CARTESIAN_POINT('Ctrl Pts',(-53.5678562600879,-2.25900515456935,
-2.99520192780961));
#41603=CARTESIAN_POINT('Ctrl Pts',(-53.3761610896312,1.20646915281294,-3.61292403145259));
#41604=CARTESIAN_POINT('Ctrl Pts',(-53.1776879379031,3.68992516100066,-0.945826390348501));
#41605=CARTESIAN_POINT('Ctrl Pts',(-52.979214786175,2.79562367813024,2.58745046926129));
#41606=CARTESIAN_POINT('Ctrl Pts',(-52.7807416344468,-0.657876967632621,
3.75194409668105));
#41607=CARTESIAN_POINT('Ctrl Pts',(-52.6219278554796,-2.93938347591651,
1.93553501403558));
#41608=CARTESIAN_POINT('Ctrl Pts',(-52.529271793755,-3.22032010800284,0.432287811380001));
#41609=CARTESIAN_POINT('Ctrl Pts',(-52.5027734492731,-3.21831359885928,
0.00166126316387728));
#41610=CARTESIAN_POINT('Ctrl Pts',(-53.5062265507269,-3.21814301605221,
0.00152842760642868));
#41611=CARTESIAN_POINT('Ctrl Pts',(-53.4672436387736,-3.21547541045439,
-0.632074783174344));
#41612=CARTESIAN_POINT('Ctrl Pts',(-53.3621030095775,-2.72813073009025,
-2.34477970215022));
#41613=CARTESIAN_POINT('Ctrl Pts',(-53.1908046631388,0.055953337280497,
-3.80877338647033));
#41614=CARTESIAN_POINT('Ctrl Pts',(-52.9923315114106,3.23045115613742,-2.01848786902524));
#41615=CARTESIAN_POINT('Ctrl Pts',(-52.7938583596826,3.44775307743432,1.61960618367426));
#41616=CARTESIAN_POINT('Ctrl Pts',(-52.5953852079543,0.508910540986547,
3.77505824730967));
#41617=CARTESIAN_POINT('Ctrl Pts',(-52.4161746049693,-2.56535413208167,
2.60096512785637));
#41618=CARTESIAN_POINT('Ctrl Pts',(-52.3031217192267,-3.21457524440225,
0.757732432294889));
#41619=CARTESIAN_POINT('Ctrl Pts',(-52.2562265507269,-3.22092507366678,
-0.00280858089474579));
#41620=CARTESIAN_POINT('Ctrl Pts',(-54.9770630286919,-1.43290239521256,
2.88667772504901));
#41621=CARTESIAN_POINT('Ctrl Pts',(-54.9109053114492,-2.3928525167459,2.41017325886154));
#41622=CARTESIAN_POINT('Ctrl Pts',(-54.7785898769638,-3.7834146058807,0.432460660303072));
#41623=CARTESIAN_POINT('Ctrl Pts',(-54.5801167252357,-2.41256151508884,
-2.9510558129106));
#41624=CARTESIAN_POINT('Ctrl Pts',(-54.3816435735076,1.16997685241348,-3.6239435622357));
#41625=CARTESIAN_POINT('Ctrl Pts',(-54.1831704217794,3.67986340215961,-0.983988949453548));
#41626=CARTESIAN_POINT('Ctrl Pts',(-53.9846972700513,2.8219875869866,2.55909768807962));
#41627=CARTESIAN_POINT('Ctrl Pts',(-53.7862241183231,-0.619631178725218,
3.75830321175399));
#41628=CARTESIAN_POINT('Ctrl Pts',(-53.587750966595,-3.49379594847047,1.51773663572276));
#41629=CARTESIAN_POINT('Ctrl Pts',(-53.3892778148669,-3.16979840530699,
-2.1125314397275));
#41630=CARTESIAN_POINT('Ctrl Pts',(-53.1908046631388,0.055953337280497,
-3.80877338647033));
#41631=CARTESIAN_POINT('Ctrl Pts',(-52.9923315114106,3.23045115613742,-2.01848786902524));
#41632=CARTESIAN_POINT('Ctrl Pts',(-52.7938583596826,3.44775307743432,1.61960618367426));
#41633=CARTESIAN_POINT('Ctrl Pts',(-52.5953852079543,0.508910540986547,
3.77505824730967));
#41634=CARTESIAN_POINT('Ctrl Pts',(-52.3969120562264,-2.89579313584141,
2.47476709288819));
#41635=CARTESIAN_POINT('Ctrl Pts',(-52.1984389044981,-3.64963801363799,
-1.09097741721031));
#41636=CARTESIAN_POINT('Ctrl Pts',(-51.99996575277,-1.06253710715876,-3.65801790350669));
#41637=CARTESIAN_POINT('Ctrl Pts',(-51.8014926010418,2.49722875856415,-2.87644469098565));
#41638=CARTESIAN_POINT('Ctrl Pts',(-51.6030194493138,3.77098671823784,0.538278876876041));
#41639=CARTESIAN_POINT('Ctrl Pts',(-51.4045462975856,1.59271521326821,3.46025173262707));
#41640=CARTESIAN_POINT('Ctrl Pts',(-51.2060731458574,-2.04355643697909,
3.21464799167866));
#41641=CARTESIAN_POINT('Ctrl Pts',(-51.0075999941294,-3.80911970524725,
0.0262973384752155));
#41642=CARTESIAN_POINT('Ctrl Pts',(-50.8091268424012,-2.08774604371503,
-3.18612629899413));
#41643=CARTESIAN_POINT('Ctrl Pts',(-50.6106536906731,1.54478799997451,-3.48191247610533));
#41644=CARTESIAN_POINT('Ctrl Pts',(-50.412180538945,3.76319524430468,-0.590293130886969));
#41645=CARTESIAN_POINT('Ctrl Pts',(-50.2137073872169,2.53670566171588,2.84169118600161));
#41646=CARTESIAN_POINT('Ctrl Pts',(-50.0152342354887,-1.01193004948523,
3.67234012625855));
#41647=CARTESIAN_POINT('Ctrl Pts',(-49.8167610837606,-3.63422673693658,
1.14126265479567));
#41648=CARTESIAN_POINT('Ctrl Pts',(-49.6182879320324,-2.92968669924813,
-2.43454724029718));
#41649=CARTESIAN_POINT('Ctrl Pts',(-49.4198147803043,0.456741400770442,
-3.78172866771592));
#41650=CARTESIAN_POINT('Ctrl Pts',(-49.2213416285762,3.42506018203235,-1.66704744142366));
#41651=CARTESIAN_POINT('Ctrl Pts',(-49.022868476848,3.25801707681289,1.97367908980867));
#41652=CARTESIAN_POINT('Ctrl Pts',(-48.82439532512,0.108526357580573,3.80766417274334));
#41653=CARTESIAN_POINT('Ctrl Pts',(-48.6259221733918,-3.14031134746123,
2.15604477308386));
#41654=CARTESIAN_POINT('Ctrl Pts',(-48.4274490216636,-3.5144513867625,-1.46925691171152));
#41655=CARTESIAN_POINT('Ctrl Pts',(-48.2289758699356,-0.671399218037883,
-3.74957431085067));
#41656=CARTESIAN_POINT('Ctrl Pts',(-48.0305027182074,2.78626390843014,-2.59746373509423));
#41657=CARTESIAN_POINT('Ctrl Pts',(-47.8320295664793,3.69333078266646,0.932412007837439));
#41658=CARTESIAN_POINT('Ctrl Pts',(-47.6335564147512,1.21945602247574,3.6087409759921));
#41659=CARTESIAN_POINT('Ctrl Pts',(-47.435083263023,-2.37073078241276,2.98156334493733));
#41660=CARTESIAN_POINT('Ctrl Pts',(-47.2366101112949,-3.79070785577725,
-0.374991166165694));
#41661=CARTESIAN_POINT('Ctrl Pts',(-47.0381369595668,-1.74060256508747,
-3.38827199807887));
#41662=CARTESIAN_POINT('Ctrl Pts',(-46.8396638078386,1.90288171805956,-3.29986751092048));
#41663=CARTESIAN_POINT('Ctrl Pts',(-46.6411906561105,3.80443374423865,-0.190704767250943));
#41664=CARTESIAN_POINT('Ctrl Pts',(-46.4427175043824,2.22333848041998,3.09303256110211));
#41665=CARTESIAN_POINT('Ctrl Pts',(-46.2442443526542,-1.39304094239042,
3.54535207777422));
#41666=CARTESIAN_POINT('Ctrl Pts',(-46.0457712009261,-3.7342055529521,0.752192336344735));
#41667=CARTESIAN_POINT('Ctrl Pts',(-45.847298049198,-2.65701102689385,-2.72953784101238));
#41668=CARTESIAN_POINT('Ctrl Pts',(-45.6488248974699,0.852459331624162,
-3.71259983171912));
#41669=CARTESIAN_POINT('Ctrl Pts',(-45.4503517457417,3.5815730376942,-1.29708095283833));
#41670=CARTESIAN_POINT('Ctrl Pts',(-45.2518785940136,3.03205016544447,2.30580923252167));
#41671=CARTESIAN_POINT('Ctrl Pts',(-45.0534054422855,-0.29306613324189,
3.79792004445863));
#41672=CARTESIAN_POINT('Ctrl Pts',(-44.8549322905573,-3.34990440598796,
1.8133463246982));
#41673=CARTESIAN_POINT('Ctrl Pts',(-44.6564591388292,-3.34017974570013,
-1.83119733752774));
#41674=CARTESIAN_POINT('Ctrl Pts',(-44.4579859871011,-0.272794281860559,
-3.79942991807168));
#41675=CARTESIAN_POINT('Ctrl Pts',(-44.2595128353729,3.04431198941514,-2.28959580137133));
#41676=CARTESIAN_POINT('Ctrl Pts',(-44.0610396836448,3.57460013936063,1.31617562135035));
#41677=CARTESIAN_POINT('Ctrl Pts',(-43.8625665319167,0.832634827927634,
3.71709613352627));
#41678=CARTESIAN_POINT('Ctrl Pts',(-43.6640933801885,-2.671539427591,2.71531978031699));
#41679=CARTESIAN_POINT('Ctrl Pts',(-43.4656202284604,-3.73013829052675,
-0.772109290256342));
#41680=CARTESIAN_POINT('Ctrl Pts',(-43.2671470767323,-1.3741012622493,-3.55273558594484));
#41681=CARTESIAN_POINT('Ctrl Pts',(-43.0686739250041,2.23981285336136,-3.0811236269373));
#41682=CARTESIAN_POINT('Ctrl Pts',(-42.8702007732761,3.80336187175512,0.211004490552806));
#41683=CARTESIAN_POINT('Ctrl Pts',(-42.6717276215479,1.88524481156147,3.30997529039638));
#41684=CARTESIAN_POINT('Ctrl Pts',(-42.4732544698198,-1.75865936318237,
3.37893499002941));
#41685=CARTESIAN_POINT('Ctrl Pts',(-42.2747813180916,-3.79265502670778,
0.354756636220095));
#41686=CARTESIAN_POINT('Ctrl Pts',(-42.0763081663635,-2.35478585077766,
-2.99417234299084));
#41687=CARTESIAN_POINT('Ctrl Pts',(-41.8778350146354,1.2386967785751,-3.60218193784014));
#41688=CARTESIAN_POINT('Ctrl Pts',(-41.6793618629072,3.69825402795075,-0.912689195345268));
#41689=CARTESIAN_POINT('Ctrl Pts',(-41.4808887111792,2.77236281533892,2.61229570352975));
#41690=CARTESIAN_POINT('Ctrl Pts',(-41.2824155594509,-0.691399338080392,
3.7459379837173));
#41691=CARTESIAN_POINT('Ctrl Pts',(-41.0839424077229,-3.52224206302542,
1.45048104848306));
#41692=CARTESIAN_POINT('Ctrl Pts',(-40.8854692559947,-3.12876085432636,
-2.17277240846552));
#41693=CARTESIAN_POINT('Ctrl Pts',(-40.6869961042666,0.128844490289695,
-3.80703080101488));
#41694=CARTESIAN_POINT('Ctrl Pts',(-40.4885229525384,3.26850326385081,-1.95626451093675));
#41695=CARTESIAN_POINT('Ctrl Pts',(-40.2900498008104,3.41611517854965,1.68530160785441));
#41696=CARTESIAN_POINT('Ctrl Pts',(-40.0915766490822,0.436553624420728,
3.78411222819291));
#41697=CARTESIAN_POINT('Ctrl Pts',(-39.8931034973541,-2.94263699390992,
2.41887824096765));
#41698=CARTESIAN_POINT('Ctrl Pts',(-39.694630345626,-3.62808461624092,-1.1606405300307));
#41699=CARTESIAN_POINT('Ctrl Pts',(-39.4961571938978,-0.992318122077262,
-3.67768801927938));
#41700=CARTESIAN_POINT('Ctrl Pts',(-39.2976840421697,2.55183428468159,-2.82811354193527));
#41701=CARTESIAN_POINT('Ctrl Pts',(-39.0992108904416,3.7599915464262,0.610367097210888));
#41702=CARTESIAN_POINT('Ctrl Pts',(-38.9007377387134,1.52618470788745,3.4901066831781));
#41703=CARTESIAN_POINT('Ctrl Pts',(-38.7022645869853,-2.10471914804825,
3.17493964200786));
#41704=CARTESIAN_POINT('Ctrl Pts',(-38.5037914352571,-3.80892512200428,
-0.0466244304919306));
#41705=CARTESIAN_POINT('Ctrl Pts',(-38.3053182835291,-2.02637231772134,
-3.22550765811006));
#41706=CARTESIAN_POINT('Ctrl Pts',(-38.1068451318009,1.6111582665074,-3.45170298009821));
#41707=CARTESIAN_POINT('Ctrl Pts',(-37.9083719800728,3.77380550466478,-0.518147117637242));
#41708=CARTESIAN_POINT('Ctrl Pts',(-37.7098988283447,2.48184309593248,2.88972996484555));
#41709=CARTESIAN_POINT('Ctrl Pts',(-37.5114256766165,-1.082043260835,3.65229610029575));
#41710=CARTESIAN_POINT('Ctrl Pts',(-37.3129525248884,-3.65540769414567,
1.07148448991797));
#41711=CARTESIAN_POINT('Ctrl Pts',(-37.1144793731602,-2.88254597247797,
-2.49018335451532));
#41712=CARTESIAN_POINT('Ctrl Pts',(-36.9160062214322,0.529050339993744,
-3.77229242772965));
#41713=CARTESIAN_POINT('Ctrl Pts',(-36.717533069704,3.45634442597985,-1.60117695198001));
#41714=CARTESIAN_POINT('Ctrl Pts',(-36.5190599179759,3.21963846421469,2.03568479443731));
#41715=CARTESIAN_POINT('Ctrl Pts',(-36.3205867662477,0.0356173628047984,
3.80904395170505));
#41716=CARTESIAN_POINT('Ctrl Pts',(-36.1221136145196,-3.18100851513376,
2.09553555188179));
#41717=CARTESIAN_POINT('Ctrl Pts',(-35.9236404627915,-3.48568180578722,
-1.53626390029769));
#41718=CARTESIAN_POINT('Ctrl Pts',(-35.7251673110634,-0.599499081901595,
-3.76173966049661));
#41719=CARTESIAN_POINT('Ctrl Pts',(-35.5266941593352,2.83547591786548,-2.54365106525228));
#41720=CARTESIAN_POINT('Ctrl Pts',(-35.3282210076071,3.67480510407022,1.0029416082971));
#41721=CARTESIAN_POINT('Ctrl Pts',(-35.1297478558789,1.15015139627886,3.6314234382941));
#41722=CARTESIAN_POINT('Ctrl Pts',(-34.9312747041509,-2.42737165097821,
2.9356347338491));
#41723=CARTESIAN_POINT('Ctrl Pts',(-34.7328015524227,-3.78283489369835,
-0.447486971399394));
#41724=CARTESIAN_POINT('Ctrl Pts',(-34.5343284006946,-1.67542282389703,
-3.42097102935977));
#41725=CARTESIAN_POINT('Ctrl Pts',(-34.3358552489665,1.96570152728694,-3.26283648505036));
#41726=CARTESIAN_POINT('Ctrl Pts',(-34.1373820972383,3.80738723472595,-0.117842553434008));
#41727=CARTESIAN_POINT('Ctrl Pts',(-33.9389089455102,2.16372197368752,3.13502657773993));
#41728=CARTESIAN_POINT('Ctrl Pts',(-33.740435793782,-1.46065342046419,3.51803581673643));
#41729=CARTESIAN_POINT('Ctrl Pts',(-33.541962642054,-3.74792032005764,0.680571595831895));
#41730=CARTESIAN_POINT('Ctrl Pts',(-33.3434894903258,-2.60427333777752,
-2.77990014293592));
#41731=CARTESIAN_POINT('Ctrl Pts',(-33.1450163385977,0.923372444839,-3.6956011352236));
#41732=CARTESIAN_POINT('Ctrl Pts',(-32.9465431868696,3.60574643173899,-1.22828217139039));
#41733=CARTESIAN_POINT('Ctrl Pts',(-32.7480700351414,2.98735507926837,2.36342845310018));
#41734=CARTESIAN_POINT('Ctrl Pts',(-32.5495968834133,-0.365715011353638,
3.79161403007012));
#41735=CARTESIAN_POINT('Ctrl Pts',(-32.3511237316851,-3.38400298226306,
1.74888771468858));
#41736=CARTESIAN_POINT('Ctrl Pts',(-32.152650579957,-3.30451356820155,-1.89480196857768));
#41737=CARTESIAN_POINT('Ctrl Pts',(-31.9541774282289,-0.200012812968363,
-3.80395574332859));
#41738=CARTESIAN_POINT('Ctrl Pts',(-31.7557042765008,3.08758327993605,-2.23089979873894));
#41739=CARTESIAN_POINT('Ctrl Pts',(-31.5572311247726,3.54874993145618,1.38436207205476));
#41740=CARTESIAN_POINT('Ctrl Pts',(-31.3587579730445,0.761326868309329,
3.73235392509128));
#41741=CARTESIAN_POINT('Ctrl Pts',(-31.1602848213164,-2.72302854613296,
2.66368165505921));
#41742=CARTESIAN_POINT('Ctrl Pts',(-30.9618116695882,-3.71467449989982,
-0.843372860808289));
#41743=CARTESIAN_POINT('Ctrl Pts',(-30.7633385178601,-1.30584039539486,
-3.57838864355298));
#41744=CARTESIAN_POINT('Ctrl Pts',(-30.5648653661319,2.29838356734553,-3.03768289982842));
#41745=CARTESIAN_POINT('Ctrl Pts',(-30.3663922144039,3.79862574454081,0.283772577015008));
#41746=CARTESIAN_POINT('Ctrl Pts',(-30.1679190626757,1.82153737945105,3.34545751696486));
#41747=CARTESIAN_POINT('Ctrl Pts',(-29.9694459109477,-1.82301916741003,
3.34465028632439));
#41748=CARTESIAN_POINT('Ctrl Pts',(-29.7709727592194,-3.79875107706736,
0.282089838586104));
#41749=CARTESIAN_POINT('Ctrl Pts',(-29.5724996074914,-2.29703771278357,
-3.03870073692754));
#41750=CARTESIAN_POINT('Ctrl Pts',(-29.3740264557631,1.30742541749708,-3.57780983287773));
#41751=CARTESIAN_POINT('Ctrl Pts',(-29.1755533040351,3.71504773171258,-0.841727256093824));
#41752=CARTESIAN_POINT('Ctrl Pts',(-28.9770801523069,2.72184832452091,2.66488763756686));
#41753=CARTESIAN_POINT('Ctrl Pts',(-28.7786070005788,-0.762980147188692,
3.732016307246));
#41754=CARTESIAN_POINT('Ctrl Pts',(-28.5801338488507,-3.54936282628784,
1.38278991532342));
#41755=CARTESIAN_POINT('Ctrl Pts',(-28.3816606971225,-3.08659473573302,
-2.2322673137192));
#41756=CARTESIAN_POINT('Ctrl Pts',(-28.1831875453944,0.201697865006982,
-3.80386676867179));
#41757=CARTESIAN_POINT('Ctrl Pts',(-27.9847143936663,3.30535260103752,-1.89333795329003));
#41758=CARTESIAN_POINT('Ctrl Pts',(-27.7862412419381,3.38322793010033,1.75038658459866));
#41759=CARTESIAN_POINT('Ctrl Pts',(-27.5877680902101,0.364035370925649,
3.79177566204397));
#41760=CARTESIAN_POINT('Ctrl Pts',(-27.3892949384819,-2.98840173480935,
2.36210488631272));
#41761=CARTESIAN_POINT('Ctrl Pts',(-27.1908217867538,-3.60520197502674,
-1.22987932002179));
#41762=CARTESIAN_POINT('Ctrl Pts',(-26.9923486350256,-0.921735281371103,
-3.69600980702566));
#41763=CARTESIAN_POINT('Ctrl Pts',(-26.7938754832976,2.60550451902449,-2.77874623236759));
#41764=CARTESIAN_POINT('Ctrl Pts',(-26.5954023315693,3.74761847355685,0.682231778217214));
#41765=CARTESIAN_POINT('Ctrl Pts',(-26.3969291798413,1.45909486194852,3.51868251002977));
#41766=CARTESIAN_POINT('Ctrl Pts',(-26.1984560281131,-2.16511051163293,
3.13406778723285));
#41767=CARTESIAN_POINT('Ctrl Pts',(-25.999982876385,-3.80733465941356,-0.119529133612606));
#41768=CARTESIAN_POINT('Ctrl Pts',(-25.8015097246568,-1.9642559671063,-3.26370692897528));
#41769=CARTESIAN_POINT('Ctrl Pts',(-25.6030365729288,1.67693807707542,-3.4202285169574));
#41770=CARTESIAN_POINT('Ctrl Pts',(-25.4045634212006,3.78303274977641,-0.445811211919431));
#41771=CARTESIAN_POINT('Ctrl Pts',(-25.2060902694725,2.42607098893233,2.93670971994425));
#41772=CARTESIAN_POINT('Ctrl Pts',(-25.0076171177444,-1.15175992694511,
3.63091358933775));
#41773=CARTESIAN_POINT('Ctrl Pts',(-24.8091439660162,-3.67524902536336,
1.00131364922265));
#41774=CARTESIAN_POINT('Ctrl Pts',(-24.6106708142881,-2.83434885622448,
-2.54490687133595));
#41775=CARTESIAN_POINT('Ctrl Pts',(-24.41219766256,0.601165393915808,-3.76147372604303));
#41776=CARTESIAN_POINT('Ctrl Pts',(-24.2137245108318,3.48636199609287,-1.53471966650373));
#41777=CARTESIAN_POINT('Ctrl Pts',(-24.0152513591037,3.18007992525289,2.09694446553971));
#41778=CARTESIAN_POINT('Ctrl Pts',(-23.8167782073755,-0.0373046849413855,
3.80902780024449));
#41779=CARTESIAN_POINT('Ctrl Pts',(-23.6183050556475,-3.22053991348009,
2.03425836319669));
#41780=CARTESIAN_POINT('Ctrl Pts',(-23.4198319039193,-3.45563479945234,
-1.60270788210705));
#41781=CARTESIAN_POINT('Ctrl Pts',(-23.2213587521912,-0.527379242599795,
-3.77252641568339));
#41782=CARTESIAN_POINT('Ctrl Pts',(-23.022885600463,2.88364878803355,-2.48890620350118));
#41783=CARTESIAN_POINT('Ctrl Pts',(-22.8244124487349,3.65493269060604,1.0731036528189));
#41784=CARTESIAN_POINT('Ctrl Pts',(-22.6259392970067,1.08042526501054,3.65277506415067));
#41785=CARTESIAN_POINT('Ctrl Pts',(-22.4274661452787,-2.48312294147182,
2.8886302775001));
#41786=CARTESIAN_POINT('Ctrl Pts',(-22.2289929935505,-3.77357560622099,
-0.519818782546203));
#41787=CARTESIAN_POINT('Ctrl Pts',(-22.0305198418224,-1.60962907726382,
-3.45241635035243));
#41788=CARTESIAN_POINT('Ctrl Pts',(-21.8320466900942,2.02780095034114,-3.22460970170803));
#41789=CARTESIAN_POINT('Ctrl Pts',(-21.6335735383662,3.80894540192439,-0.0449371529252134));
#41790=CARTESIAN_POINT('Ctrl Pts',(-21.435100386638,2.1033125106639,3.17587167641245));
#41791=CARTESIAN_POINT('Ctrl Pts',(-21.2366272349099,-1.52773060133581,
3.48943027331057));
#41792=CARTESIAN_POINT('Ctrl Pts',(-21.0381540831817,-3.76026155718447,
0.608701440867885));
#41793=CARTESIAN_POINT('Ctrl Pts',(-20.8396809314537,-2.5505812400301,-2.82924367288512));
#41794=CARTESIAN_POINT('Ctrl Pts',(-20.6412077797255,0.993947162456761,
-3.67724808257454));
#41795=CARTESIAN_POINT('Ctrl Pts',(-20.4427346279974,3.62859839939353,-1.15903325166825));
#41796=CARTESIAN_POINT('Ctrl Pts',(-20.2442614762692,2.94156519346794,2.42018152937583));
#41797=CARTESIAN_POINT('Ctrl Pts',(-20.0457883245411,-0.438229862995021,
3.78391847292371));
#41798=CARTESIAN_POINT('Ctrl Pts',(-19.847315172813,-3.41686139622225,1.68378817597706));
#41799=CARTESIAN_POINT('Ctrl Pts',(-19.6488420210848,-3.26763635950076,
-1.95771219657607));
#41800=CARTESIAN_POINT('Ctrl Pts',(-19.4503688693567,-0.12715804379987,
-3.80708750286241));
#41801=CARTESIAN_POINT('Ctrl Pts',(-19.2518957176286,3.12972303941186,-2.17138622062695));
#41802=CARTESIAN_POINT('Ctrl Pts',(-19.0534225659005,3.52159918511936,1.4520411846503));
#41803=CARTESIAN_POINT('Ctrl Pts',(-18.8549494141723,0.689739899217004,
3.74624389141739));
#41804=CARTESIAN_POINT('Ctrl Pts',(-18.6564762624442,-2.77351973488412,
2.61106734933481));
#41805=CARTESIAN_POINT('Ctrl Pts',(-18.4580031107161,-3.69784936315266,
-0.914327353842945));
#41806=CARTESIAN_POINT('Ctrl Pts',(-18.2595299589879,-1.23710096689095,
-3.6027303007957));
#41807=CARTESIAN_POINT('Ctrl Pts',(-18.0610568072598,2.35611197454017,-2.99312892906109));
#41808=CARTESIAN_POINT('Ctrl Pts',(-17.8625836555317,3.79249750493022,0.356436667098387));
#41809=CARTESIAN_POINT('Ctrl Pts',(-17.6641105038036,1.75716239414189,3.37971370727872));
#41810=CARTESIAN_POINT('Ctrl Pts',(-17.4656373520754,-1.88671087539651,
3.30913984219684));
#41811=CARTESIAN_POINT('Ctrl Pts',(-17.2671642003473,-3.80345496909903,
0.209319661259676));
#41812=CARTESIAN_POINT('Ctrl Pts',(-17.0686910486191,-2.23844776122589,
-3.08211551419099));
#41813=CARTESIAN_POINT('Ctrl Pts',(-16.870217896891,1.37567491389401,-3.55212653967123));
#41814=CARTESIAN_POINT('Ctrl Pts',(-16.6717447451629,3.73047995257294,-0.770456842402849));
#41815=CARTESIAN_POINT('Ctrl Pts',(-16.4732715934348,2.67033633643725,2.7165029491714));
#41816=CARTESIAN_POINT('Ctrl Pts',(-16.2747984417066,-0.834281340932724,
3.71672692926525));
#41817=CARTESIAN_POINT('Ctrl Pts',(-16.0763252899785,-3.57518282650542,
1.31459202021571));
#41818=CARTESIAN_POINT('Ctrl Pts',(-15.8778521382504,-3.04329744837427,
-2.29094414232926));
#41819=CARTESIAN_POINT('Ctrl Pts',(-15.6793789865222,0.274477321913715,
-3.79930870321287));
#41820=CARTESIAN_POINT('Ctrl Pts',(-15.4809058347941,3.34099059953505,-1.82971752912093));
#41821=CARTESIAN_POINT('Ctrl Pts',(-15.282432683066,3.34910080337457,1.81483008333833));
#41822=CARTESIAN_POINT('Ctrl Pts',(-15.0839595313379,0.291383706511294,
3.79804949390259));
#41823=CARTESIAN_POINT('Ctrl Pts',(-14.8854863796097,-3.03307129250833,
2.30446587241291));
#41824=CARTESIAN_POINT('Ctrl Pts',(-14.6870132278816,-3.58099810695365,
-1.29866738641899));
#41825=CARTESIAN_POINT('Ctrl Pts',(-14.4885400761535,-0.850814645052164,
-3.71297708884916));
#41826=CARTESIAN_POINT('Ctrl Pts',(-14.2900669244253,2.6582198935355,-2.72836057370837));
#41827=CARTESIAN_POINT('Ctrl Pts',(-14.0915937726972,3.73387198132893,0.753846436352181));
#41828=CARTESIAN_POINT('Ctrl Pts',(-13.8931206209691,1.39147028998462,3.54596881749461));
#41829=CARTESIAN_POINT('Ctrl Pts',(-13.694647469241,-2.224708410058,3.09204736586798));
#41830=CARTESIAN_POINT('Ctrl Pts',(-13.4961743175128,-3.80434889280168,
-0.192390031947064));
#41831=CARTESIAN_POINT('Ctrl Pts',(-13.2977011657847,-1.9014197600839,-3.30071012336989));
#41832=CARTESIAN_POINT('Ctrl Pts',(-13.0992280140566,1.74210332689385,-3.38750061564265));
#41833=CARTESIAN_POINT('Ctrl Pts',(-12.9007548623284,3.79087359697976,-0.373311926243645));
#41834=CARTESIAN_POINT('Ctrl Pts',(-12.7022817106003,2.36940978052417,2.98261323582365));
#41835=CARTESIAN_POINT('Ctrl Pts',(-12.5038085588722,-1.22105449849256,
3.60820042878236));
#41836=CARTESIAN_POINT('Ctrl Pts',(-12.3053354071441,-3.69374345902606,
0.930775849201267));
#41837=CARTESIAN_POINT('Ctrl Pts',(-12.1068622554159,-2.78511301374644,
-2.5986977360236));
#41838=CARTESIAN_POINT('Ctrl Pts',(-11.9083891036878,0.673060134005079,
-3.74927652735391));
#41839=CARTESIAN_POINT('Ctrl Pts',(-11.7099159519597,3.51510189157322,-1.46769994018271));
#41840=CARTESIAN_POINT('Ctrl Pts',(-11.5114428002315,3.1393559572694,2.15743565283212));
#41841=CARTESIAN_POINT('Ctrl Pts',(-11.3129696485034,-0.110213061344868,
3.80761572426406));
#41842=CARTESIAN_POINT('Ctrl Pts',(-11.1144964967753,-3.2588910551131,1.97223566377292));
#41843=CARTESIAN_POINT('Ctrl Pts',(-10.9160233450471,-3.42432137932337,
-1.66856450689293));
#41844=CARTESIAN_POINT('Ctrl Pts',(-10.717550193319,-0.45506613045934,-3.78193062330111));
#41845=CARTESIAN_POINT('Ctrl Pts',(-10.5190770415909,2.93076486464135,-2.43324921262453));
#41846=CARTESIAN_POINT('Ctrl Pts',(-10.3206038898627,3.63372082507465,1.1428724285645));
#41847=CARTESIAN_POINT('Ctrl Pts',(-10.1221307381346,1.01030318175698,3.67278802866238));
#41848=CARTESIAN_POINT('Ctrl Pts',(-9.92365758640649,-2.53796422227748,
2.8405672019851));
#41849=CARTESIAN_POINT('Ctrl Pts',(-9.72518443467834,-3.76293338666949,
-0.591960091595758));
#41850=CARTESIAN_POINT('Ctrl Pts',(-9.52671128295022,-1.54324543714212,
-3.48259643704148));
#41851=CARTESIAN_POINT('Ctrl Pts',(-9.3282381312221,2.0891572291558,-3.18520117016493));
#41852=CARTESIAN_POINT('Ctrl Pts',(-9.12976497949396,3.80910767480012,0.0279847160571414));
#41853=CARTESIAN_POINT('Ctrl Pts',(-8.93129182776584,2.0421322300825,3.21555288829343));
#41854=CARTESIAN_POINT('Ctrl Pts',(-8.73281867603769,-1.59424790270054,
3.45954593079627));
#41855=CARTESIAN_POINT('Ctrl Pts',(-8.53434552430958,-3.77122474154193,
0.536608210276483));
#41856=CARTESIAN_POINT('Ctrl Pts',(-8.33587237258143,-2.49595441061896,
-2.87755034754663));
#41857=CARTESIAN_POINT('Ctrl Pts',(-8.13739922085333,1.06415762040292,-3.65754739976015));
#41858=CARTESIAN_POINT('Ctrl Pts',(-7.93892606912516,3.65012056591666,-1.08935957187082));
#41859=CARTESIAN_POINT('Ctrl Pts',(-7.74045291739707,2.89469728902442,2.47604766260028));
#41860=CARTESIAN_POINT('Ctrl Pts',(-7.54197976566891,-0.510584113075111,
3.77483619327098));
#41861=CARTESIAN_POINT('Ctrl Pts',(-7.3435066139408,-3.44846760598317,1.61807156610622));
#41862=CARTESIAN_POINT('Ctrl Pts',(-7.14503346221266,-3.22956163427927,
-2.01990496631462));
#41863=CARTESIAN_POINT('Ctrl Pts',(-6.94656031048453,-0.0542566740194617,
-3.80882404895191));
#41864=CARTESIAN_POINT('Ctrl Pts',(-6.74808715875641,3.17071582455421,-2.11107687744781));
#41865=CARTESIAN_POINT('Ctrl Pts',(-6.54961400702828,3.49315785049429,1.51918815623972));
#41866=CARTESIAN_POINT('Ctrl Pts',(-6.35114085530014,0.617900155701453,
3.75876094213507));
#41867=CARTESIAN_POINT('Ctrl Pts',(-6.15266770357201,-2.82299448995578,
2.55749614513145));
#41868=CARTESIAN_POINT('Ctrl Pts',(-5.95419455184388,-3.67966904629497,
-0.984946766120382));
#41869=CARTESIAN_POINT('Ctrl Pts',(-5.75572140011576,-1.16790816827868,
-3.62575163696693));
#41870=CARTESIAN_POINT('Ctrl Pts',(-5.55724824838763,2.41297691887338,-2.94747804273184));
#41871=CARTESIAN_POINT('Ctrl Pts',(-5.35877509665951,3.78497939857008,0.428970131116378));
#41872=CARTESIAN_POINT('Ctrl Pts',(-5.16030194493137,1.69214344806,3.41273130701552));
#41873=CARTESIAN_POINT('Ctrl Pts',(-4.96182879320323,-1.94971114633403,
3.27241667179486));
#41874=CARTESIAN_POINT('Ctrl Pts',(-4.76335564147511,-3.80676497740825,
0.136472772224148));
#41875=CARTESIAN_POINT('Ctrl Pts',(-4.56488248974698,-2.179037470938,-3.12440076292683));
#41876=CARTESIAN_POINT('Ctrl Pts',(-4.36640933801884,1.44342026140034,-3.52514147306206));
#41877=CARTESIAN_POINT('Ctrl Pts',(-4.16793618629072,3.74454502431787,-0.698904068557403));
#41878=CARTESIAN_POINT('Ctrl Pts',(-3.96946303456259,2.61784574945316,2.7671227133945));
#41879=CARTESIAN_POINT('Ctrl Pts',(-3.77098988283447,-0.905276827937616,
3.70007547035483));
#41880=CARTESIAN_POINT('Ctrl Pts',(-3.57251673110632,-3.59969252675421,
1.24591232298042));
#41881=CARTESIAN_POINT('Ctrl Pts',(-3.3740435793782,-2.9988850021576,-2.34878132703989));
#41882=CARTESIAN_POINT('Ctrl Pts',(-3.17557042765007,0.347156461294124,
-3.7933583964979));
#41883=CARTESIAN_POINT('Ctrl Pts',(-2.97709727592195,3.37540367795816,-1.76542632168304));
#41884=CARTESIAN_POINT('Ctrl Pts',(-2.77862412419381,3.31374730129506,1.87860804283756));
#41885=CARTESIAN_POINT('Ctrl Pts',(-2.58015097246569,0.218623351459381,
3.80293227389407));
#41886=CARTESIAN_POINT('Ctrl Pts',(-2.38167782073755,-3.07662565351087,
2.24598069837365));
#41887=CARTESIAN_POINT('Ctrl Pts',(-2.18320466900942,-3.55548884937955,
-1.36697641350964));
#41888=CARTESIAN_POINT('Ctrl Pts',(-1.98473151728128,-0.779568879692582,
-3.72858958741861));
#41889=CARTESIAN_POINT('Ctrl Pts',(-1.78625836555316,2.7099356073734,-2.67696366978096));
#41890=CARTESIAN_POINT('Ctrl Pts',(-1.58778521382502,3.71880583993438,0.825163098419798));
#41891=CARTESIAN_POINT('Ctrl Pts',(-1.3893120620969,1.32324257672849,3.57199715958687));
#41892=CARTESIAN_POINT('Ctrl Pts',(-1.19083891036877,-2.28331276119187,
3.04881430456285));
#41893=CARTESIAN_POINT('Ctrl Pts',(-0.992365758640647,-3.80030983792451,
-0.265028402279971));
#41894=CARTESIAN_POINT('Ctrl Pts',(-0.793892606912507,-1.8372343102454,
-3.33679471955611));
#41895=CARTESIAN_POINT('Ctrl Pts',(-0.59541945518438,1.80537864589007,-3.35297192389334));
#41896=CARTESIAN_POINT('Ctrl Pts',(-0.396946303456254,3.79975239553181,
-0.301770123854898));
#41897=CARTESIAN_POINT('Ctrl Pts',(-0.198473151728127,2.30693671058513,
3.02973452897375));
#41898=CARTESIAN_POINT('Ctrl Pts',(-0.0661577172427008,-0.082916802787829,
3.39526186154233));
#41899=CARTESIAN_POINT('Ctrl Pts',(8.88178419700125E-15,-1.09131022003164,
3.0323521507494));
#41900=CARTESIAN_POINT('Ctrl Pts',(-54.8403753524613,-1.53816642191861,
3.09873914818303));
#41901=CARTESIAN_POINT('Ctrl Pts',(-54.7742176352186,-2.56863650040579,
2.58722966070319));
#41902=CARTESIAN_POINT('Ctrl Pts',(-54.6419022007331,-4.06135220822103,
0.464230130887601));
#41903=CARTESIAN_POINT('Ctrl Pts',(-54.4434290490051,-2.58979336326103,
-3.16784658591715));
#41904=CARTESIAN_POINT('Ctrl Pts',(-54.2449558972769,1.25592581519661,-3.89016608596827));
#41905=CARTESIAN_POINT('Ctrl Pts',(-54.0464827455489,3.95019391506363,-1.0562748493163));
#41906=CARTESIAN_POINT('Ctrl Pts',(-53.8480095938205,3.02929673638347,2.7470943920291));
#41907=CARTESIAN_POINT('Ctrl Pts',(-53.6495364420926,-0.665150589651805,
4.03439607821359));
#41908=CARTESIAN_POINT('Ctrl Pts',(-53.4510632903643,-3.75045755449035,
1.62923276434178));
#41909=CARTESIAN_POINT('Ctrl Pts',(-53.2525901386363,-3.4026584696794,-2.26772244689711));
#41910=CARTESIAN_POINT('Ctrl Pts',(-53.0541169869081,0.0600637872383345,
-4.08857389822173));
#41911=CARTESIAN_POINT('Ctrl Pts',(-52.85564383518,3.46776689928094,-2.16677023749668));
#41912=CARTESIAN_POINT('Ctrl Pts',(-52.6571706834519,3.70103227721164,1.73858586375658));
#41913=CARTESIAN_POINT('Ctrl Pts',(-52.4586975317237,0.546296180759445,
4.05238197395636));
#41914=CARTESIAN_POINT('Ctrl Pts',(-52.2602243799957,-3.10852419624347,
2.65656869376971));
#41915=CARTESIAN_POINT('Ctrl Pts',(-52.0617512282674,-3.91774810586626,
-1.17112291516237));
#41916=CARTESIAN_POINT('Ctrl Pts',(-51.8632780765394,-1.14059332005749,
-3.92674360008736));
#41917=CARTESIAN_POINT('Ctrl Pts',(-51.6648049248112,2.680680440696,-3.08775437389328));
#41918=CARTESIAN_POINT('Ctrl Pts',(-51.4663317730831,4.0480113417869,0.577821976434141));
#41919=CARTESIAN_POINT('Ctrl Pts',(-51.2678586213549,1.70971942604948,3.71444910992895));
#41920=CARTESIAN_POINT('Ctrl Pts',(-51.0693854696268,-2.19368039523064,
3.45080280108978));
#41921=CARTESIAN_POINT('Ctrl Pts',(-50.8709123178987,-4.08894565830513,
0.0282291963244218));
#41922=CARTESIAN_POINT('Ctrl Pts',(-50.6724391661706,-2.24111626351152,
-3.42018584481279));
#41923=CARTESIAN_POINT('Ctrl Pts',(-50.4739660144424,1.65827137876417,-3.73770109722635));
#41924=CARTESIAN_POINT('Ctrl Pts',(-50.2754928627143,4.03964748977492,-0.633657307052364));
#41925=CARTESIAN_POINT('Ctrl Pts',(-50.0770197109862,2.72305740026553,3.05044780326519));
#41926=CARTESIAN_POINT('Ctrl Pts',(-49.878546559258,-1.08626856138223,3.9421179634757));
#41927=CARTESIAN_POINT('Ctrl Pts',(-49.6800734075299,-3.90120468433239,
1.22510221216824));
#41928=CARTESIAN_POINT('Ctrl Pts',(-49.4816002558018,-3.14490765217551,
-2.61339420613093));
#41929=CARTESIAN_POINT('Ctrl Pts',(-49.2831271040736,0.490294585669324,
-4.05954241748915));
#41930=CARTESIAN_POINT('Ctrl Pts',(-49.0846539523456,3.6766723139372,-1.7895122561802));
#41931=CARTESIAN_POINT('Ctrl Pts',(-48.8861808006173,3.49735787052484,2.11866971102118));
#41932=CARTESIAN_POINT('Ctrl Pts',(-48.6877076488894,0.116498932293703,
4.08738319931909));
#41933=CARTESIAN_POINT('Ctrl Pts',(-48.489234497161,-3.37100523048403,2.31443236133217));
#41934=CARTESIAN_POINT('Ctrl Pts',(-48.2907613454331,-3.77263038476602,
-1.57719161773841));
#41935=CARTESIAN_POINT('Ctrl Pts',(-48.0922881937048,-0.720721618121668,
-4.02502593387261));
#41936=CARTESIAN_POINT('Ctrl Pts',(-47.8938150419768,2.99094872118978,-2.78827888963095));
#41937=CARTESIAN_POINT('Ctrl Pts',(-47.6953418902486,3.9646506376959,1.0009089569821));
#41938=CARTESIAN_POINT('Ctrl Pts',(-47.4968687385205,1.30903982926209,3.87384668573263));
#41939=CARTESIAN_POINT('Ctrl Pts',(-47.2983955867924,-2.54488965689468,
3.20059526547526));
#41940=CARTESIAN_POINT('Ctrl Pts',(-47.0999224350642,-4.06918123560976,
-0.402538806718081));
#41941=CARTESIAN_POINT('Ctrl Pts',(-46.9014492833361,-1.86847089408725,
-3.63718159253868));
#41942=CARTESIAN_POINT('Ctrl Pts',(-46.7029761316081,2.04267141529049,-3.54228272563159));
#41943=CARTESIAN_POINT('Ctrl Pts',(-46.5045029798797,4.08391545673528,-0.204714340952344));
#41944=CARTESIAN_POINT('Ctrl Pts',(-46.3060298281518,2.38666960608566,3.32025324494081));
#41945=CARTESIAN_POINT('Ctrl Pts',(-46.1075566764235,-1.49537666285008,
3.80580110559607));
#41946=CARTESIAN_POINT('Ctrl Pts',(-45.9090835246955,-4.00852815466228,
0.80744996899671));
#41947=CARTESIAN_POINT('Ctrl Pts',(-45.7106103729673,-2.85220065085376,
-2.93005543743158));
#41948=CARTESIAN_POINT('Ctrl Pts',(-45.5121372212392,0.915082788846247,
-3.98533523165999));
#41949=CARTESIAN_POINT('Ctrl Pts',(-45.3136640695111,3.84468293348948,-1.39236725043635));
#41950=CARTESIAN_POINT('Ctrl Pts',(-45.115190917783,3.25479095410903,2.47519883326633));
#41951=CARTESIAN_POINT('Ctrl Pts',(-44.9167177660547,-0.314595388395248,
4.07692324685582));
#41952=CARTESIAN_POINT('Ctrl Pts',(-44.7182446143267,-3.59599543635577,
1.94655856342968));
#41953=CARTESIAN_POINT('Ctrl Pts',(-44.5197714625985,-3.58555638204929,
-1.96572094924447));
#41954=CARTESIAN_POINT('Ctrl Pts',(-44.3212983108704,-0.292834324131919,
-4.07854403896331));
#41955=CARTESIAN_POINT('Ctrl Pts',(-44.1228251591423,3.26795355748413,-2.4577943293286));
#41956=CARTESIAN_POINT('Ctrl Pts',(-43.9243520074141,3.83719779136388,1.4128646534984));
#41957=CARTESIAN_POINT('Ctrl Pts',(-43.7258788556861,0.893801935370474,
3.99016184126421));
#41958=CARTESIAN_POINT('Ctrl Pts',(-43.5274057039578,-2.86779633845362,
2.91479288806339));
#41959=CARTESIAN_POINT('Ctrl Pts',(-43.3289325522298,-4.00416210257613,
-0.828830064275004));
#41960=CARTESIAN_POINT('Ctrl Pts',(-43.1304594005017,-1.47504563393096,
-3.81372702182184));
#41961=CARTESIAN_POINT('Ctrl Pts',(-42.9319862487735,2.40435422114778,-3.30746945539968));
#41962=CARTESIAN_POINT('Ctrl Pts',(-42.7335130970454,4.08276484224243,0.226505324666171));
#41963=CARTESIAN_POINT('Ctrl Pts',(-42.5350399453173,2.02373886450903,3.55313304386828));
#41964=CARTESIAN_POINT('Ctrl Pts',(-42.3365667935891,-1.88785418258624,
3.62715866822016));
#41965=CARTESIAN_POINT('Ctrl Pts',(-42.138093641861,-4.07127144981634,0.380817805601726));
#41966=CARTESIAN_POINT('Ctrl Pts',(-41.9396204901328,-2.52777337701186,
-3.21413054707226));
#41967=CARTESIAN_POINT('Ctrl Pts',(-41.7411473384048,1.3296940518132,-3.86680580682888));
#41968=CARTESIAN_POINT('Ctrl Pts',(-41.5426741866766,3.96993555494399,-0.979737265160665));
#41969=CARTESIAN_POINT('Ctrl Pts',(-41.3442010349485,2.9760264245333,2.80420044569437));
#41970=CARTESIAN_POINT('Ctrl Pts',(-41.1457278832203,-0.742190989089927,
4.02112247449225));
#41971=CARTESIAN_POINT('Ctrl Pts',(-40.9472547314922,-3.78099338050939,
1.55703644006726));
#41972=CARTESIAN_POINT('Ctrl Pts',(-40.7487815797641,-3.35860621380553,
-2.33238884402664));
#41973=CARTESIAN_POINT('Ctrl Pts',(-40.550308428036,0.138309677808596,-4.08670329876998));
#41974=CARTESIAN_POINT('Ctrl Pts',(-40.3518352763078,3.50861439493976,-2.09997582052138));
#41975=CARTESIAN_POINT('Ctrl Pts',(-40.1533621245797,3.66707019166621,1.80910741210853));
#41976=CARTESIAN_POINT('Ctrl Pts',(-39.9548889728515,0.46862377276644,4.06210107933703));
#41977=CARTESIAN_POINT('Ctrl Pts',(-39.7564158211235,-3.15880930274817,
2.59657412912179));
#41978=CARTESIAN_POINT('Ctrl Pts',(-39.5579426693953,-3.89461135051907,
-1.24590362691542));
#41979=CARTESIAN_POINT('Ctrl Pts',(-39.3594695176672,-1.06521590049673,
-3.94785872397707));
#41980=CARTESIAN_POINT('Ctrl Pts',(-39.160996365939,2.73929740372549,-3.03587271687992));
#41981=CARTESIAN_POINT('Ctrl Pts',(-38.9625232142109,4.03620844150535,0.655205949205342));
#41982=CARTESIAN_POINT('Ctrl Pts',(-38.7640500624828,1.63830144967379,3.74649726800244));
#41983=CARTESIAN_POINT('Ctrl Pts',(-38.5655769107546,-2.25933624782354,
3.40817739245239));
#41984=CARTESIAN_POINT('Ctrl Pts',(-38.3671037590265,-4.08873678056746,
-0.0500495593165138));
#41985=CARTESIAN_POINT('Ctrl Pts',(-38.1686306072984,-2.17523389439348,
-3.46246024148072));
#41986=CARTESIAN_POINT('Ctrl Pts',(-37.9701574555703,1.72951734480887,-3.70527234804113));
#41987=CARTESIAN_POINT('Ctrl Pts',(-37.7716843038422,4.05103720219932,-0.556211295777075));
#41988=CARTESIAN_POINT('Ctrl Pts',(-37.573211152114,2.66416451489506,3.10201561194119));
#41989=CARTESIAN_POINT('Ctrl Pts',(-37.3747380003859,-1.16153243685025,
3.92060146116609));
#41990=CARTESIAN_POINT('Ctrl Pts',(-37.1762648486577,-3.92394163925128,
1.15019799639151));
#41991=CARTESIAN_POINT('Ctrl Pts',(-36.9777916969297,-3.09430386836932,
-2.67311746643273));
#41992=CARTESIAN_POINT('Ctrl Pts',(-36.7793185452014,0.567915491803217,
-4.04941297144696));
#41993=CARTESIAN_POINT('Ctrl Pts',(-36.5808453934734,3.7102547643092,-1.71880278190193));
#41994=CARTESIAN_POINT('Ctrl Pts',(-36.3823722417452,3.45615988424496,2.18523048525522));
#41995=CARTESIAN_POINT('Ctrl Pts',(-36.1838990900172,0.0382338892631252,
4.08886433974823));
#41996=CARTESIAN_POINT('Ctrl Pts',(-35.9854259382889,-3.41469209777534,
2.24947800534782));
#41997=CARTESIAN_POINT('Ctrl Pts',(-35.7869527865609,-3.74174732980241,
-1.64912108077893));
#41998=CARTESIAN_POINT('Ctrl Pts',(-35.5884796348327,-0.643539546610226,
-4.0380849757158));
#41999=CARTESIAN_POINT('Ctrl Pts',(-35.3900064831046,3.04377594844649,-2.73051302776818));
#42000=CARTESIAN_POINT('Ctrl Pts',(-35.1915333313765,3.94476402374705,1.07661981038065));
#42001=CARTESIAN_POINT('Ctrl Pts',(-34.9930601796483,1.23464393931464,3.89819544946974));
#42002=CARTESIAN_POINT('Ctrl Pts',(-34.7945870279202,-2.6056914829135,3.15129264192092));
#42003=CARTESIAN_POINT('Ctrl Pts',(-34.5961138761921,-4.06072990916123,
-0.480360306432908));
#42004=CARTESIAN_POINT('Ctrl Pts',(-34.397640724464,-1.79850291188313,-3.67228276350022));
#42005=CARTESIAN_POINT('Ctrl Pts',(-34.1991675727358,2.11010609996108,-3.50253132263795));
#42006=CARTESIAN_POINT('Ctrl Pts',(-34.0006944210077,4.08708591685189,-0.126499515508336));
#42007=CARTESIAN_POINT('Ctrl Pts',(-33.8022212692795,2.32267354525533,3.36533223045274));
#42008=CARTESIAN_POINT('Ctrl Pts',(-33.6037481175514,-1.56795609591073,
3.77647813451229));
#42009=CARTESIAN_POINT('Ctrl Pts',(-33.4052749658233,-4.02325043743371,
0.730567818099445));
#42010=CARTESIAN_POINT('Ctrl Pts',(-33.2068018140952,-2.79558874006392,
-2.98411746008444));
#42011=CARTESIAN_POINT('Ctrl Pts',(-33.008328662367,0.991205328654403,-3.96708777513178));
#42012=CARTESIAN_POINT('Ctrl Pts',(-32.8098555106389,3.87063215595414,-1.31851436565809));
#42013=CARTESIAN_POINT('Ctrl Pts',(-32.6113823589108,3.20681247280386,2.53705088309687));
#42014=CARTESIAN_POINT('Ctrl Pts',(-32.4129092071826,-0.392581206044021,
4.07015397937399));
#42015=CARTESIAN_POINT('Ctrl Pts',(-32.2144360554545,-3.63259896583331,
1.87736468822116));
#42016=CARTESIAN_POINT('Ctrl Pts',(-32.0159629037264,-3.54727009206207,
-2.03399811040102));
#42017=CARTESIAN_POINT('Ctrl Pts',(-31.8174897519982,-0.214706175304816,
-4.08340234087202));
#42018=CARTESIAN_POINT('Ctrl Pts',(-31.6190166002702,3.31440364810769,-2.39478639476751));
#42019=CARTESIAN_POINT('Ctrl Pts',(-31.420543448542,3.80944857276316,1.48606022442755));
#42020=CARTESIAN_POINT('Ctrl Pts',(-31.2220702968139,0.817255542910768,
4.0065405023205));
#42021=CARTESIAN_POINT('Ctrl Pts',(-31.0235971450857,-2.92306795604602,
2.85936131740812));
#42022=CARTESIAN_POINT('Ctrl Pts',(-30.8251239933576,-3.98756230933313,
-0.905328806754085));
#42023=CARTESIAN_POINT('Ctrl Pts',(-30.6266508416295,-1.40177018008474,
-3.84126460705041));
#42024=CARTESIAN_POINT('Ctrl Pts',(-30.4281776899013,2.46722766309277,-3.26083748101967));
#42025=CARTESIAN_POINT('Ctrl Pts',(-30.2297045381732,4.07768078915179,0.304619107961798));
#42026=CARTESIAN_POINT('Ctrl Pts',(-30.031231386445,1.95535135030967,3.5912218695028));
#42027=CARTESIAN_POINT('Ctrl Pts',(-29.832758234717,-1.95694199353205,3.59035533799984));
#42028=CARTESIAN_POINT('Ctrl Pts',(-29.6342850829888,-4.07781532886962,
0.302812752024875));
#42029=CARTESIAN_POINT('Ctrl Pts',(-29.4358119312607,-2.46578293922098,
-3.26193009057516));
#42030=CARTESIAN_POINT('Ctrl Pts',(-29.2373387795326,1.40347164124787,-3.84064327572426));
#42031=CARTESIAN_POINT('Ctrl Pts',(-29.0388656278044,3.98796295954069,-0.903562312452452));
#42032=CARTESIAN_POINT('Ctrl Pts',(-28.8403924760763,2.92180103286938,2.86065589392999));
#42033=CARTESIAN_POINT('Ctrl Pts',(-28.6419193243482,-0.819030275137617,
4.00617808235744));
#42034=CARTESIAN_POINT('Ctrl Pts',(-28.4434461726201,-3.81010649213961,
1.48437257375252));
#42035=CARTESIAN_POINT('Ctrl Pts',(-28.2449730208919,-3.31334248336611,
-2.39625437027754));
#42036=CARTESIAN_POINT('Ctrl Pts',(-28.0464998691638,0.216515014814097,
-4.08330682994959));
#42037=CARTESIAN_POINT('Ctrl Pts',(-27.8480267174356,3.54817076201677,-2.03242654546783));
#42038=CARTESIAN_POINT('Ctrl Pts',(-27.6495535657076,3.63176697670682,1.87897366827073));
#42039=CARTESIAN_POINT('Ctrl Pts',(-27.4510804139794,0.390778175693683,
4.07032748517296));
#42040=CARTESIAN_POINT('Ctrl Pts',(-27.2526072622513,-3.20793601786463,
2.53563008430642));
#42041=CARTESIAN_POINT('Ctrl Pts',(-27.0541341105231,-3.87004770230544,
-1.32022884419077));
#42042=CARTESIAN_POINT('Ctrl Pts',(-26.855660958795,-0.98944789571108,-3.96752646882488));
#42043=CARTESIAN_POINT('Ctrl Pts',(-26.6571878070669,2.79691036647756,-2.98287878081619));
#42044=CARTESIAN_POINT('Ctrl Pts',(-26.4587146553387,4.02292641665342,0.732349960978325));
#42045=CARTESIAN_POINT('Ctrl Pts',(-26.2602415036106,1.56628304240493,3.77717233525659));
#42046=CARTESIAN_POINT('Ctrl Pts',(-26.0617683518825,-2.32416408812179,
3.36430300517625));
#42047=CARTESIAN_POINT('Ctrl Pts',(-25.8632952001543,-4.08702947924636,
-0.12830999541797));
#42048=CARTESIAN_POINT('Ctrl Pts',(-25.6648220484262,-2.10855434588592,
-3.50346571120634));
#42049=CARTESIAN_POINT('Ctrl Pts',(-25.4663488966981,1.80012947875039,-3.67148570457339));
#42050=CARTESIAN_POINT('Ctrl Pts',(-25.26787574497,4.06094230016339,-0.478561442133215));
#42051=CARTESIAN_POINT('Ctrl Pts',(-25.0694025932418,2.60429527149516,3.15244659875803));
#42052=CARTESIAN_POINT('Ctrl Pts',(-24.8709294415137,-1.23637063603042,
3.89764814593555));
#42053=CARTESIAN_POINT('Ctrl Pts',(-24.6724562897856,-3.94524055643307,
1.07487225800491));
#42054=CARTESIAN_POINT('Ctrl Pts',(-24.4739831380575,-3.0425660904843,-2.73186108801089));
#42055=CARTESIAN_POINT('Ctrl Pts',(-24.2755099863293,0.645328269413449,
-4.03779950515733));
#42056=CARTESIAN_POINT('Ctrl Pts',(-24.0770368346012,3.74247748832006,-1.64746340431906));
#42057=CARTESIAN_POINT('Ctrl Pts',(-23.878563682873,3.41369529172666,2.25099042076953));
#42058=CARTESIAN_POINT('Ctrl Pts',(-23.6800905311449,-0.0400451656365475,
4.08884700176738));
#42059=CARTESIAN_POINT('Ctrl Pts',(-23.4816173794168,-3.45712755587142,
2.18369926537229));
#42060=CARTESIAN_POINT('Ctrl Pts',(-23.2831442276887,-3.70949300712285,
-1.72044617737949));
#42061=CARTESIAN_POINT('Ctrl Pts',(-23.0846710759605,-0.56612163207619,
-4.04966414864845));
#42062=CARTESIAN_POINT('Ctrl Pts',(-22.8861979242324,3.09548769907761,-2.67174649321603));
#42063=CARTESIAN_POINT('Ctrl Pts',(-22.6877247725043,3.9234317409515,1.15193610640832));
#42064=CARTESIAN_POINT('Ctrl Pts',(-22.4892516207761,1.1597955796458,3.92111561071425));
#42065=CARTESIAN_POINT('Ctrl Pts',(-22.290778469048,-2.66553838058246,3.10083513924794));
#42066=CARTESIAN_POINT('Ctrl Pts',(-22.0923053173199,-4.0507904149318,-0.558005764709968));
#42067=CARTESIAN_POINT('Ctrl Pts',(-21.8938321655918,-1.72787581810372,
-3.70603812397624));
#42068=CARTESIAN_POINT('Ctrl Pts',(-21.6953590138636,2.17676747737354,-3.46149631931074));
#42069=CARTESIAN_POINT('Ctrl Pts',(-21.4968858621355,4.08875855029321,-0.0482383307871566));
#42070=CARTESIAN_POINT('Ctrl Pts',(-21.2984127104073,2.25782627589523,3.40917789606675));
#42071=CARTESIAN_POINT('Ctrl Pts',(-21.0999395586792,-1.63996090770976,
3.74577116764184));
#42072=CARTESIAN_POINT('Ctrl Pts',(-20.9014664069511,-4.03649828782243,
0.653417930240319));
#42073=CARTESIAN_POINT('Ctrl Pts',(-20.702993255223,-2.73795230777559,-3.03708586962885));
#42074=CARTESIAN_POINT('Ctrl Pts',(-20.5045201034949,1.06696461361248,-3.94738646859561));
#42075=CARTESIAN_POINT('Ctrl Pts',(-20.3060469517667,3.89516287726385,-1.24417827450031));
#42076=CARTESIAN_POINT('Ctrl Pts',(-20.1075738000386,3.15765876558903,2.59797315984052));
#42077=CARTESIAN_POINT('Ctrl Pts',(-19.9091006483104,-0.47042315135575,
4.06189309039781));
#42078=CARTESIAN_POINT('Ctrl Pts',(-19.7106274965824,-3.66787122806022,
1.80748280033891));
#42079=CARTESIAN_POINT('Ctrl Pts',(-19.5121543448542,-3.50768380597088,
-2.10152985619589));
#42080=CARTESIAN_POINT('Ctrl Pts',(-19.3136811931261,-0.136499341408789,
-4.08676416605462));
#42081=CARTESIAN_POINT('Ctrl Pts',(-19.1152080413979,3.3596390830333,-2.33090082391081));
#42082=CARTESIAN_POINT('Ctrl Pts',(-18.9167348896698,3.78030327543875,1.55871118712222));
#42083=CARTESIAN_POINT('Ctrl Pts',(-18.7182617379417,0.740409644353662,
4.02145085481609));
#42084=CARTESIAN_POINT('Ctrl Pts',(-18.5197885862136,-2.9772683338242,2.80288185401394));
#42085=CARTESIAN_POINT('Ctrl Pts',(-18.3213154344854,-3.9695011626178,-0.981495766230743));
#42086=CARTESIAN_POINT('Ctrl Pts',(-18.1228422827573,-1.32798100844273,
-3.86739445368175));
#42087=CARTESIAN_POINT('Ctrl Pts',(-17.9243691310291,2.52919692061813,-3.2130104817583));
#42088=CARTESIAN_POINT('Ctrl Pts',(-17.725895979301,4.07110235615733,0.382621255085668));
#42089=CARTESIAN_POINT('Ctrl Pts',(-17.5274228275729,1.88624724304817,3.62799459167821));
#42090=CARTESIAN_POINT('Ctrl Pts',(-17.3289496758448,-2.02531262848022,
3.55223622188495));
#42091=CARTESIAN_POINT('Ctrl Pts',(-17.1304765241166,-4.08286477871325,
0.224696724265731));
#42092=CARTESIAN_POINT('Ctrl Pts',(-16.9320033723885,-2.40288884646982,
-3.30853420877946));
#42093=CARTESIAN_POINT('Ctrl Pts',(-16.7335302206604,1.47673488933885,-3.81307323372661));
#42094=CARTESIAN_POINT('Ctrl Pts',(-16.5350570689322,4.0045288638356,-0.827056224122942));
#42095=CARTESIAN_POINT('Ctrl Pts',(-16.3365839172041,2.86650486569058,2.91606297499303));
#42096=CARTESIAN_POINT('Ctrl Pts',(-16.138110765476,-0.895569404687675,
3.98976551448081));
#42097=CARTESIAN_POINT('Ctrl Pts',(-15.9396376137478,-3.83782328393318,
1.41116471769011));
#42098=CARTESIAN_POINT('Ctrl Pts',(-15.7411644620197,-3.26686448612226,
-2.45924172225226));
#42099=CARTESIAN_POINT('Ctrl Pts',(-15.5426913102916,0.294641003851046,
-4.07841391940575));
#42100=CARTESIAN_POINT('Ctrl Pts',(-15.3442181585635,3.5864268029142,-1.96413243099634));
#42101=CARTESIAN_POINT('Ctrl Pts',(-15.1457450068353,3.5951327994024,1.94815132210359));
#42102=CARTESIAN_POINT('Ctrl Pts',(-14.9472718551072,0.312789367054645,
4.07706220592849));
#42103=CARTESIAN_POINT('Ctrl Pts',(-14.7487987033791,-3.255887095317,2.47375678709552));
#42104=CARTESIAN_POINT('Ctrl Pts',(-14.5503255516509,-3.84406576712621,
-1.39407022676811));
#42105=CARTESIAN_POINT('Ctrl Pts',(-14.3518523999228,-0.913317280135754,
-3.98574020289311));
#42106=CARTESIAN_POINT('Ctrl Pts',(-14.1533792481947,2.85349832338418,-2.92879168559267));
#42107=CARTESIAN_POINT('Ctrl Pts',(-13.9549060964666,4.00817007816534,0.809225582673443));
#42108=CARTESIAN_POINT('Ctrl Pts',(-13.7564329447384,1.49369062701152,3.80646315231487));
#42109=CARTESIAN_POINT('Ctrl Pts',(-13.5579597930103,-2.38814017363929,
3.31919567519045));
#42110=CARTESIAN_POINT('Ctrl Pts',(-13.3594866412822,-4.0838243719331,-0.206523408741399));
#42111=CARTESIAN_POINT('Ctrl Pts',(-13.161013489554,-2.04110205880377,-3.54318723816566));
#42112=CARTESIAN_POINT('Ctrl Pts',(-12.9625403378259,1.8700819050158,-3.63635354272455));
#42113=CARTESIAN_POINT('Ctrl Pts',(-12.7640671860978,4.06935915250997,-0.400736206295686));
#42114=CARTESIAN_POINT('Ctrl Pts',(-12.5655940343697,2.54347161142596,3.20172228355665));
#42115=CARTESIAN_POINT('Ctrl Pts',(-12.3671208826415,-1.31075573269272,
3.87326642878672));
#42116=CARTESIAN_POINT('Ctrl Pts',(-12.1686477309134,-3.96509363012978,
0.999152602687558));
#42117=CARTESIAN_POINT('Ctrl Pts',(-11.9701745791853,-2.9897132793594,-2.7896035428668));
#42118=CARTESIAN_POINT('Ctrl Pts',(-11.7717014274571,0.722504548472898,
-4.0247062745732));
#42119=CARTESIAN_POINT('Ctrl Pts',(-11.573228275729,3.77332867702978,-1.57552026780286));
#42120=CARTESIAN_POINT('Ctrl Pts',(-11.3747551240009,3.36997965531711,2.31592541803525));
#42121=CARTESIAN_POINT('Ctrl Pts',(-11.1762819722727,-0.118309544867903,
4.08733119171252));
#42122=CARTESIAN_POINT('Ctrl Pts',(-10.9778088205446,-3.49829605311116,
2.11712024786968));
#42123=CARTESIAN_POINT('Ctrl Pts',(-10.7793356688165,-3.67587923722566,
-1.79114076847305));
#42124=CARTESIAN_POINT('Ctrl Pts',(-10.5808625170884,-0.488496246473859,
-4.05975920915685));
#42125=CARTESIAN_POINT('Ctrl Pts',(-10.3823893653602,3.1460650218686,-2.61200082261243));
#42126=CARTESIAN_POINT('Ctrl Pts',(-10.1839162136321,3.90066160711989,1.22683024330753));
#42127=CARTESIAN_POINT('Ctrl Pts',(-9.98544306190397,1.08452218052527,3.94259876973319));
#42128=CARTESIAN_POINT('Ctrl Pts',(-9.78696991017584,-2.7244084173359,3.04924124901626));
#42129=CARTESIAN_POINT('Ctrl Pts',(-9.5884967584477,-4.0393663955265,-0.635446726204635));
#42130=CARTESIAN_POINT('Ctrl Pts',(-9.39002360671958,-1.65661549601823,
-3.73843530337295));
#42131=CARTESIAN_POINT('Ctrl Pts',(-9.19155045499145,2.24263111760604,-3.41919275407193));
#42132=CARTESIAN_POINT('Ctrl Pts',(-8.99307730326332,4.08893274407603,0.0300405322163189));
#42133=CARTESIAN_POINT('Ctrl Pts',(-8.79460415153519,2.19215156309674,3.45177417331515));
#42134=CARTESIAN_POINT('Ctrl Pts',(-8.59613099980706,-1.71136471007461,
3.71369145840958));
#42135=CARTESIAN_POINT('Ctrl Pts',(-8.39765784807893,-4.04826685078408,
0.576028579148569));
#42136=CARTESIAN_POINT('Ctrl Pts',(-8.1991846963508,-2.67931247646759,-3.0889412543132));
#42137=CARTESIAN_POINT('Ctrl Pts',(-8.00071154462267,1.14233287961659,-3.92623853214494));
#42138=CARTESIAN_POINT('Ctrl Pts',(-7.80223839289453,3.91826610745135,-1.16938621949784));
#42139=CARTESIAN_POINT('Ctrl Pts',(-7.60376524116641,3.10734784621199,2.65794333682912));
#42140=CARTESIAN_POINT('Ctrl Pts',(-7.40529208943829,-0.548092696977365,
4.05214360736044));
#42141=CARTESIAN_POINT('Ctrl Pts',(-7.20681893771015,-3.70179929653215,
1.73693850995084));
#42142=CARTESIAN_POINT('Ctrl Pts',(-7.00834578598201,-3.46681203127418,
-2.16829143773666));
#42143=CARTESIAN_POINT('Ctrl Pts',(-6.8098726342539,-0.058242483521796,
-4.08862828247588));
#42144=CARTESIAN_POINT('Ctrl Pts',(-6.61139948252575,3.40364328447616,-2.26616102940976));
#42145=CARTESIAN_POINT('Ctrl Pts',(-6.41292633079764,3.74977258049331,1.63079091661213));
#42146=CARTESIAN_POINT('Ctrl Pts',(-6.2144531790695,0.663292402032029,4.03488743443219));
#42147=CARTESIAN_POINT('Ctrl Pts',(-6.01598002734137,-3.03037760856484,
2.74537519636395));
#42148=CARTESIAN_POINT('Ctrl Pts',(-5.81750687561324,-3.9499852814079,-1.05730302921229));
#42149=CARTESIAN_POINT('Ctrl Pts',(-5.61903372388512,-1.25370516116971,
-3.89210698567597));
#42150=CARTESIAN_POINT('Ctrl Pts',(-5.42056057215698,2.59023928348237,-3.16400598520845));
#42151=CARTESIAN_POINT('Ctrl Pts',(-5.22208742042886,4.06303195387578,0.460483180078377));
#42152=CARTESIAN_POINT('Ctrl Pts',(-5.02361426870073,1.81645186829979,3.6634377338051));
#42153=CARTESIAN_POINT('Ctrl Pts',(-4.82514111697259,-2.09294103195811,
3.51281529007031));
#42154=CARTESIAN_POINT('Ctrl Pts',(-4.62666796524447,-4.08641794720157,
0.146498349393829));
#42155=CARTESIAN_POINT('Ctrl Pts',(-4.42819481351633,-2.33911415117824,
-3.35392582091246));
#42156=CARTESIAN_POINT('Ctrl Pts',(-4.2297216617882,1.54945695270031,-3.78410578731147));
#42157=CARTESIAN_POINT('Ctrl Pts',(-4.03124851006007,4.01962718536272,-0.750247032867542));
#42158=CARTESIAN_POINT('Ctrl Pts',(-3.83277535833195,2.81015820967587,2.97040137366801));
#42159=CARTESIAN_POINT('Ctrl Pts',(-3.63430220660382,-0.971780369637932,
3.97189080434176));
#42160=CARTESIAN_POINT('Ctrl Pts',(-3.43582905487568,-3.86413351836361,
1.33743966530148));
#42161=CARTESIAN_POINT('Ctrl Pts',(-3.23735590314755,-3.219189408103,-2.52132774831895));
#42162=CARTESIAN_POINT('Ctrl Pts',(-3.03888275141943,0.372659305824992,
-4.07202649063205));
#42163=CARTESIAN_POINT('Ctrl Pts',(-2.8404095996913,3.62336793852966,-1.8951182561049));
#42164=CARTESIAN_POINT('Ctrl Pts',(-2.64193644796316,3.55718215462882,2.01661454478224));
#42165=CARTESIAN_POINT('Ctrl Pts',(-2.44346329623504,0.234683883134984,
4.08230368521807));
#42166=CARTESIAN_POINT('Ctrl Pts',(-2.24499014450691,-3.30264105137573,
2.41097516903988));
#42167=CARTESIAN_POINT('Ctrl Pts',(-2.04651699277877,-3.81668254578493,
-1.4673973788029));
#42168=CARTESIAN_POINT('Ctrl Pts',(-1.84804384105064,-0.836837650855956,
-4.00249962847716));
#42169=CARTESIAN_POINT('Ctrl Pts',(-1.64957068932252,2.90901318244003,-2.87361905689455));
#42170=CARTESIAN_POINT('Ctrl Pts',(-1.45109753759438,3.99199714630452,0.885781316882712));
#42171=CARTESIAN_POINT('Ctrl Pts',(-1.25262438586625,1.42045076229673,3.83440359121586));
#42172=CARTESIAN_POINT('Ctrl Pts',(-1.05415123413812,-2.45104972378982,
3.27278662218134));
#42173=CARTESIAN_POINT('Ctrl Pts',(-0.855678082410002,-4.07948859958104,
-0.28449794668778));
#42174=CARTESIAN_POINT('Ctrl Pts',(-0.657204930681864,-1.97220141068763,
-3.58192268475822));
#42175=CARTESIAN_POINT('Ctrl Pts',(-0.458731778953736,1.93800556216186,
-3.59928830058453));
#42176=CARTESIAN_POINT('Ctrl Pts',(-0.26025862722561,4.07889020629659,-0.323938792483296));
#42177=CARTESIAN_POINT('Ctrl Pts',(-0.0617854754974834,2.47640913824184,
3.25230520610813));
#42178=CARTESIAN_POINT('Ctrl Pts',(0.070529958987943,-0.0890080456892121,
3.64468494608818));
#42179=CARTESIAN_POINT('Ctrl Pts',(0.136687676230653,-1.17148016637959,
3.25511512389028));
#42180=CARTESIAN_POINT('Ctrl Pts',(-54.7036876762307,-1.64343044862466,
3.31080057131706));
#42181=CARTESIAN_POINT('Ctrl Pts',(-54.6375299589879,-2.74442048406567,
2.76428606254484));
#42182=CARTESIAN_POINT('Ctrl Pts',(-54.5052145245025,-4.33928981056137,
0.495999601472129));
#42183=CARTESIAN_POINT('Ctrl Pts',(-54.3067413727745,-2.76702521143321,
-3.38463735892371));
#42184=CARTESIAN_POINT('Ctrl Pts',(-54.1082682210462,1.34187477797974,-4.15638860970085));
#42185=CARTESIAN_POINT('Ctrl Pts',(-53.9097950693182,4.22052442796764,-1.12856074917905));
#42186=CARTESIAN_POINT('Ctrl Pts',(-53.71132191759,3.23660588578034,2.93509109597859));
#42187=CARTESIAN_POINT('Ctrl Pts',(-53.512848765862,-0.710670000578388,
4.31048894467319));
#42188=CARTESIAN_POINT('Ctrl Pts',(-53.3143756141337,-4.00711916051023,
1.7407288929608));
#42189=CARTESIAN_POINT('Ctrl Pts',(-53.1159024624056,-3.6355185340518,-2.42291345406673));
#42190=CARTESIAN_POINT('Ctrl Pts',(-52.9174293106775,0.0641742371961704,
-4.36837440997313));
#42191=CARTESIAN_POINT('Ctrl Pts',(-52.7189561589494,3.70508264242447,-2.31505260596812));
#42192=CARTESIAN_POINT('Ctrl Pts',(-52.5204830072212,3.95431147698897,1.8575655438389));
#42193=CARTESIAN_POINT('Ctrl Pts',(-52.3220098554931,0.583681820532341,
4.32970570060305));
#42194=CARTESIAN_POINT('Ctrl Pts',(-52.123536703765,-3.32125525664554,2.83837029465124));
#42195=CARTESIAN_POINT('Ctrl Pts',(-51.9250635520368,-4.18585819809453,
-1.25126841311442));
#42196=CARTESIAN_POINT('Ctrl Pts',(-51.7265904003087,-1.21864953295622,
-4.19546929666802));
#42197=CARTESIAN_POINT('Ctrl Pts',(-51.5281172485806,2.86413212282785,-3.2990640568009));
#42198=CARTESIAN_POINT('Ctrl Pts',(-51.3296440968525,4.32503596533597,0.617365075992241));
#42199=CARTESIAN_POINT('Ctrl Pts',(-51.1311709451243,1.82672363883074,3.96864648723083));
#42200=CARTESIAN_POINT('Ctrl Pts',(-50.9326977933962,-2.34380435348219,
3.6869576105009));
#42201=CARTESIAN_POINT('Ctrl Pts',(-50.7342246416681,-4.36877161136301,
0.0301610541736334));
#42202=CARTESIAN_POINT('Ctrl Pts',(-50.5357514899399,-2.39448648330802,
-3.65424539063146));
#42203=CARTESIAN_POINT('Ctrl Pts',(-50.3372783382118,1.77175475755383,-3.99348971834736));
#42204=CARTESIAN_POINT('Ctrl Pts',(-50.1388051864837,4.31609973524516,-0.677021483217761));
#42205=CARTESIAN_POINT('Ctrl Pts',(-49.9403320347555,2.90940913881518,3.25920442052877));
#42206=CARTESIAN_POINT('Ctrl Pts',(-49.7418588830275,-1.16060707327924,
4.21189580069286));
#42207=CARTESIAN_POINT('Ctrl Pts',(-49.5433857312992,-4.16818263172822,
1.3089417695408));
#42208=CARTESIAN_POINT('Ctrl Pts',(-49.3449125795711,-3.36012860510288,
-2.79224117196468));
#42209=CARTESIAN_POINT('Ctrl Pts',(-49.1464394278431,0.523847770568201,
-4.33735616726239));
#42210=CARTESIAN_POINT('Ctrl Pts',(-48.9479662761149,3.92828444584205,-1.91197707093674));
#42211=CARTESIAN_POINT('Ctrl Pts',(-48.7494931243868,3.7366986642368,2.26366033223368));
#42212=CARTESIAN_POINT('Ctrl Pts',(-48.5510199726586,0.12447150700683,4.36710222589484));
#42213=CARTESIAN_POINT('Ctrl Pts',(-48.3525468209305,-3.60169911350682,
2.47281994958047));
#42214=CARTESIAN_POINT('Ctrl Pts',(-48.1540736692024,-4.03080938276955,
-1.68512632376529));
#42215=CARTESIAN_POINT('Ctrl Pts',(-47.9556005174743,-0.770044018205449,
-4.30047755689456));
#42216=CARTESIAN_POINT('Ctrl Pts',(-47.7571273657461,3.19563353394943,-2.97909404416766));
#42217=CARTESIAN_POINT('Ctrl Pts',(-47.558654214018,4.23597049272536,1.06940590612676));
#42218=CARTESIAN_POINT('Ctrl Pts',(-47.3601810622898,1.39862363604842,4.13895239547316));
#42219=CARTESIAN_POINT('Ctrl Pts',(-47.1617079105618,-2.71904853137658,
3.41962718601319));
#42220=CARTESIAN_POINT('Ctrl Pts',(-46.9632347588336,-4.34765461544227,
-0.43008644727046));
#42221=CARTESIAN_POINT('Ctrl Pts',(-46.7647616071055,-1.99633922308703,
-3.8860911869985));
#42222=CARTESIAN_POINT('Ctrl Pts',(-46.5662884553773,2.18246111252143,-3.78469794034269));
#42223=CARTESIAN_POINT('Ctrl Pts',(-46.3678153036492,4.36339716923192,-0.218723914653743));
#42224=CARTESIAN_POINT('Ctrl Pts',(-46.169342151921,2.55000073175133,3.54747392877952));
#42225=CARTESIAN_POINT('Ctrl Pts',(-45.970869000193,-1.59771238330974,4.06625013341793));
#42226=CARTESIAN_POINT('Ctrl Pts',(-45.7723958484648,-4.28285075637247,
0.862707601648684));
#42227=CARTESIAN_POINT('Ctrl Pts',(-45.5739226967367,-3.04739027481367,
-3.13057303385079));
#42228=CARTESIAN_POINT('Ctrl Pts',(-45.3754495450085,0.977706246068333,
-4.25807063160085));
#42229=CARTESIAN_POINT('Ctrl Pts',(-45.1769763932805,4.10779282928477,-1.48765354803437));
#42230=CARTESIAN_POINT('Ctrl Pts',(-44.9785032415523,3.47753174277359,2.644588434011));
#42231=CARTESIAN_POINT('Ctrl Pts',(-44.7800300898242,-0.336124643548603,
4.35592644925301));
#42232=CARTESIAN_POINT('Ctrl Pts',(-44.581556938096,-3.84208646672359,2.07977080216117));
#42233=CARTESIAN_POINT('Ctrl Pts',(-44.3830837863679,-3.83093301839846,
-2.1002445609612));
#42234=CARTESIAN_POINT('Ctrl Pts',(-44.1846106346398,-0.312874366403276,
-4.35765815985495));
#42235=CARTESIAN_POINT('Ctrl Pts',(-43.9861374829117,3.4915951255531,-2.62599285728587));
#42236=CARTESIAN_POINT('Ctrl Pts',(-43.7876643311835,4.09979544336713,1.50955368564645));
#42237=CARTESIAN_POINT('Ctrl Pts',(-43.5891911794554,0.954969042813313,
4.26322754900215));
#42238=CARTESIAN_POINT('Ctrl Pts',(-43.3907180277272,-3.06405324931624,
3.1142659958098));
#42239=CARTESIAN_POINT('Ctrl Pts',(-43.1922448759992,-4.2781859146255,-0.885550838293665));
#42240=CARTESIAN_POINT('Ctrl Pts',(-42.993771724271,-1.57599000561263,-4.07471845769885));
#42241=CARTESIAN_POINT('Ctrl Pts',(-42.7952985725428,2.5688955889342,-3.53381528386206));
#42242=CARTESIAN_POINT('Ctrl Pts',(-42.5968254208148,4.36216781272975,0.242006158779532));
#42243=CARTESIAN_POINT('Ctrl Pts',(-42.3983522690865,2.1622329174566,3.79629079734019));
#42244=CARTESIAN_POINT('Ctrl Pts',(-42.1998791173585,-2.01704900199012,
3.87538234641091));
#42245=CARTESIAN_POINT('Ctrl Pts',(-42.0014059656303,-4.34988787292489,
0.406878974983359));
#42246=CARTESIAN_POINT('Ctrl Pts',(-41.8029328139022,-2.70076090324605,
-3.43408875115367));
#42247=CARTESIAN_POINT('Ctrl Pts',(-41.6044596621741,1.4206913250513,-4.13142967581763));
#42248=CARTESIAN_POINT('Ctrl Pts',(-41.4059865104459,4.24161708193722,-1.04678533497605));
#42249=CARTESIAN_POINT('Ctrl Pts',(-41.2075133587178,3.17969003372768,2.99610518785898));
#42250=CARTESIAN_POINT('Ctrl Pts',(-41.0090402069897,-0.792982640099472,
4.2963069652672));
#42251=CARTESIAN_POINT('Ctrl Pts',(-40.8105670552616,-4.03974469799334,
1.66359183165144));
#42252=CARTESIAN_POINT('Ctrl Pts',(-40.6120939035334,-3.58845157328471,
-2.49200527958776));
#42253=CARTESIAN_POINT('Ctrl Pts',(-40.4136207518053,0.147774865327506,
-4.36637579652508));
#42254=CARTESIAN_POINT('Ctrl Pts',(-40.2151476000772,3.74872552602871,-2.24368713010601));
#42255=CARTESIAN_POINT('Ctrl Pts',(-40.016674448349,3.91802520478279,1.93291321636264));
#42256=CARTESIAN_POINT('Ctrl Pts',(-39.8182012966209,0.500693921112148,
4.34008993048116));
#42257=CARTESIAN_POINT('Ctrl Pts',(-39.6197281448928,-3.37498161158642,
2.77427001727592));
#42258=CARTESIAN_POINT('Ctrl Pts',(-39.4212549931647,-4.16113808479721,
-1.33116672380013));
#42259=CARTESIAN_POINT('Ctrl Pts',(-39.2227818414366,-1.1381136789162,-4.21802942867477));
#42260=CARTESIAN_POINT('Ctrl Pts',(-39.0243086897083,2.92676052276938,-3.24363189182457));
#42261=CARTESIAN_POINT('Ctrl Pts',(-38.8258355379803,4.3124253365845,0.700044801199802));
#42262=CARTESIAN_POINT('Ctrl Pts',(-38.6273623862521,1.75041819146013,4.00288785282676));
#42263=CARTESIAN_POINT('Ctrl Pts',(-38.428889234524,-2.41395334759883,3.64141514289692));
#42264=CARTESIAN_POINT('Ctrl Pts',(-38.2304160827959,-4.36854843913065,
-0.0534746881410977));
#42265=CARTESIAN_POINT('Ctrl Pts',(-38.0319429310678,-2.32409547106562,
-3.69941282485139));
#42266=CARTESIAN_POINT('Ctrl Pts',(-37.8334697793396,1.84787642311034,-3.95884171598405));
#42267=CARTESIAN_POINT('Ctrl Pts',(-37.6349966276115,4.32826889973387,-0.594275473916914));
#42268=CARTESIAN_POINT('Ctrl Pts',(-37.4365234758834,2.84648593385764,3.31430125903684));
#42269=CARTESIAN_POINT('Ctrl Pts',(-37.2380503241552,-1.24102161286549,
4.18890682203643));
#42270=CARTESIAN_POINT('Ctrl Pts',(-37.0395771724271,-4.1924755843569,1.22891150286507));
#42271=CARTESIAN_POINT('Ctrl Pts',(-36.841104020699,-3.30606176426067,-2.85605157835015));
#42272=CARTESIAN_POINT('Ctrl Pts',(-36.6426308689708,0.606780643612692,
-4.32653351516425));
#42273=CARTESIAN_POINT('Ctrl Pts',(-36.4441577172427,3.96416510263855,-1.83642861182384));
#42274=CARTESIAN_POINT('Ctrl Pts',(-36.2456845655146,3.69268130427524,2.33477617607313));
#42275=CARTESIAN_POINT('Ctrl Pts',(-36.0472114137865,0.040850415721449,
4.36868472779142));
#42276=CARTESIAN_POINT('Ctrl Pts',(-35.8487382620583,-3.64837568041693,
2.40342045881384));
#42277=CARTESIAN_POINT('Ctrl Pts',(-35.6502651103302,-3.9978128538176,-1.76197826126017));
#42278=CARTESIAN_POINT('Ctrl Pts',(-35.4517919586021,-0.68758001131886,
-4.31443029093499));
#42279=CARTESIAN_POINT('Ctrl Pts',(-35.2533188068739,3.25207597902751,-2.91737499028409));
#42280=CARTESIAN_POINT('Ctrl Pts',(-35.0548456551459,4.21472294342388,1.15029801246422));
#42281=CARTESIAN_POINT('Ctrl Pts',(-34.8563725034176,1.31913648235043,4.16496746064537));
#42282=CARTESIAN_POINT('Ctrl Pts',(-34.6578993516896,-2.7840113148488,3.36695054999275));
#42283=CARTESIAN_POINT('Ctrl Pts',(-34.4594261999614,-4.33862492462412,
-0.513233641466429));
#42284=CARTESIAN_POINT('Ctrl Pts',(-34.2609530482333,-1.92158299986923,
-3.92359449764067));
#42285=CARTESIAN_POINT('Ctrl Pts',(-34.0624798965052,2.25451067263522,-3.74222616022556));
#42286=CARTESIAN_POINT('Ctrl Pts',(-33.864006744777,4.36678459897784,-0.135156477582659));
#42287=CARTESIAN_POINT('Ctrl Pts',(-33.6655335930489,2.48162511682313,3.59563788316554));
#42288=CARTESIAN_POINT('Ctrl Pts',(-33.4670604413208,-1.67525877135726,
4.03492045228817));
#42289=CARTESIAN_POINT('Ctrl Pts',(-33.2685872895926,-4.29858055480978,
0.78056404036699));
#42290=CARTESIAN_POINT('Ctrl Pts',(-33.0701141378645,-2.98690414235031,
-3.18833477723296));
#42291=CARTESIAN_POINT('Ctrl Pts',(-32.8716409861363,1.0590382124698,-4.23857441503996));
#42292=CARTESIAN_POINT('Ctrl Pts',(-32.6731678344083,4.13551788016929,-1.40874655992579));
#42293=CARTESIAN_POINT('Ctrl Pts',(-32.4746946826801,3.42626986633934,2.71067331309355));
#42294=CARTESIAN_POINT('Ctrl Pts',(-32.276221530952,-0.419447400734403,
4.34869392867786));
#42295=CARTESIAN_POINT('Ctrl Pts',(-32.0777483792239,-3.88119494940355,
2.00584166175373));
#42296=CARTESIAN_POINT('Ctrl Pts',(-31.8792752274957,-3.79002661592259,
-2.17319425222436));
#42297=CARTESIAN_POINT('Ctrl Pts',(-31.6808020757676,-0.229399537641264,
-4.36284893841544));
#42298=CARTESIAN_POINT('Ctrl Pts',(-31.4823289240394,3.54122401627932,-2.55867299079608));
#42299=CARTESIAN_POINT('Ctrl Pts',(-31.2838557723114,4.07014721407014,1.58775837680034));
#42300=CARTESIAN_POINT('Ctrl Pts',(-31.0853826205832,0.873184217512199,
4.28072707954971));
#42301=CARTESIAN_POINT('Ctrl Pts',(-30.8869094688551,-3.12310736595907,
3.05504097975702));
#42302=CARTESIAN_POINT('Ctrl Pts',(-30.688436317127,-4.26045011876644,-0.967284752699883));
#42303=CARTESIAN_POINT('Ctrl Pts',(-30.4899631653988,-1.49769996477461,
-4.10414057054783));
#42304=CARTESIAN_POINT('Ctrl Pts',(-30.2914900136707,2.63607175884002,-3.48399206221092));
#42305=CARTESIAN_POINT('Ctrl Pts',(-30.0930168619426,4.35673583376276,0.325465638908587));
#42306=CARTESIAN_POINT('Ctrl Pts',(-29.8945437102144,2.08916532116829,3.83698622204075));
#42307=CARTESIAN_POINT('Ctrl Pts',(-29.6960705584864,-2.09086481965406,
3.8360603896753));
#42308=CARTESIAN_POINT('Ctrl Pts',(-29.4975974067581,-4.35687958067188,
0.323535665463647));
#42309=CARTESIAN_POINT('Ctrl Pts',(-29.2991242550301,-2.63452816565838,
-3.48515944422279));
#42310=CARTESIAN_POINT('Ctrl Pts',(-29.1006511033019,1.49951786499866,-4.10347671857079));
#42311=CARTESIAN_POINT('Ctrl Pts',(-28.9021779515738,4.2608781873688,-0.965397368811076));
#42312=CARTESIAN_POINT('Ctrl Pts',(-28.7037047998456,3.12175374121783,3.05642415029312));
#42313=CARTESIAN_POINT('Ctrl Pts',(-28.5052316481175,-0.875080403086531,
4.28033985746888));
#42314=CARTESIAN_POINT('Ctrl Pts',(-28.3067584963894,-4.07085015799139,
1.58595523218163));
#42315=CARTESIAN_POINT('Ctrl Pts',(-28.1082853446612,-3.54009023099919,
-2.56024142683588));
#42316=CARTESIAN_POINT('Ctrl Pts',(-27.9098121929331,0.231332164621206,
-4.36274689122739));
#42317=CARTESIAN_POINT('Ctrl Pts',(-27.711339041205,3.79098892299601,-2.17151513764563));
#42318=CARTESIAN_POINT('Ctrl Pts',(-27.5128658894769,3.8803060233133,2.00756075194279));
#42319=CARTESIAN_POINT('Ctrl Pts',(-27.3143927377488,0.417520980461716,
4.34887930830195));
#42320=CARTESIAN_POINT('Ctrl Pts',(-27.1159195860206,-3.42747030091991,
2.70915528230011));
#42321=CARTESIAN_POINT('Ctrl Pts',(-26.9174464342925,-4.13489342958415,
-1.41057836835976));
#42322=CARTESIAN_POINT('Ctrl Pts',(-26.7189732825644,-1.05716051005105,
-4.2390431306241));
#42323=CARTESIAN_POINT('Ctrl Pts',(-26.5205001308362,2.98831621393063,-3.18701132926479));
#42324=CARTESIAN_POINT('Ctrl Pts',(-26.3220269791081,4.29823435975001,0.782468143739444));
#42325=CARTESIAN_POINT('Ctrl Pts',(-26.12355382738,1.67347122286134,4.0356621604834));
#42326=CARTESIAN_POINT('Ctrl Pts',(-25.9250806756518,-2.48321766461065,
3.59453822311966));
#42327=CARTESIAN_POINT('Ctrl Pts',(-25.7266075239237,-4.36672429907916,
-0.13709085722334));
#42328=CARTESIAN_POINT('Ctrl Pts',(-25.5281343721955,-2.25285272466553,
-3.7432244934374));
#42329=CARTESIAN_POINT('Ctrl Pts',(-25.3296612204675,1.92332088042537,-3.92274289218939));
#42330=CARTESIAN_POINT('Ctrl Pts',(-25.1311880687393,4.33885185055037,-0.511311672346996));
#42331=CARTESIAN_POINT('Ctrl Pts',(-24.9327149170112,2.78251955405799,3.36818347757181));
#42332=CARTESIAN_POINT('Ctrl Pts',(-24.734241765283,-1.32098134511574,4.16438270253336));
#42333=CARTESIAN_POINT('Ctrl Pts',(-24.5357686135549,-4.21523208750278,
1.14843086678717));
#42334=CARTESIAN_POINT('Ctrl Pts',(-24.3372954618268,-3.25078332474412,
-2.91881530468582));
#42335=CARTESIAN_POINT('Ctrl Pts',(-24.1388223100987,0.689491144911088,
-4.31412528427163));
#42336=CARTESIAN_POINT('Ctrl Pts',(-23.9403491583705,3.99859298054725,-1.76020714213438));
#42337=CARTESIAN_POINT('Ctrl Pts',(-23.7418760066424,3.64731065820044,2.40503637599935));
#42338=CARTESIAN_POINT('Ctrl Pts',(-23.5434028549143,-0.0427856463317108,
4.36866620329026));
#42339=CARTESIAN_POINT('Ctrl Pts',(-23.3449297031862,-3.69371519826275,
2.33314016754789));
#42340=CARTESIAN_POINT('Ctrl Pts',(-23.146456551458,-3.96335121479337,-1.83818447265194));
#42341=CARTESIAN_POINT('Ctrl Pts',(-22.9479833997299,-0.604864021552577,
-4.32680188161348));
#42342=CARTESIAN_POINT('Ctrl Pts',(-22.7495102480017,3.30732661012167,-2.85458678293089));
#42343=CARTESIAN_POINT('Ctrl Pts',(-22.5510370962736,4.19193079129697,1.23076855999775));
#42344=CARTESIAN_POINT('Ctrl Pts',(-22.3525639445455,1.23916589428106,4.18945615727784));
#42345=CARTESIAN_POINT('Ctrl Pts',(-22.1540907928174,-2.84795381969309,
3.31304000099578));
#42346=CARTESIAN_POINT('Ctrl Pts',(-21.9556176410892,-4.32800522364261,
-0.596192746873735));
#42347=CARTESIAN_POINT('Ctrl Pts',(-21.7571444893611,-1.84612255894362,
-3.95965989760005));
#42348=CARTESIAN_POINT('Ctrl Pts',(-21.558671337633,2.32573400440593,-3.69838293691345));
#42349=CARTESIAN_POINT('Ctrl Pts',(-21.3601981859049,4.36857169866203,-0.0515395086490985));
#42350=CARTESIAN_POINT('Ctrl Pts',(-21.1617250341767,2.41234004112657,3.64248411572105));
#42351=CARTESIAN_POINT('Ctrl Pts',(-20.9632518824486,-1.75219121408373,
4.00211206197311));
#42352=CARTESIAN_POINT('Ctrl Pts',(-20.7647787307204,-4.31273501846039,
0.698134419612753));
#42353=CARTESIAN_POINT('Ctrl Pts',(-20.5663055789923,-2.92532337552109,
-3.24492806637258));
#42354=CARTESIAN_POINT('Ctrl Pts',(-20.3678324272642,1.1399820647682,-4.21752485461668));
#42355=CARTESIAN_POINT('Ctrl Pts',(-20.1693592755361,4.16172735513416,-1.32932329733237));
#42356=CARTESIAN_POINT('Ctrl Pts',(-19.970886123808,3.37375233771011,2.77576479030521));
#42357=CARTESIAN_POINT('Ctrl Pts',(-19.7724129720798,-0.502616439716474,
4.3398677078719));
#42358=CARTESIAN_POINT('Ctrl Pts',(-19.5739398203517,-3.91888105989819,
1.93117742470076));
#42359=CARTESIAN_POINT('Ctrl Pts',(-19.3754666686235,-3.747731252441,-2.24534751581572));
#42360=CARTESIAN_POINT('Ctrl Pts',(-19.1769935168955,-0.145840639017714,
-4.36644082924682));
#42361=CARTESIAN_POINT('Ctrl Pts',(-18.9785203651673,3.58955512665475,-2.49041542719466));
#42362=CARTESIAN_POINT('Ctrl Pts',(-18.7800472134392,4.03900736575815,1.66538118959415));
#42363=CARTESIAN_POINT('Ctrl Pts',(-18.581574061711,0.791079389490325,4.29665781821478));
#42364=CARTESIAN_POINT('Ctrl Pts',(-18.3831009099829,-3.18101693276428,
2.99469635869308));
#42365=CARTESIAN_POINT('Ctrl Pts',(-18.1846277582548,-4.24115296208294,
-1.04866417861854));
#42366=CARTESIAN_POINT('Ctrl Pts',(-17.9861546065267,-1.41886104999451,
-4.1320586065678));
#42367=CARTESIAN_POINT('Ctrl Pts',(-17.7876814547985,2.7022818666961,-3.43289203445551));
#42368=CARTESIAN_POINT('Ctrl Pts',(-17.5892083030704,4.34970720738444,0.40880584307295));
#42369=CARTESIAN_POINT('Ctrl Pts',(-17.3907351513423,2.01533209195444,3.87627547607769));
#42370=CARTESIAN_POINT('Ctrl Pts',(-17.1922619996141,-2.16391438156393,
3.79533260157307));
#42371=CARTESIAN_POINT('Ctrl Pts',(-16.993788847886,-4.36227458832746,0.240073787271785));
#42372=CARTESIAN_POINT('Ctrl Pts',(-16.7953156961578,-2.56732993171374,
-3.53495290336793));
#42373=CARTESIAN_POINT('Ctrl Pts',(-16.5968425444297,1.57779486478368,-4.074019927782));
#42374=CARTESIAN_POINT('Ctrl Pts',(-16.3983693927016,4.27857777509826,-0.88365560584303));
#42375=CARTESIAN_POINT('Ctrl Pts',(-16.1998962409735,3.06267339494391,3.11562300081466));
#42376=CARTESIAN_POINT('Ctrl Pts',(-16.0014230892454,-0.956857468442627,
4.26280409969637));
#42377=CARTESIAN_POINT('Ctrl Pts',(-15.8029499375172,-4.10046374136095,
1.50773741516452));
#42378=CARTESIAN_POINT('Ctrl Pts',(-15.6044767857891,-3.49043152387025,
-2.62753930217525));
#42379=CARTESIAN_POINT('Ctrl Pts',(-15.4060036340609,0.31480468578838,-4.35751913559863));
#42380=CARTESIAN_POINT('Ctrl Pts',(-15.2075304823328,3.83186300629334,-2.09854733287175));
#42381=CARTESIAN_POINT('Ctrl Pts',(-15.0090573306047,3.84116479543024,2.08147256086886));
#42382=CARTESIAN_POINT('Ctrl Pts',(-14.8105841788766,0.334195027597992,
4.35607491795439));
#42383=CARTESIAN_POINT('Ctrl Pts',(-14.6121110271484,-3.47870289812566,
2.64304770177813));
#42384=CARTESIAN_POINT('Ctrl Pts',(-14.4136378754203,-4.10713342729877,
-1.48947306711724));
#42385=CARTESIAN_POINT('Ctrl Pts',(-14.2151647236922,-0.975819915219347,
-4.25850331693705));
#42386=CARTESIAN_POINT('Ctrl Pts',(-14.016691571964,3.04877675323287,-3.12922279747697));
#42387=CARTESIAN_POINT('Ctrl Pts',(-13.8182184202359,4.28246817500175,0.864604728994704));
#42388=CARTESIAN_POINT('Ctrl Pts',(-13.6197452685078,1.59591096403841,4.06695748713514));
#42389=CARTESIAN_POINT('Ctrl Pts',(-13.4212721167797,-2.55157193722059,
3.54634398451292));
#42390=CARTESIAN_POINT('Ctrl Pts',(-13.2227989650515,-4.36329985106452,
-0.220656785535732));
#42391=CARTESIAN_POINT('Ctrl Pts',(-13.0243258133234,-2.18078435752364,
-3.78566435296142));
#42392=CARTESIAN_POINT('Ctrl Pts',(-12.8258526615952,1.99806048313776,-3.88520646980645));
#42393=CARTESIAN_POINT('Ctrl Pts',(-12.6273795098672,4.34784470804019,-0.428160486347726));
#42394=CARTESIAN_POINT('Ctrl Pts',(-12.428906358139,2.71753344232774,3.42083133128965));
#42395=CARTESIAN_POINT('Ctrl Pts',(-12.2304332064109,-1.40045696689287,
4.13833242879109));
#42396=CARTESIAN_POINT('Ctrl Pts',(-12.0319600546827,-4.23644380123351,
1.06752935617385));
#42397=CARTESIAN_POINT('Ctrl Pts',(-11.8334869029546,-3.19431354497235,
-2.98050934971));
#42398=CARTESIAN_POINT('Ctrl Pts',(-11.6350137512265,0.771948962940714,
-4.30013602179249));
#42399=CARTESIAN_POINT('Ctrl Pts',(-11.4365405994984,4.03155546248635,-1.68334059542301));
#42400=CARTESIAN_POINT('Ctrl Pts',(-11.2380674477702,3.60060335336482,2.47441518323838));
#42401=CARTESIAN_POINT('Ctrl Pts',(-11.0395942960421,-0.126406028390937,
4.36704665916097));
#42402=CARTESIAN_POINT('Ctrl Pts',(-10.841121144314,-3.73770105110923,2.26200483196645));
#42403=CARTESIAN_POINT('Ctrl Pts',(-10.6426479925859,-3.92743709512795,
-1.91371703005316));
#42404=CARTESIAN_POINT('Ctrl Pts',(-10.4441748408577,-0.521926362488377,
-4.3375877950126));
#42405=CARTESIAN_POINT('Ctrl Pts',(-10.2457016891296,3.36136517909586,-2.79075243260033));
#42406=CARTESIAN_POINT('Ctrl Pts',(-10.0472285374015,4.16760238916512,1.31078805805055));
#42407=CARTESIAN_POINT('Ctrl Pts',(-9.84875538567332,1.15874117929357,4.212409510804));
#42408=CARTESIAN_POINT('Ctrl Pts',(-9.65028223394519,-2.91085261239433,
3.25791529604742));
#42409=CARTESIAN_POINT('Ctrl Pts',(-9.45180908221706,-4.31579940438351,
-0.678933360813514));
#42410=CARTESIAN_POINT('Ctrl Pts',(-9.25333593048893,-1.76998555489433,
-3.99427416970442));
#42411=CARTESIAN_POINT('Ctrl Pts',(-9.05486277876081,2.39610500605629,-3.65318433797894));
#42412=CARTESIAN_POINT('Ctrl Pts',(-8.85638962703267,4.36875781335193,0.0320963483755011));
#42413=CARTESIAN_POINT('Ctrl Pts',(-8.65791647530455,2.34217089611098,3.68799545833686));
#42414=CARTESIAN_POINT('Ctrl Pts',(-8.45944332357642,-1.82848151744868,
3.9678369860229));
#42415=CARTESIAN_POINT('Ctrl Pts',(-8.26097017184828,-4.32530896002622,
0.615448948020644));
#42416=CARTESIAN_POINT('Ctrl Pts',(-8.06249702012015,-2.86267054231623,
-3.30033216107977));
#42417=CARTESIAN_POINT('Ctrl Pts',(-7.86402386839203,1.22050813883025,-4.19492966452973));
#42418=CARTESIAN_POINT('Ctrl Pts',(-7.66555071666389,4.18641164898603,-1.24941286712486));
#42419=CARTESIAN_POINT('Ctrl Pts',(-7.46707756493577,3.31999840339956,2.83983901105795));
#42420=CARTESIAN_POINT('Ctrl Pts',(-7.26860441320764,-0.585601280879622,
4.32945102144992));
#42421=CARTESIAN_POINT('Ctrl Pts',(-7.07013126147951,-3.95513098708112,
1.85580545379544));
#42422=CARTESIAN_POINT('Ctrl Pts',(-6.87165810975138,-3.7040624282691,-2.3166779091587));
#42423=CARTESIAN_POINT('Ctrl Pts',(-6.67318495802324,-0.0622282930241267,
-4.36843251599986));
#42424=CARTESIAN_POINT('Ctrl Pts',(-6.47471180629512,3.63657074439811,-2.42124518137171));
#42425=CARTESIAN_POINT('Ctrl Pts',(-6.27623865456699,4.00638731049232,1.74239367698454));
#42426=CARTESIAN_POINT('Ctrl Pts',(-6.07776550283886,0.708684648362605,
4.31101392672931));
#42427=CARTESIAN_POINT('Ctrl Pts',(-5.87929235111072,-3.2377607271739,2.93325424759644));
#42428=CARTESIAN_POINT('Ctrl Pts',(-5.68081919938259,-4.22030151652084,
-1.1296592923042));
#42429=CARTESIAN_POINT('Ctrl Pts',(-5.48234604765447,-1.33950215406073,
-4.15846233438502));
#42430=CARTESIAN_POINT('Ctrl Pts',(-5.28387289592634,2.76750164809137,-3.38053392768505));
#42431=CARTESIAN_POINT('Ctrl Pts',(-5.08539974419822,4.34108450918146,0.491996229040367));
#42432=CARTESIAN_POINT('Ctrl Pts',(-4.88692659247008,1.94076028853959,3.91414416059468));
#42433=CARTESIAN_POINT('Ctrl Pts',(-4.68845344074195,-2.23617091758218,
3.75321390834575));
#42434=CARTESIAN_POINT('Ctrl Pts',(-4.48998028901382,-4.36607091699489,
0.156523926563516));
#42435=CARTESIAN_POINT('Ctrl Pts',(-4.29150713728569,-2.49919083141846,
-3.58345087889809));
#42436=CARTESIAN_POINT('Ctrl Pts',(-4.09303398555755,1.65549364400027,-4.04307010156087));
#42437=CARTESIAN_POINT('Ctrl Pts',(-3.89456083382943,4.29470934640759,-0.801589997177687));
#42438=CARTESIAN_POINT('Ctrl Pts',(-3.6960876821013,3.00247066989856,3.17368003394153));
#42439=CARTESIAN_POINT('Ctrl Pts',(-3.49761453037318,-1.03828391133824,
4.2437061383287));
#42440=CARTESIAN_POINT('Ctrl Pts',(-3.29914137864504,-4.12857450997301,
1.42896700762253));
#42441=CARTESIAN_POINT('Ctrl Pts',(-3.10066822691691,-3.4394938140484,-2.693874169598));
#42442=CARTESIAN_POINT('Ctrl Pts',(-2.90219507518879,0.398162150355857,
-4.35069458476621));
#42443=CARTESIAN_POINT('Ctrl Pts',(-2.70372192346066,3.87133219910116,-2.02481019052676));
#42444=CARTESIAN_POINT('Ctrl Pts',(-2.50524877173252,3.80061700796258,2.15462104672691));
#42445=CARTESIAN_POINT('Ctrl Pts',(-2.3067756200044,0.250744414810584,4.36167509654208));
#42446=CARTESIAN_POINT('Ctrl Pts',(-2.10830246827627,-3.52865644924059,
2.57596963970611));
#42447=CARTESIAN_POINT('Ctrl Pts',(-1.90982931654813,-4.07787624219031,
-1.56781834409616));
#42448=CARTESIAN_POINT('Ctrl Pts',(-1.71135616482,-0.894106422019328,-4.27640966953572));
#42449=CARTESIAN_POINT('Ctrl Pts',(-1.51288301309188,3.10809075750666,-3.07027444400813));
#42450=CARTESIAN_POINT('Ctrl Pts',(-1.31440986136373,4.26518845267467,0.946399535345616));
#42451=CARTESIAN_POINT('Ctrl Pts',(-1.11593670963561,1.51765894786496,4.09681002284487));
#42452=CARTESIAN_POINT('Ctrl Pts',(-0.917463557907481,-2.61878668638777,
3.49675893979982));
#42453=CARTESIAN_POINT('Ctrl Pts',(-0.718990406179359,-4.35866736123758,
-0.303967491095578));
#42454=CARTESIAN_POINT('Ctrl Pts',(-0.52051725445122,-2.10716851112986,
-3.82705064996035));
#42455=CARTESIAN_POINT('Ctrl Pts',(-0.322044102723092,2.07063247843363,
-3.84560467727572));
#42456=CARTESIAN_POINT('Ctrl Pts',(-0.123570950994966,4.35802801706137,
-0.346107461111702));
#42457=CARTESIAN_POINT('Ctrl Pts',(0.0749022007331604,2.64588156589855,
3.47487588324251));
#42458=CARTESIAN_POINT('Ctrl Pts',(0.207217635218587,-0.0950992885905953,
3.89410803063403));
#42459=CARTESIAN_POINT('Ctrl Pts',(0.273375352461297,-1.25165011272755,
3.47787809703117));
#42460=CARTESIAN_POINT('Ctrl Pts',(-54.567,-1.74869447533071,3.52286199445108));
#42461=CARTESIAN_POINT('Ctrl Pts',(-54.5008422827573,-2.92020446772555,
2.9413424643865));
#42462=CARTESIAN_POINT('Ctrl Pts',(-54.3685268482719,-4.6172274129017,0.527769072056658));
#42463=CARTESIAN_POINT('Ctrl Pts',(-54.1700536965438,-2.9442570596054,-3.60142813193026));
#42464=CARTESIAN_POINT('Ctrl Pts',(-53.9715805448156,1.42782374076287,-4.42261113343342));
#42465=CARTESIAN_POINT('Ctrl Pts',(-53.7731073930875,4.49085494087165,-1.2008466490418));
#42466=CARTESIAN_POINT('Ctrl Pts',(-53.5746342413593,3.44391503517721,3.12308779992807));
#42467=CARTESIAN_POINT('Ctrl Pts',(-53.3761610896313,-0.756189411504974,
4.58658181113279));
#42468=CARTESIAN_POINT('Ctrl Pts',(-53.1776879379031,-4.26378076653011,
1.85222502157982));
#42469=CARTESIAN_POINT('Ctrl Pts',(-52.979214786175,-3.86837859842421,-2.57810446123634));
#42470=CARTESIAN_POINT('Ctrl Pts',(-52.7807416344468,0.0682846871540122,
-4.64817492172454));
#42471=CARTESIAN_POINT('Ctrl Pts',(-52.5822684827187,3.94239838556798,-2.46333497443955));
#42472=CARTESIAN_POINT('Ctrl Pts',(-52.3837953309906,4.2075906767663,1.97654522392122));
#42473=CARTESIAN_POINT('Ctrl Pts',(-52.1853221792624,0.621067460305235,
4.60702942724974));
#42474=CARTESIAN_POINT('Ctrl Pts',(-51.9868490275344,-3.5339863170476,3.02017189553276));
#42475=CARTESIAN_POINT('Ctrl Pts',(-51.7883758758061,-4.4539682903228,-1.33141391106648));
#42476=CARTESIAN_POINT('Ctrl Pts',(-51.5899027240781,-1.29670574585495,
-4.46419499324869));
#42477=CARTESIAN_POINT('Ctrl Pts',(-51.3914295723499,3.0475838049597,-3.51037373970853));
#42478=CARTESIAN_POINT('Ctrl Pts',(-51.1929564206218,4.60206058888503,0.656908175550339));
#42479=CARTESIAN_POINT('Ctrl Pts',(-50.9944832688937,1.94372785161201,4.22284386453272));
#42480=CARTESIAN_POINT('Ctrl Pts',(-50.7960101171655,-2.49392831173375,
3.92311241991201));
#42481=CARTESIAN_POINT('Ctrl Pts',(-50.5975369654375,-4.64859756442089,
0.032092912022845));
#42482=CARTESIAN_POINT('Ctrl Pts',(-50.3990638137092,-2.54785670310451,
-3.88830493645013));
#42483=CARTESIAN_POINT('Ctrl Pts',(-50.2005906619813,1.8852381363435,-4.24927833946838));
#42484=CARTESIAN_POINT('Ctrl Pts',(-50.0021175102529,4.59255198071539,-0.720385659383156));
#42485=CARTESIAN_POINT('Ctrl Pts',(-49.803644358525,3.09576087736483,3.46796103779234));
#42486=CARTESIAN_POINT('Ctrl Pts',(-49.6051712067967,-1.23494558517625,
4.48167363791002));
#42487=CARTESIAN_POINT('Ctrl Pts',(-49.4066980550687,-4.43516057912403,
1.39278132691336));
#42488=CARTESIAN_POINT('Ctrl Pts',(-49.2082249033404,-3.57534955803026,
-2.97108813779842));
#42489=CARTESIAN_POINT('Ctrl Pts',(-49.0097517516124,0.557400955467083,
-4.61516991703562));
#42490=CARTESIAN_POINT('Ctrl Pts',(-48.8112785998842,4.1798965777469,-2.03444188569328));
#42491=CARTESIAN_POINT('Ctrl Pts',(-48.6128054481562,3.97603945794876,2.40865095344619));
#42492=CARTESIAN_POINT('Ctrl Pts',(-48.414332296428,0.132444081719959,4.64682125247059));
#42493=CARTESIAN_POINT('Ctrl Pts',(-48.2158591446998,-3.83239299652962,
2.63120753782877));
#42494=CARTESIAN_POINT('Ctrl Pts',(-48.0173859929717,-4.28898838077306,
-1.79306102979217));
#42495=CARTESIAN_POINT('Ctrl Pts',(-47.8189128412436,-0.819366418289231,
-4.57592917991651));
#42496=CARTESIAN_POINT('Ctrl Pts',(-47.6204396895155,3.40031834670907,-3.16990919870439));
#42497=CARTESIAN_POINT('Ctrl Pts',(-47.4219665377873,4.50729034775482,1.13790285527143));
#42498=CARTESIAN_POINT('Ctrl Pts',(-47.2234933860592,1.48820744283477,4.40405810521368));
#42499=CARTESIAN_POINT('Ctrl Pts',(-47.025020234331,-2.89320740585849,3.63865910655113));
#42500=CARTESIAN_POINT('Ctrl Pts',(-46.826547082603,-4.62612799527478,-0.457634087822847));
#42501=CARTESIAN_POINT('Ctrl Pts',(-46.6280739308748,-2.12420755208681,
-4.13500078145832));
#42502=CARTESIAN_POINT('Ctrl Pts',(-46.4296007791468,2.32225080975237,-4.02711315505378));
#42503=CARTESIAN_POINT('Ctrl Pts',(-46.2311276274185,4.64287888172855,-0.232733488355147));
#42504=CARTESIAN_POINT('Ctrl Pts',(-46.0326544756905,2.71333185741701,3.77469461261823));
#42505=CARTESIAN_POINT('Ctrl Pts',(-45.8341813239623,-1.7000481037694,4.32669916123979));
#42506=CARTESIAN_POINT('Ctrl Pts',(-45.6357081722342,-4.55717335808265,
0.917965234300663));
#42507=CARTESIAN_POINT('Ctrl Pts',(-45.437235020506,-3.24257989877357,-3.33109063027));
#42508=CARTESIAN_POINT('Ctrl Pts',(-45.238761868778,1.04032970329042,-4.5308060315417));
#42509=CARTESIAN_POINT('Ctrl Pts',(-45.0402887170497,4.37090272508006,-1.5829398456324));
#42510=CARTESIAN_POINT('Ctrl Pts',(-44.8418155653217,3.70027253143814,2.81397803475566));
#42511=CARTESIAN_POINT('Ctrl Pts',(-44.6433424135935,-0.357653898701961,
4.6349296516502));
#42512=CARTESIAN_POINT('Ctrl Pts',(-44.4448692618655,-4.0881774970914,2.21298304089265));
#42513=CARTESIAN_POINT('Ctrl Pts',(-44.2463961101372,-4.07630965474763,
-2.23476817267793));
#42514=CARTESIAN_POINT('Ctrl Pts',(-44.0479229584092,-0.332914408674636,
-4.63677228074658));
#42515=CARTESIAN_POINT('Ctrl Pts',(-43.8494498066809,3.71523669362209,-2.79419138524314));
#42516=CARTESIAN_POINT('Ctrl Pts',(-43.6509766549529,4.36239309537038,1.6062427177945));
#42517=CARTESIAN_POINT('Ctrl Pts',(-43.4525035032247,1.01613615025615,4.53629325674009));
#42518=CARTESIAN_POINT('Ctrl Pts',(-43.2540303514966,-3.26031016017885,
3.3137391035562));
#42519=CARTESIAN_POINT('Ctrl Pts',(-43.0555571997685,-4.55220972667487,
-0.942271612312327));
#42520=CARTESIAN_POINT('Ctrl Pts',(-42.8570840480404,-1.6769343772943,-4.33570989357585));
#42521=CARTESIAN_POINT('Ctrl Pts',(-42.6586108963122,2.73343695672062,-3.76016111232444));
#42522=CARTESIAN_POINT('Ctrl Pts',(-42.4601377445842,4.64157078321707,0.257506992892894));
#42523=CARTESIAN_POINT('Ctrl Pts',(-42.2616645928559,2.30072697040417,4.03944855081209));
#42524=CARTESIAN_POINT('Ctrl Pts',(-42.0631914411279,-2.14624382139399,
4.12360602460166));
#42525=CARTESIAN_POINT('Ctrl Pts',(-41.8647182893996,-4.62850429603346,
0.432940144364989));
#42526=CARTESIAN_POINT('Ctrl Pts',(-41.6662451376716,-2.87374842948024,
-3.65404695523508));
#42527=CARTESIAN_POINT('Ctrl Pts',(-41.4677719859434,1.5116885982894,-4.39605354480638));
#42528=CARTESIAN_POINT('Ctrl Pts',(-41.2692988342153,4.51329860893046,-1.11383340479144));
#42529=CARTESIAN_POINT('Ctrl Pts',(-41.0708256824872,3.38335364292205,3.1880099300236));
#42530=CARTESIAN_POINT('Ctrl Pts',(-40.8723525307591,-0.843774291109008,
4.57149145604215));
#42531=CARTESIAN_POINT('Ctrl Pts',(-40.6738793790309,-4.29849601547731,
1.77014722323563));
#42532=CARTESIAN_POINT('Ctrl Pts',(-40.4754062273028,-3.81829693276388,
-2.65162171514888));
#42533=CARTESIAN_POINT('Ctrl Pts',(-40.2769330755747,0.157240052846411,
-4.64604829428018));
#42534=CARTESIAN_POINT('Ctrl Pts',(-40.0784599238465,3.98883665711766,-2.38739843969065));
#42535=CARTESIAN_POINT('Ctrl Pts',(-39.8799867721184,4.16898021789935,2.05671902061676));
#42536=CARTESIAN_POINT('Ctrl Pts',(-39.6815136203903,0.532764069457865,
4.61807878162528));
#42537=CARTESIAN_POINT('Ctrl Pts',(-39.4830404686622,-3.59115392042467,
2.95196590543005));
#42538=CARTESIAN_POINT('Ctrl Pts',(-39.284567316934,-4.42766481907536,-1.41642982068484));
#42539=CARTESIAN_POINT('Ctrl Pts',(-39.0860941652059,-1.21101145733567,
-4.48820013337248));
#42540=CARTESIAN_POINT('Ctrl Pts',(-38.8876210134777,3.11422364181328,-3.45139106676922));
#42541=CARTESIAN_POINT('Ctrl Pts',(-38.6891478617497,4.58864223166364,0.744883653194257));
#42542=CARTESIAN_POINT('Ctrl Pts',(-38.4906747100215,1.86253493324648,4.25927843765109));
#42543=CARTESIAN_POINT('Ctrl Pts',(-38.2922015582934,-2.56857044737412,
3.87465289334144));
#42544=CARTESIAN_POINT('Ctrl Pts',(-38.0937284065652,-4.64836009769383,
-0.0568998169656816));
#42545=CARTESIAN_POINT('Ctrl Pts',(-37.8952552548371,-2.47295704773775,
-3.93636540822205));
#42546=CARTESIAN_POINT('Ctrl Pts',(-37.696782103109,1.9662355014118,-4.21241108392697));
#42547=CARTESIAN_POINT('Ctrl Pts',(-37.4983089513809,4.60550059726841,-0.63233965205675));
#42548=CARTESIAN_POINT('Ctrl Pts',(-37.2998357996527,3.02880735282022,3.52658690613249));
#42549=CARTESIAN_POINT('Ctrl Pts',(-37.1013626479246,-1.32051078888074,
4.45721218290677));
#42550=CARTESIAN_POINT('Ctrl Pts',(-36.9028894961964,-4.4610095294625,1.30762500933861));
#42551=CARTESIAN_POINT('Ctrl Pts',(-36.7044163444683,-3.51781966015203,
-3.03898569026757));
#42552=CARTESIAN_POINT('Ctrl Pts',(-36.5059431927402,0.64564579542217,-4.60365405888156));
#42553=CARTESIAN_POINT('Ctrl Pts',(-36.3074700410121,4.2180754409679,-1.95405444174575));
#42554=CARTESIAN_POINT('Ctrl Pts',(-36.1089968892839,3.92920272430553,2.48432186689104));
#42555=CARTESIAN_POINT('Ctrl Pts',(-35.9105237375558,0.0434669421797721,
4.64850511583461));
#42556=CARTESIAN_POINT('Ctrl Pts',(-35.7120505858277,-3.88205926305851,
2.55736291227986));
#42557=CARTESIAN_POINT('Ctrl Pts',(-35.5135774340995,-4.25387837783278,
-1.8748354417414));
#42558=CARTESIAN_POINT('Ctrl Pts',(-35.3151042823715,-0.731620476027489,
-4.59077560615418));
#42559=CARTESIAN_POINT('Ctrl Pts',(-35.1166311306433,3.46037600960852,-3.10423695279999));
#42560=CARTESIAN_POINT('Ctrl Pts',(-34.9181579789152,4.48468186310071,1.22397621454777));
#42561=CARTESIAN_POINT('Ctrl Pts',(-34.7196848271871,1.40362902538621,4.431739471821));
#42562=CARTESIAN_POINT('Ctrl Pts',(-34.5212116754589,-2.96233114678408,
3.58260845806457));
#42563=CARTESIAN_POINT('Ctrl Pts',(-34.3227385237308,-4.61651994008701,
-0.546106976499942));
#42564=CARTESIAN_POINT('Ctrl Pts',(-34.1242653720026,-2.04466308785533,
-4.17490623178112));
#42565=CARTESIAN_POINT('Ctrl Pts',(-33.9257922202745,2.39891524530935,-3.98192099781315));
#42566=CARTESIAN_POINT('Ctrl Pts',(-33.7273190685464,4.64648328110378,-0.143813439656987));
#42567=CARTESIAN_POINT('Ctrl Pts',(-33.5288459168183,2.64057668839093,3.82594353587835));
#42568=CARTESIAN_POINT('Ctrl Pts',(-33.3303727650901,-1.7825614468038,4.29336277006403));
#42569=CARTESIAN_POINT('Ctrl Pts',(-33.131899613362,-4.57391067218585,0.830560262634542));
#42570=CARTESIAN_POINT('Ctrl Pts',(-32.9334264616339,-3.17821954463672,
-3.39255209438148));
#42571=CARTESIAN_POINT('Ctrl Pts',(-32.7349533099057,1.12687109628521,-4.51006105494813));
#42572=CARTESIAN_POINT('Ctrl Pts',(-32.5364801581776,4.40040360438443,-1.49897875419349));
#42573=CARTESIAN_POINT('Ctrl Pts',(-32.3380070064495,3.64572725987484,2.88429574309024));
#42574=CARTESIAN_POINT('Ctrl Pts',(-32.1395338547213,-0.446313595424793,
4.62723387798174));
#42575=CARTESIAN_POINT('Ctrl Pts',(-31.9410607029933,-4.12979093297379,
2.13431863528631));
#42576=CARTESIAN_POINT('Ctrl Pts',(-31.7425875512651,-4.03278313978311,
-2.3123903940477));
#42577=CARTESIAN_POINT('Ctrl Pts',(-31.544114399537,-0.244092899977717,
-4.64229553595886));
#42578=CARTESIAN_POINT('Ctrl Pts',(-31.3456412478088,3.76804438445096,-2.72255958682465));
#42579=CARTESIAN_POINT('Ctrl Pts',(-31.1471680960807,4.33084585537712,1.68945652917313));
#42580=CARTESIAN_POINT('Ctrl Pts',(-30.9486949443526,0.92911289211364,4.55491365677892));
#42581=CARTESIAN_POINT('Ctrl Pts',(-30.7502217926244,-3.32314677587213,
3.25072064210593));
#42582=CARTESIAN_POINT('Ctrl Pts',(-30.5517486408963,-4.53333792819974,
-1.02924069864568));
#42583=CARTESIAN_POINT('Ctrl Pts',(-30.3532754891682,-1.59362974946449,
-4.36701653404526));
#42584=CARTESIAN_POINT('Ctrl Pts',(-30.15480233744,2.80491585458726,-3.70714664340217));
#42585=CARTESIAN_POINT('Ctrl Pts',(-29.956329185712,4.63579087837372,0.346312169855375));
#42586=CARTESIAN_POINT('Ctrl Pts',(-29.7578560339838,2.22297929202692,4.08275057457869));
#42587=CARTESIAN_POINT('Ctrl Pts',(-29.5593828822557,-2.22478764577608,
4.08176544135075));
#42588=CARTESIAN_POINT('Ctrl Pts',(-29.3609097305275,-4.63594383247414,
0.344258578902418));
#42589=CARTESIAN_POINT('Ctrl Pts',(-29.1624365787994,-2.80327339209578,
-3.70838879787041));
#42590=CARTESIAN_POINT('Ctrl Pts',(-28.9639634270712,1.59556408874945,-4.36631016141731));
#42591=CARTESIAN_POINT('Ctrl Pts',(-28.7654902753432,4.53379341519692,-1.0272324251697));
#42592=CARTESIAN_POINT('Ctrl Pts',(-28.567017123615,3.32170644956629,3.25219240665626));
#42593=CARTESIAN_POINT('Ctrl Pts',(-28.3685439718869,-0.931130531035452,
4.55450163258032));
#42594=CARTESIAN_POINT('Ctrl Pts',(-28.1700708201587,-4.33159382384316,
1.68753789061073));
#42595=CARTESIAN_POINT('Ctrl Pts',(-27.9715976684306,-3.76683797863228,
-2.72422848339423));
#42596=CARTESIAN_POINT('Ctrl Pts',(-27.7731245167025,0.24614931442832,-4.64218695250519));
#42597=CARTESIAN_POINT('Ctrl Pts',(-27.5746513649744,4.03380708397526,-2.31060372982344));
#42598=CARTESIAN_POINT('Ctrl Pts',(-27.3761782132462,4.12884506991978,2.13614783561486));
#42599=CARTESIAN_POINT('Ctrl Pts',(-27.1777050615181,0.44426378522975,4.62743113143094));
#42600=CARTESIAN_POINT('Ctrl Pts',(-26.9792319097899,-3.64700458397518,
2.88268048029381));
#42601=CARTESIAN_POINT('Ctrl Pts',(-26.7807587580619,-4.39973915686285,
-1.50092789252875));
#42602=CARTESIAN_POINT('Ctrl Pts',(-26.5822856063337,-1.12487312439103,
-4.51055979242331));
#42603=CARTESIAN_POINT('Ctrl Pts',(-26.3838124546056,3.1797220613837,-3.39114387771338));
#42604=CARTESIAN_POINT('Ctrl Pts',(-26.1853393028775,4.57354230284658,0.832586326500559));
#42605=CARTESIAN_POINT('Ctrl Pts',(-25.9868661511493,1.78065940331774,4.29415198571022));
#42606=CARTESIAN_POINT('Ctrl Pts',(-25.7883929994211,-2.64227124109951,
3.82477344106307));
#42607=CARTESIAN_POINT('Ctrl Pts',(-25.5899198476931,-4.64641911891196,
-0.145871719028707));
#42608=CARTESIAN_POINT('Ctrl Pts',(-25.3914466959649,-2.39715110344515,
-3.98298327566846));
#42609=CARTESIAN_POINT('Ctrl Pts',(-25.1929735442368,2.04651228210034,-4.17400007980539));
#42610=CARTESIAN_POINT('Ctrl Pts',(-24.9945003925087,4.61676140093734,-0.544061902560779));
#42611=CARTESIAN_POINT('Ctrl Pts',(-24.7960272407805,2.96074383662082,3.58392035638559));
#42612=CARTESIAN_POINT('Ctrl Pts',(-24.5975540890525,-1.40559205420105,
4.43111725913116));
#42613=CARTESIAN_POINT('Ctrl Pts',(-24.3990809373243,-4.48522361857249,
1.22198947556942));
#42614=CARTESIAN_POINT('Ctrl Pts',(-24.2006077855961,-3.45900055900394,
-3.10576952136075));
#42615=CARTESIAN_POINT('Ctrl Pts',(-24.002134633868,0.733654020408733,-4.59045106338594));
#42616=CARTESIAN_POINT('Ctrl Pts',(-23.8036614821399,4.25470847277443,-1.8729508799497));
#42617=CARTESIAN_POINT('Ctrl Pts',(-23.6051883304118,3.88092602467422,2.55908233122917));
#42618=CARTESIAN_POINT('Ctrl Pts',(-23.4067151786836,-0.0455261270268758,
4.64848540481315));
#42619=CARTESIAN_POINT('Ctrl Pts',(-23.2082420269555,-3.93030284065408,
2.48258106972349));
#42620=CARTESIAN_POINT('Ctrl Pts',(-23.0097688752274,-4.21720942246388,
-1.95592276792438));
#42621=CARTESIAN_POINT('Ctrl Pts',(-22.8112957234993,-0.643606411028971,
-4.60393961457854));
#42622=CARTESIAN_POINT('Ctrl Pts',(-22.6128225717711,3.51916552116573,-3.03742707264574));
#42623=CARTESIAN_POINT('Ctrl Pts',(-22.414349420043,4.46042984164243,1.30960101358717));
#42624=CARTESIAN_POINT('Ctrl Pts',(-22.2158762683148,1.31853620891633,4.45779670384143));
#42625=CARTESIAN_POINT('Ctrl Pts',(-22.0174031165868,-3.03036925880373,
3.52524486274362));
#42626=CARTESIAN_POINT('Ctrl Pts',(-21.8189299648586,-4.60522003235342,
-0.634379729037498));
#42627=CARTESIAN_POINT('Ctrl Pts',(-21.6204568131305,-1.96436929978352,
-4.21328167122386));
#42628=CARTESIAN_POINT('Ctrl Pts',(-21.4219836614024,2.47470053143833,-3.93526955451616));
#42629=CARTESIAN_POINT('Ctrl Pts',(-21.2235105096742,4.64838484703084,-0.0548406865110448));
#42630=CARTESIAN_POINT('Ctrl Pts',(-21.0250373579461,2.56685380635791,3.87579033537536));
#42631=CARTESIAN_POINT('Ctrl Pts',(-20.8265642062179,-1.86442152045769,
4.25845295630437));
#42632=CARTESIAN_POINT('Ctrl Pts',(-20.6280910544898,-4.58897174909836,
0.742850908985189));
#42633=CARTESIAN_POINT('Ctrl Pts',(-20.4296179027617,-3.11269444326658,
-3.45277026311631));
#42634=CARTESIAN_POINT('Ctrl Pts',(-20.2311447510336,1.21299951592391,-4.48766324063775));
#42635=CARTESIAN_POINT('Ctrl Pts',(-20.0326715993054,4.42829183300448,-1.41446832016443));
#42636=CARTESIAN_POINT('Ctrl Pts',(-19.8341984475773,3.5898459098312,2.9535564207699));
#42637=CARTESIAN_POINT('Ctrl Pts',(-19.6357252958492,-0.534809728077204,
4.617842325346));
#42638=CARTESIAN_POINT('Ctrl Pts',(-19.4372521441211,-4.16989089173616,
2.05487204906261));
#42639=CARTESIAN_POINT('Ctrl Pts',(-19.2387789923929,-3.98777869891112,
-2.38916517543554));
#42640=CARTESIAN_POINT('Ctrl Pts',(-19.0403058406648,-0.155181936626634,
-4.64611749243903));
#42641=CARTESIAN_POINT('Ctrl Pts',(-18.8418326889366,3.8194711702762,-2.64993003047852));
#42642=CARTESIAN_POINT('Ctrl Pts',(-18.6433595372085,4.29771145607754,1.77205119206607));
#42643=CARTESIAN_POINT('Ctrl Pts',(-18.4448863854804,0.841749134626984,
4.57186478161348));
#42644=CARTESIAN_POINT('Ctrl Pts',(-18.2464132337522,-3.38476553170436,
3.18651086337221));
#42645=CARTESIAN_POINT('Ctrl Pts',(-18.0479400820241,-4.51280476154808,
-1.11583259100634));
#42646=CARTESIAN_POINT('Ctrl Pts',(-17.849466930296,-1.50974109154628,-4.39672275945386));
#42647=CARTESIAN_POINT('Ctrl Pts',(-17.6509937785679,2.87536681277406,-3.65277358715271));
#42648=CARTESIAN_POINT('Ctrl Pts',(-17.4525206268397,4.62831205861156,0.434990431060229));
#42649=CARTESIAN_POINT('Ctrl Pts',(-17.2540474751116,2.1444169408607,4.12455636047718));
#42650=CARTESIAN_POINT('Ctrl Pts',(-17.0555743233835,-2.30251613464764,
4.03842898126119));
#42651=CARTESIAN_POINT('Ctrl Pts',(-16.8571011716554,-4.64168439794168,
0.255450850277838));
#42652=CARTESIAN_POINT('Ctrl Pts',(-16.6586280199272,-2.73177101695766,
-3.7613715979564));
#42653=CARTESIAN_POINT('Ctrl Pts',(-16.4601548681991,1.67885484022851,-4.33496662183739));
#42654=CARTESIAN_POINT('Ctrl Pts',(-16.261681716471,4.55262668636092,-0.94025498756312));
#42655=CARTESIAN_POINT('Ctrl Pts',(-16.0632085647428,3.25884192419725,3.31518302663628));
#42656=CARTESIAN_POINT('Ctrl Pts',(-15.8647354130147,-1.01814553219758,
4.53584268491193));
#42657=CARTESIAN_POINT('Ctrl Pts',(-15.6662622612865,-4.3631041987887,1.60431011263891));
#42658=CARTESIAN_POINT('Ctrl Pts',(-15.4677891095584,-3.71399856161824,
-2.79583688209824));
#42659=CARTESIAN_POINT('Ctrl Pts',(-15.2693159578303,0.33496836772571,-4.63662435179152));
#42660=CARTESIAN_POINT('Ctrl Pts',(-15.0708428061022,4.07729920967249,-2.23296223474716));
#42661=CARTESIAN_POINT('Ctrl Pts',(-14.872369654374,4.08719679145807,2.21479379963412));
#42662=CARTESIAN_POINT('Ctrl Pts',(-14.6738965026459,0.35560068814135,4.63508762998029));
#42663=CARTESIAN_POINT('Ctrl Pts',(-14.4754233509178,-3.70151870093434,
2.81233861646075));
#42664=CARTESIAN_POINT('Ctrl Pts',(-14.2769501991897,-4.37020108747133,
-1.58487590746636));
#42665=CARTESIAN_POINT('Ctrl Pts',(-14.0784770474615,-1.03832255030294,
-4.53126643098101));
#42666=CARTESIAN_POINT('Ctrl Pts',(-13.8800038957334,3.24405518308156,-3.32965390936127));
#42667=CARTESIAN_POINT('Ctrl Pts',(-13.6815307440053,4.55676627183815,0.919983875315956));
#42668=CARTESIAN_POINT('Ctrl Pts',(-13.4830575922771,1.69813130106531,4.32745182195541));
#42669=CARTESIAN_POINT('Ctrl Pts',(-13.284584440549,-2.71500370080188,3.77349229383538));
#42670=CARTESIAN_POINT('Ctrl Pts',(-13.0861112888209,-4.64277533019594,
-0.234790162330059));
#42671=CARTESIAN_POINT('Ctrl Pts',(-12.8876381370927,-2.32046665624351,
-4.02814146775719));
#42672=CARTESIAN_POINT('Ctrl Pts',(-12.6891649853646,2.12603906125972,-4.13405939688834));
#42673=CARTESIAN_POINT('Ctrl Pts',(-12.4906918336365,4.62633026357041,-0.455584766399773));
#42674=CARTESIAN_POINT('Ctrl Pts',(-12.2922186819084,2.89159527322953,3.63994037902266));
#42675=CARTESIAN_POINT('Ctrl Pts',(-12.0937455301802,-1.49015820109303,
4.40339842879546));
#42676=CARTESIAN_POINT('Ctrl Pts',(-11.8952723784521,-4.50779397233723,
1.13590610966014));
#42677=CARTESIAN_POINT('Ctrl Pts',(-11.696799226724,-3.39891381058531,-3.1714151565532));
#42678=CARTESIAN_POINT('Ctrl Pts',(-11.4983260749959,0.821393377408535,
-4.57556576901178));
#42679=CARTESIAN_POINT('Ctrl Pts',(-11.2998529232677,4.28978224794291,-1.79116092304315));
#42680=CARTESIAN_POINT('Ctrl Pts',(-11.1013797715396,3.83122705141254,2.6329049484415));
#42681=CARTESIAN_POINT('Ctrl Pts',(-10.9029066198114,-0.134502511913974,
4.64676212660943));
#42682=CARTESIAN_POINT('Ctrl Pts',(-10.7044334680833,-3.97710604910729,
2.40688941606321));
#42683=CARTESIAN_POINT('Ctrl Pts',(-10.5059603163552,-4.17899495303025,
-2.03629329163328));
#42684=CARTESIAN_POINT('Ctrl Pts',(-10.3074871646271,-0.55535647850289,
-4.61541638086834));
#42685=CARTESIAN_POINT('Ctrl Pts',(-10.1090140128989,3.57666533632311,-2.96950404258823));
#42686=CARTESIAN_POINT('Ctrl Pts',(-9.91054086117082,4.43454317121036,1.39474587279358));
#42687=CARTESIAN_POINT('Ctrl Pts',(-9.71206770944268,1.23296017806185,4.4822202518748));
#42688=CARTESIAN_POINT('Ctrl Pts',(-9.51359455771455,-3.09729680745274,
3.46658934307858));
#42689=CARTESIAN_POINT('Ctrl Pts',(-9.31512140598642,-4.59223241324053,
-0.722419995422388));
#42690=CARTESIAN_POINT('Ctrl Pts',(-9.11664825425829,-1.88335561377043,
-4.2501130360359));
#42691=CARTESIAN_POINT('Ctrl Pts',(-8.91817510253017,2.54957889450653,-3.88717592188593));
#42692=CARTESIAN_POINT('Ctrl Pts',(-8.71970195080204,4.64858288262784,0.0341521645346766));
#42693=CARTESIAN_POINT('Ctrl Pts',(-8.52122879907389,2.49219022912522,3.92421674335857));
#42694=CARTESIAN_POINT('Ctrl Pts',(-8.32275564734577,-1.94559832482275,
4.22198251363622));
#42695=CARTESIAN_POINT('Ctrl Pts',(-8.12428249561764,-4.60235106926837,
0.654869316892727));
#42696=CARTESIAN_POINT('Ctrl Pts',(-7.92580934388951,-3.04602860816486,
-3.51172306784635));
#42697=CARTESIAN_POINT('Ctrl Pts',(-7.72733619216139,1.29868339804392,-4.46362079691452));
#42698=CARTESIAN_POINT('Ctrl Pts',(-7.52886304043324,4.45455719052072,-1.32943951475187));
#42699=CARTESIAN_POINT('Ctrl Pts',(-7.33038988870513,3.53264896058713,3.02173468528678));
#42700=CARTESIAN_POINT('Ctrl Pts',(-7.131916736977,-0.623109864781879,4.60675843553939));
#42701=CARTESIAN_POINT('Ctrl Pts',(-6.93344358524887,-4.2084626776301,1.97467239764006));
#42702=CARTESIAN_POINT('Ctrl Pts',(-6.73497043352073,-3.94131282526402,
-2.46506438058074));
#42703=CARTESIAN_POINT('Ctrl Pts',(-6.5364972817926,-0.066214102526462,
-4.64823674952382));
#42704=CARTESIAN_POINT('Ctrl Pts',(-6.33802413006447,3.86949820432006,-2.57632933333366));
#42705=CARTESIAN_POINT('Ctrl Pts',(-6.13955097833635,4.26300204049134,1.85399643735695));
#42706=CARTESIAN_POINT('Ctrl Pts',(-5.94107782660821,0.754076894693181,
4.58714041902643));
#42707=CARTESIAN_POINT('Ctrl Pts',(-5.74260467488009,-3.44514384578296,
3.12113329882894));
#42708=CARTESIAN_POINT('Ctrl Pts',(-5.54413152315195,-4.49061775163378,
-1.20201555539611));
#42709=CARTESIAN_POINT('Ctrl Pts',(-5.34565837142384,-1.42529914695175,
-4.42481768309406));
#42710=CARTESIAN_POINT('Ctrl Pts',(-5.14718521969569,2.94476401270036,-3.59706187016166));
#42711=CARTESIAN_POINT('Ctrl Pts',(-4.94871206796758,4.61913706448716,0.523509278002365));
#42712=CARTESIAN_POINT('Ctrl Pts',(-4.75023891623944,2.06506870877937,4.16485058738426));
#42713=CARTESIAN_POINT('Ctrl Pts',(-4.55176576451131,-2.37940080320625,
3.9936125266212));
#42714=CARTESIAN_POINT('Ctrl Pts',(-4.35329261278318,-4.64572388678821,
0.1665495037332));
#42715=CARTESIAN_POINT('Ctrl Pts',(-4.15481946105504,-2.65926751165869,
-3.81297593688373));
#42716=CARTESIAN_POINT('Ctrl Pts',(-3.95634630932691,1.76153033530024,-4.30203441581027));
#42717=CARTESIAN_POINT('Ctrl Pts',(-3.75787315759879,4.56979150745246,-0.852932961487828));
#42718=CARTESIAN_POINT('Ctrl Pts',(-3.55940000587066,3.19478313012126,3.37695869421504));
#42719=CARTESIAN_POINT('Ctrl Pts',(-3.36092685414253,-1.10478745303856,
4.51552147231563));
#42720=CARTESIAN_POINT('Ctrl Pts',(-3.16245370241439,-4.39301550158241,
1.52049434994359));
#42721=CARTESIAN_POINT('Ctrl Pts',(-2.96398055068627,-3.6597982199938,-2.86642059087705));
#42722=CARTESIAN_POINT('Ctrl Pts',(-2.76550739895815,0.423664994886726,
-4.62936267890035));
#42723=CARTESIAN_POINT('Ctrl Pts',(-2.56703424723001,4.11929645967266,-2.15450212494862));
#42724=CARTESIAN_POINT('Ctrl Pts',(-2.36856109550188,4.04405186129635,2.29262754867159));
#42725=CARTESIAN_POINT('Ctrl Pts',(-2.17008794377375,0.266804946486184,
4.64104650786609));
#42726=CARTESIAN_POINT('Ctrl Pts',(-1.97161479204563,-3.75467184710545,
2.74096411037234));
#42727=CARTESIAN_POINT('Ctrl Pts',(-1.77314164031749,-4.33906993859569,
-1.66823930938942));
#42728=CARTESIAN_POINT('Ctrl Pts',(-1.57466848858935,-0.951375193182703,
-4.55031971059427));
#42729=CARTESIAN_POINT('Ctrl Pts',(-1.37619533686123,3.30716833257329,-3.26692983112172));
#42730=CARTESIAN_POINT('Ctrl Pts',(-1.17772218513309,4.5383797590448,1.00701775380853));
#42731=CARTESIAN_POINT('Ctrl Pts',(-0.979249033404966,1.6148671334332,4.35921645447386));
#42732=CARTESIAN_POINT('Ctrl Pts',(-0.780775881676836,-2.78652364898572,
3.72073125741831));
#42733=CARTESIAN_POINT('Ctrl Pts',(-0.582302729948716,-4.63784612289411,
-0.323437035503383));
#42734=CARTESIAN_POINT('Ctrl Pts',(-0.383829578220575,-2.24213561157208,
-4.07217861516247));
#42735=CARTESIAN_POINT('Ctrl Pts',(-0.185356426492449,2.20325939470542,
-4.0919210539669));
#42736=CARTESIAN_POINT('Ctrl Pts',(0.0131167252356776,4.63716582782614,
-0.368276129740102));
#42737=CARTESIAN_POINT('Ctrl Pts',(0.211589876963804,2.81535399355526,3.69744656037688));
#42738=CARTESIAN_POINT('Ctrl Pts',(0.343905311449231,-0.101190531491979,
4.14353111517988));
#42739=CARTESIAN_POINT('Ctrl Pts',(0.41006302869194,-1.3318200590755,3.70064107017205));
#42740=CARTESIAN_POINT('',(0.,3.89175630324288,-0.568086152066163));
#42741=CARTESIAN_POINT('Ctrl Pts',(1.36557432028894E-14,3.8984675804681,
-0.567744983796988));
#42742=CARTESIAN_POINT('Ctrl Pts',(1.22189337746952E-14,3.90378079301249,
-0.48168157494731));
#42743=CARTESIAN_POINT('Ctrl Pts',(1.81248313162765E-15,3.90605201893254,
-0.395549047494557));
#42744=CARTESIAN_POINT('Ctrl Pts',(2.1094237467878E-15,3.9051901940657,
-0.30946516814072));
#42745=CARTESIAN_POINT('Ctrl Pts',(2.53269562981551E-15,3.90397348654204,
-0.187933627678834));
#42746=CARTESIAN_POINT('Ctrl Pts',(-1.73372847453606E-15,3.89651412242738,
-0.0664981433266434));
#42747=CARTESIAN_POINT('Ctrl Pts',(-3.44169137633799E-15,3.88304410532436,
0.0544558887272117));
#42748=CARTESIAN_POINT('Ctrl Pts',(-4.42827767156581E-15,3.87526329564968,
0.124323676985952));
#42749=CARTESIAN_POINT('Ctrl Pts',(-5.99827845040638E-15,3.86547596069021,
0.194030594989938));
#42750=CARTESIAN_POINT('Ctrl Pts',(-8.54871728961371E-15,3.85371957233101,
0.263499450080404));
#42751=CARTESIAN_POINT('Ctrl Pts',(-1.02912501597371E-14,3.84568727105213,
0.310962561755177));
#42752=CARTESIAN_POINT('Ctrl Pts',(9.54271907070366E-15,3.83673570538044,
0.358314497435108));
#42753=CARTESIAN_POINT('Ctrl Pts',(1.0769163338864E-14,3.82687555339248,
0.405529836552379));
#42754=CARTESIAN_POINT('Ctrl Pts',(1.14030656965669E-14,3.82177921615585,
0.429933648093749));
#42755=CARTESIAN_POINT('Ctrl Pts',(3.36346654511152E-15,3.81643949818047,
0.454303276137411));
#42756=CARTESIAN_POINT('Ctrl Pts',(3.77475828372553E-15,3.81086326754485,
0.478612579049032));
#42757=CARTESIAN_POINT('Ctrl Pts',(5.8076671888918E-15,3.78330139879781,
0.598767188849739));
#42758=CARTESIAN_POINT('Ctrl Pts',(-8.81286749205166E-15,3.74994210044639,
0.717568668278516));
#42759=CARTESIAN_POINT('Ctrl Pts',(-6.66133814775094E-15,3.71102535385896,
0.834613822750009));
#42760=CARTESIAN_POINT('Ctrl Pts',(-4.77874997148781E-15,3.67697320059496,
0.937028332912565));
#42761=CARTESIAN_POINT('Ctrl Pts',(-1.19256951314485E-14,3.63866504086141,
1.03809826459941));
#42762=CARTESIAN_POINT('Ctrl Pts',(-1.80411241501588E-14,3.59623186452301,
1.13753521681003));
#42763=CARTESIAN_POINT('Ctrl Pts',(-2.07166243458445E-14,3.57766734987495,
1.18103888340217));
#42764=CARTESIAN_POINT('Ctrl Pts',(7.25282410556592E-15,3.55831295269719,
1.22422972408107));
#42765=CARTESIAN_POINT('Ctrl Pts',(6.38378239159465E-15,3.53817820767951,
1.26708221387324));
#42766=CARTESIAN_POINT('Ctrl Pts',(5.86343967720961E-15,3.52612243669922,
1.29274033879192));
#42767=CARTESIAN_POINT('Ctrl Pts',(-1.21504972407371E-14,3.5137868896413,
1.31827714523396));
#42768=CARTESIAN_POINT('Ctrl Pts',(-1.25455201782643E-14,3.50117347886088,
1.34368698778094));
#42769=CARTESIAN_POINT('Ctrl Pts',(-1.28529383185491E-14,3.49135736208285,
1.36346165349941));
#42770=CARTESIAN_POINT('Ctrl Pts',(-1.07293940314999E-15,3.48137159065754,
1.38316187499542));
#42771=CARTESIAN_POINT('Ctrl Pts',(-1.49880108324396E-15,3.47122829643433,
1.40276372527097));
#42772=CARTESIAN_POINT('Ctrl Pts',(-3.7927871000821E-15,3.41658948716747,
1.50835286967661));
#42773=CARTESIAN_POINT('Ctrl Pts',(-1.78861038778567E-14,3.3573208681292,
1.61121938665418));
#42774=CARTESIAN_POINT('Ctrl Pts',(-1.51545442861334E-14,3.29363279258605,
1.71100480040831));
#42775=CARTESIAN_POINT('Ctrl Pts',(-1.24429888430173E-14,3.23041112668357,
1.81005945132219));
#42776=CARTESIAN_POINT('Ctrl Pts',(-5.91093669341422E-15,3.16283391779207,
1.90607864354505));
#42777=CARTESIAN_POINT('Ctrl Pts',(7.21644966006352E-16,3.09106889768542,
1.99867770501885));
#42778=CARTESIAN_POINT('Ctrl Pts',(7.15828444958648E-15,3.02142398629525,
2.08854117083508));
#42779=CARTESIAN_POINT('Ctrl Pts',(-1.113421031979E-15,2.94783444879763,
2.17518402768862));
#42780=CARTESIAN_POINT('Ctrl Pts',(-2.692290834716E-15,2.87042640391083,
2.25821467895789));
#42781=CARTESIAN_POINT('Ctrl Pts',(-3.75588572577925E-15,2.81828100159452,
2.31414771177578));
#42782=CARTESIAN_POINT('Ctrl Pts',(1.06053239849839E-14,2.76440223430484,
2.36844071851178));
#42783=CARTESIAN_POINT('Ctrl Pts',(1.08246744900953E-14,2.70882332088636,
2.42096180237772));
#42784=CARTESIAN_POINT('Ctrl Pts',(1.09325239104711E-14,2.68149649255625,
2.44678516872728));
#42785=CARTESIAN_POINT('Ctrl Pts',(-3.0607682060388E-15,2.65375860355061,
2.47218002031012));
#42786=CARTESIAN_POINT('Ctrl Pts',(-4.05231403988182E-15,2.62561329981337,
2.49712970045525));
#42787=CARTESIAN_POINT('Ctrl Pts',(-4.49139428739187E-15,2.61314988510334,
2.50817801648817));
#42788=CARTESIAN_POINT('Ctrl Pts',(9.44721820786953E-15,2.60061273947681,
2.51913353665884));
#42789=CARTESIAN_POINT('Ctrl Pts',(9.07607322631065E-15,2.58800583701869,
2.5299921641494));
#42790=CARTESIAN_POINT('Ctrl Pts',(6.58226895225797E-15,2.50329730317145,
2.60295365626651));
#42791=CARTESIAN_POINT('Ctrl Pts',(-5.44922795401061E-15,2.41539203436312,
2.67158814314046));
#42792=CARTESIAN_POINT('Ctrl Pts',(-3.88578058618805E-15,2.3244377116327,
2.7355533676673));
#42793=CARTESIAN_POINT('Ctrl Pts',(-3.00127507940947E-15,2.27298116696346,
2.77174108623125));
#42794=CARTESIAN_POINT('Ctrl Pts',(1.68198853175566E-14,2.22054821616337,
2.80643359943742));
#42795=CARTESIAN_POINT('Ctrl Pts',(1.35724764760425E-14,2.16716210631343,
2.83956236070516));
#42796=CARTESIAN_POINT('Ctrl Pts',(7.66563464323506E-15,2.07094770881052,
2.89926822454041));
#42797=CARTESIAN_POINT('Ctrl Pts',(8.40867004919118E-15,1.97163780542389,
2.95389782223386));
#42798=CARTESIAN_POINT('Ctrl Pts',(9.63118473862323E-15,1.8696483294102,
3.00342377340144));
#42799=CARTESIAN_POINT('Ctrl Pts',(1.08588687776138E-14,1.76722759538598,
3.05315914287378));
#42800=CARTESIAN_POINT('Ctrl Pts',(-1.80644630904049E-15,1.66210361371026,
3.09774762574349));
#42801=CARTESIAN_POINT('Ctrl Pts',(-5.4678483962789E-15,1.55469419618438,
3.13710949192373));
#42802=CARTESIAN_POINT('Ctrl Pts',(-6.61135484369508E-15,1.52114875142644,
3.14940274644399));
#42803=CARTESIAN_POINT('Ctrl Pts',(9.392172699074E-15,1.4873804182791,3.16118581633617));
#42804=CARTESIAN_POINT('Ctrl Pts',(8.85402862138562E-15,1.45340208653369,
3.17245523646713));
#42805=CARTESIAN_POINT('Ctrl Pts',(8.61943655830772E-15,1.43858998086425,
3.17736789206964));
#42806=CARTESIAN_POINT('Ctrl Pts',(-3.17134925512025E-15,1.42373964752971,
3.182182318915));
#42807=CARTESIAN_POINT('Ctrl Pts',(-3.02535774210355E-15,1.40886346011089,
3.18689486353806));
#42808=CARTESIAN_POINT('Ctrl Pts',(-1.98365783949599E-15,1.30271672140575,
3.22052049816183));
#42809=CARTESIAN_POINT('Ctrl Pts',(3.26982359098091E-15,1.19509672053443,
3.24901613967402));
#42810=CARTESIAN_POINT('Ctrl Pts',(5.10702591327572E-15,1.0864059213934,
3.27238984682911));
#42811=CARTESIAN_POINT('Ctrl Pts',(6.94588490287831E-15,0.977617112092361,
3.29578463084439));
#42812=CARTESIAN_POINT('Ctrl Pts',(1.14510993419572E-14,0.867754622283836,
3.31404818378446));
#42813=CARTESIAN_POINT('Ctrl Pts',(8.67361737988404E-15,0.757218921225994,
3.32713646231221));
#42814=CARTESIAN_POINT('Ctrl Pts',(5.93036099161788E-15,0.648045298426994,
3.34006346028121));
#42815=CARTESIAN_POINT('Ctrl Pts',(2.18853355113062E-14,0.538214089575848,
3.34794178778571));
#42816=CARTESIAN_POINT('Ctrl Pts',(2.32869279415127E-14,0.428121599625193,
3.35067992093372));
#42817=CARTESIAN_POINT('Ctrl Pts',(2.41195983244399E-14,0.362716882969348,
3.35230661520498));
#42818=CARTESIAN_POINT('Ctrl Pts',(-8.15105557746918E-15,0.297220211304994,
3.35211819703499));
#42819=CARTESIAN_POINT('Ctrl Pts',(-8.50708392619026E-15,0.231718325657212,
3.35008743341715));
#42820=CARTESIAN_POINT('Ctrl Pts',(-8.62454349224495E-15,0.21010818396038,
3.34941745133801));
#42821=CARTESIAN_POINT('Ctrl Pts',(9.54989894362464E-15,0.188497502383238,
3.34854689142872));
#42822=CARTESIAN_POINT('Ctrl Pts',(1.00336405850499E-14,0.166889483364383,
3.34747463388988));
#42823=CARTESIAN_POINT('Ctrl Pts',(1.05189742785417E-14,0.145210349749661,
3.3463988474222));
#42824=CARTESIAN_POINT('Ctrl Pts',(-2.12730678030541E-16,0.123528723474772,
3.34511958286768));
#42825=CARTESIAN_POINT('Ctrl Pts',(3.05311331771918E-16,0.101878773581793,
3.34363804214106));
#42826=CARTESIAN_POINT('Ctrl Pts',(2.87320079637429E-15,-0.00543815668135161,
3.33629417281912));
#42827=CARTESIAN_POINT('Ctrl Pts',(-8.51767506189532E-15,-0.112104853391998,
3.32398025711894));
#42828=CARTESIAN_POINT('Ctrl Pts',(-4.6074255521944E-15,-0.217758135893045,
3.306659700895));
#42829=CARTESIAN_POINT('Ctrl Pts',(-7.51373278920776E-16,-0.321947032063546,
3.2895792127993));
#42830=CARTESIAN_POINT('Ctrl Pts',(1.11424313353336E-14,-0.425151170945409,
3.26762971614554));
#42831=CARTESIAN_POINT('Ctrl Pts',(8.67361737988404E-15,-0.527005212035941,
3.24072940055987));
#42832=CARTESIAN_POINT('Ctrl Pts',(6.28095158031733E-15,-0.625717664680271,
3.21465879894271));
#42833=CARTESIAN_POINT('Ctrl Pts',(4.47067010218622E-15,-0.723162567288633,
3.18393779064207));
#42834=CARTESIAN_POINT('Ctrl Pts',(5.68295410730002E-15,-0.818981858554579,
3.14845138915928));
#42835=CARTESIAN_POINT('Ctrl Pts',(6.85203894076324E-15,-0.911386674340049,
3.11422952894112));
#42836=CARTESIAN_POINT('Ctrl Pts',(8.30932818362312E-15,-1.00228004599708,
3.07557558113778));
#42837=CARTESIAN_POINT('Ctrl Pts',(8.88178419700125E-15,-1.09131022003164,
3.0323521507494));
#42838=CARTESIAN_POINT('Ctrl Pts',(-0.596163522034944,-3.93875600852084,
-0.00157175874070594));
#42839=CARTESIAN_POINT('Ctrl Pts',(-0.591543258006201,-3.93922783435017,
-0.0925476617549403));
#42840=CARTESIAN_POINT('Ctrl Pts',(-0.586922993977456,-3.93634370691034,
-0.183493527674194));
#42841=CARTESIAN_POINT('Ctrl Pts',(-0.582302729948712,-3.93000729202238,
-0.274199249959615));
#42842=CARTESIAN_POINT('Ctrl Pts',(-0.516145012706005,-3.83927595245344,
-1.57301756205636));
#42843=CARTESIAN_POINT('Ctrl Pts',(-0.449987295463298,-3.04070578201288,
-2.82259808860928));
#42844=CARTESIAN_POINT('Ctrl Pts',(-0.383829578220589,-1.9005215290797,
-3.45067875835325));
#42845=CARTESIAN_POINT('Ctrl Pts',(-0.317671860977876,-0.760337276146452,
-4.07875942809726));
#42846=CARTESIAN_POINT('Ctrl Pts',(-0.251514143735159,0.72146105927955,
-4.08534024103211));
#42847=CARTESIAN_POINT('Ctrl Pts',(-0.185356426492449,1.86801129917929,
-3.46802316012836));
#42848=CARTESIAN_POINT('Ctrl Pts',(-0.12357095099497,2.93878814436674,-2.89150342870496));
#42849=CARTESIAN_POINT('Ctrl Pts',(-0.0617854754974978,3.71716450840878,
-1.77082536565068));
#42850=CARTESIAN_POINT('Ctrl Pts',(-2.03309591384482E-14,3.898467580468,
-0.567744983797649));
#42851=CARTESIAN_POINT('',(-54.567,-1.8715865317393,-2.62360084935039));
#42852=CARTESIAN_POINT('Ctrl Pts',(-54.567,-1.87559511676541,-2.6273759996692));
#42853=CARTESIAN_POINT('Ctrl Pts',(-54.567,-1.93789333947134,-2.59269552998053));
#42854=CARTESIAN_POINT('Ctrl Pts',(-54.567,-1.99885539889533,-2.55586353911646));
#42855=CARTESIAN_POINT('Ctrl Pts',(-54.567,-2.05835614585776,-2.51690310931682));
#42856=CARTESIAN_POINT('Ctrl Pts',(-54.567,-2.14425612316253,-2.46065675601161));
#42857=CARTESIAN_POINT('Ctrl Pts',(-54.567,-2.22711174078161,-2.39997677567503));
#42858=CARTESIAN_POINT('Ctrl Pts',(-54.567,-2.30683028545471,-2.33525511370045));
#42859=CARTESIAN_POINT('Ctrl Pts',(-54.567,-2.35703865932115,-2.29449208403147));
#42860=CARTESIAN_POINT('Ctrl Pts',(-54.567,-2.40600232074533,-2.25212477113805));
#42861=CARTESIAN_POINT('Ctrl Pts',(-54.567,-2.45369396016998,-2.20824155898267));
#42862=CARTESIAN_POINT('Ctrl Pts',(-54.567,-2.48399487183792,-2.18036033386087));
#42863=CARTESIAN_POINT('Ctrl Pts',(-54.567,-2.51378223757325,-2.15186704269938));
#42864=CARTESIAN_POINT('Ctrl Pts',(-54.567,-2.54304824257815,-2.12278299439938));
#42865=CARTESIAN_POINT('Ctrl Pts',(-54.567,-2.55735314842029,-2.10856702702118));
#42866=CARTESIAN_POINT('Ctrl Pts',(-54.567,-2.57152812272356,-2.09421517294112));
#42867=CARTESIAN_POINT('Ctrl Pts',(-54.567,-2.58556785894575,-2.07973508475119));
#42868=CARTESIAN_POINT('Ctrl Pts',(-54.567,-2.65948482112199,-2.00349974000504));
#42869=CARTESIAN_POINT('Ctrl Pts',(-54.567,-2.72969587957797,-1.92367319141114));
#42870=CARTESIAN_POINT('Ctrl Pts',(-54.567,-2.79610010548891,-1.84066258236708));
#42871=CARTESIAN_POINT('Ctrl Pts',(-54.567,-2.85914867889807,-1.76184680812596));
#42872=CARTESIAN_POINT('Ctrl Pts',(-54.567,-2.91876562057248,-1.68015980669411));
#42873=CARTESIAN_POINT('Ctrl Pts',(-54.567,-2.9748433696887,-1.59591432401766));
#42874=CARTESIAN_POINT('Ctrl Pts',(-54.567,-2.99960770630907,-1.55871091402662));
#42875=CARTESIAN_POINT('Ctrl Pts',(-54.567,-3.02368153939547,-1.52100814673485));
#42876=CARTESIAN_POINT('Ctrl Pts',(-54.567,-3.04705405758258,-1.48283118015269));
#42877=CARTESIAN_POINT('Ctrl Pts',(-54.567,-3.05696360798717,-1.4666447952877));
#42878=CARTESIAN_POINT('Ctrl Pts',(-54.567,-3.06674707634774,-1.45037315554266));
#42879=CARTESIAN_POINT('Ctrl Pts',(-54.567,-3.07640358148389,-1.43401812748205));
#42880=CARTESIAN_POINT('Ctrl Pts',(-54.567,-3.08610983773139,-1.41757883696721));
#42881=CARTESIAN_POINT('Ctrl Pts',(-54.567,-3.09568363424083,-1.40106231376754));
#42882=CARTESIAN_POINT('Ctrl Pts',(-54.567,-3.10512111622586,-1.38447657626704));
#42883=CARTESIAN_POINT('Ctrl Pts',(-54.567,-3.16019365145779,-1.28769031333241));
#42884=CARTESIAN_POINT('Ctrl Pts',(-54.567,-3.21066290690797,-1.18848927937393));
#42885=CARTESIAN_POINT('Ctrl Pts',(-54.567,-3.25641980079756,-1.08730183953019));
#42886=CARTESIAN_POINT('Ctrl Pts',(-54.567,-3.30287797646003,-0.98456357529316));
#42887=CARTESIAN_POINT('Ctrl Pts',(-54.567,-3.34447882586322,-0.87977687522081));
#42888=CARTESIAN_POINT('Ctrl Pts',(-54.567,-3.38107398738024,-0.773348853617018));
#42889=CARTESIAN_POINT('Ctrl Pts',(-54.567,-3.41755338310152,-0.667257508341412));
#42890=CARTESIAN_POINT('Ctrl Pts',(-54.567,-3.44905921083244,-0.559534393146257));
#42891=CARTESIAN_POINT('Ctrl Pts',(-54.567,-3.47540277351408,-0.450553507956699));
#42892=CARTESIAN_POINT('Ctrl Pts',(-54.567,-3.49233717958551,-0.380497434443491));
#42893=CARTESIAN_POINT('Ctrl Pts',(-54.567,-3.50713752571676,-0.309921054712288));
#42894=CARTESIAN_POINT('Ctrl Pts',(-54.567,-3.51974304811656,-0.238919698740827));
#42895=CARTESIAN_POINT('Ctrl Pts',(-54.567,-3.52344450058597,-0.218071047169208));
#42896=CARTESIAN_POINT('Ctrl Pts',(-54.567,-3.52695665008924,-0.197185738634729));
#42897=CARTESIAN_POINT('Ctrl Pts',(-54.567,-3.53027780775631,-0.176266156451971));
#42898=CARTESIAN_POINT('Ctrl Pts',(-54.567,-3.53256308803807,-0.16187144428919));
#42899=CARTESIAN_POINT('Ctrl Pts',(-54.567,-3.53475742989087,-0.147463468338002));
#42900=CARTESIAN_POINT('Ctrl Pts',(-54.567,-3.53685927013624,-0.133051340231281));
#42901=CARTESIAN_POINT('Ctrl Pts',(-54.567,-3.55357701763763,-0.018419260473514));
#42902=CARTESIAN_POINT('Ctrl Pts',(-54.567,-3.56447071696453,0.0966256754745031));
#42903=CARTESIAN_POINT('Ctrl Pts',(-54.567,-3.56939469418434,0.211658829454915));
#42904=CARTESIAN_POINT('Ctrl Pts',(-54.567,-3.5721437137338,0.275880976514499));
#42905=CARTESIAN_POINT('Ctrl Pts',(-54.567,-3.57303128839785,0.340100030441642));
#42906=CARTESIAN_POINT('Ctrl Pts',(-54.567,-3.57202588112357,0.404245521614954));
#42907=CARTESIAN_POINT('Ctrl Pts',(-54.567,-3.57028656986049,0.515214457416961));
#42908=CARTESIAN_POINT('Ctrl Pts',(-54.567,-3.56288525045421,0.625962966574239));
#42909=CARTESIAN_POINT('Ctrl Pts',(-54.567,-3.55008625998367,0.73620625076776));
#42910=CARTESIAN_POINT('Ctrl Pts',(-54.567,-3.53704492605657,0.848536944793815));
#42911=CARTESIAN_POINT('Ctrl Pts',(-54.567,-3.51839948040439,0.960343777988608));
#42912=CARTESIAN_POINT('Ctrl Pts',(-54.567,-3.49437547908036,1.07132868702773));
#42913=CARTESIAN_POINT('Ctrl Pts',(-54.567,-3.48660681757375,1.10721797037555));
#42914=CARTESIAN_POINT('Ctrl Pts',(-54.567,-3.47827531871655,1.14302128727563));
#42915=CARTESIAN_POINT('Ctrl Pts',(-54.567,-3.46938746150371,1.17872844162552));
#42916=CARTESIAN_POINT('Ctrl Pts',(-54.567,-3.4641078129644,1.19993954130812));
#42917=CARTESIAN_POINT('Ctrl Pts',(-54.567,-3.45863056337528,1.22112107217551));
#42918=CARTESIAN_POINT('Ctrl Pts',(-54.567,-3.45296480785638,1.24224278150716));
#42919=CARTESIAN_POINT('Ctrl Pts',(-54.567,-3.42342725283962,1.35235760191379));
#42920=CARTESIAN_POINT('Ctrl Pts',(-54.567,-3.38873905323224,1.46098133704825));
#42921=CARTESIAN_POINT('Ctrl Pts',(-54.567,-3.34920122580605,1.56782019179735));
#42922=CARTESIAN_POINT('Ctrl Pts',(-54.567,-3.30839441336409,1.67808808943033));
#42923=CARTESIAN_POINT('Ctrl Pts',(-54.567,-3.26242164280839,1.78645539462761));
#42924=CARTESIAN_POINT('Ctrl Pts',(-54.567,-3.21155853814977,1.89260246649006));
#42925=CARTESIAN_POINT('Ctrl Pts',(-54.567,-3.16022236311832,1.99973679690069));
#42926=CARTESIAN_POINT('Ctrl Pts',(-54.567,-3.10390419869295,2.1046102041018));
#42927=CARTESIAN_POINT('Ctrl Pts',(-54.567,-3.04283453234895,2.20688591053918));
#42928=CARTESIAN_POINT('Ctrl Pts',(-54.567,-3.00304595452076,2.27352136393423));
#42929=CARTESIAN_POINT('Ctrl Pts',(-54.567,-2.96123934929021,2.33905393291921));
#42930=CARTESIAN_POINT('Ctrl Pts',(-54.567,-2.91746739595464,2.40338613119922));
#42931=CARTESIAN_POINT('Ctrl Pts',(-54.567,-2.902844530786,2.42487754270281));
#42932=CARTESIAN_POINT('Ctrl Pts',(-54.567,-2.88800225968487,2.44623495342649));
#42933=CARTESIAN_POINT('Ctrl Pts',(-54.567,-2.87294234438241,2.4674546085744));
#42934=CARTESIAN_POINT('Ctrl Pts',(-54.567,-2.86355986312814,2.48067467074929));
#42935=CARTESIAN_POINT('Ctrl Pts',(-54.567,-2.8540929031093,2.49384126294727));
#42936=CARTESIAN_POINT('Ctrl Pts',(-54.567,-2.84454187121597,2.50695346356968));
#42937=CARTESIAN_POINT('Ctrl Pts',(-54.567,-2.8345065952103,2.52073046209268));
#42938=CARTESIAN_POINT('Ctrl Pts',(-54.567,-2.82438385780302,2.53444004293616));
#42939=CARTESIAN_POINT('Ctrl Pts',(-54.567,-2.81417640991632,2.54807871818807));
#42940=CARTESIAN_POINT('Ctrl Pts',(-54.567,-2.74073890385789,2.64620219700058));
#42941=CARTESIAN_POINT('Ctrl Pts',(-54.567,-2.66288925851384,2.74069993823569));
#42942=CARTESIAN_POINT('Ctrl Pts',(-54.567,-2.58091654790888,2.83123710890433));
#42943=CARTESIAN_POINT('Ctrl Pts',(-54.567,-2.49880880908221,2.92192341546302));
#42944=CARTESIAN_POINT('Ctrl Pts',(-54.567,-2.41256402764738,3.00863692299536));
#42945=CARTESIAN_POINT('Ctrl Pts',(-54.567,-2.32242287699813,3.09102490393745));
#42946=CARTESIAN_POINT('Ctrl Pts',(-54.567,-2.2339914908075,3.17185017971528));
#42947=CARTESIAN_POINT('Ctrl Pts',(-54.567,-2.14180963977267,3.24851316729089));
#42948=CARTESIAN_POINT('Ctrl Pts',(-54.567,-2.04606345312307,3.32065397851649));
#42949=CARTESIAN_POINT('Ctrl Pts',(-54.567,-1.95044552606602,3.3926981514176));
#42950=CARTESIAN_POINT('Ctrl Pts',(-54.567,-1.85127243673682,3.46023303947618));
#42951=CARTESIAN_POINT('Ctrl Pts',(-54.567,-1.74869447533108,3.5228619944509));
#42952=CARTESIAN_POINT('Ctrl Pts',(-54.567,-1.87559511676549,-2.62737599966915));
#42953=CARTESIAN_POINT('Ctrl Pts',(-54.5052145245025,-1.06132064244425,
-3.20258678468392));
#42954=CARTESIAN_POINT('Ctrl Pts',(-54.3772713317624,1.2252681129847,-3.56578698204833));
#42955=CARTESIAN_POINT('Ctrl Pts',(-54.1831704217794,3.67986340215961,-0.983988949453548));
#42956=CARTESIAN_POINT('Ctrl Pts',(-53.9846972700513,2.8219875869866,2.55909768807962));
#42957=CARTESIAN_POINT('Ctrl Pts',(-53.7862241183231,-0.619631178725218,
3.75830321175399));
#42958=CARTESIAN_POINT('Ctrl Pts',(-53.6267338785483,-2.92926965772152,
1.95781535064456));
#42959=CARTESIAN_POINT('Ctrl Pts',(-53.5334013560163,-3.22000259141683,
0.443210257437656));
#42960=CARTESIAN_POINT('Ctrl Pts',(-53.5062265507269,-3.21814301605221,
0.00152842760642868));
#42961=CARTESIAN_POINT('Origin',(-54.567,-5.160062080289E-16,2.1385152528819E-16));
#42962=CARTESIAN_POINT('',(-54.567,-3.933,-4.81653586104654E-16));
#42963=CARTESIAN_POINT('Origin',(-54.567,0.,0.));
#42964=CARTESIAN_POINT('Origin',(-54.567,0.,0.));
#42965=CARTESIAN_POINT('',(-54.567,1.87158653173894,-2.62360084935064));
#42966=CARTESIAN_POINT('Ctrl Pts',(-54.567,1.75279620618125,3.52818484004951));
#42967=CARTESIAN_POINT('Ctrl Pts',(-54.567,1.82657430789191,3.48355378460627));
#42968=CARTESIAN_POINT('Ctrl Pts',(-54.567,1.89867731497302,3.43638255044532));
#42969=CARTESIAN_POINT('Ctrl Pts',(-54.567,1.96895656450102,3.38666332265823));
#42970=CARTESIAN_POINT('Ctrl Pts',(-54.567,2.06817543877299,3.31647068622802));
#42971=CARTESIAN_POINT('Ctrl Pts',(-54.567,2.16376116540805,3.24120063054011));
#42972=CARTESIAN_POINT('Ctrl Pts',(-54.567,2.25552899767464,3.16126330551513));
#42973=CARTESIAN_POINT('Ctrl Pts',(-54.567,2.30853769233681,3.11508837526235));
#42974=CARTESIAN_POINT('Ctrl Pts',(-54.567,2.36027174475663,3.06735546330207));
#42975=CARTESIAN_POINT('Ctrl Pts',(-54.567,2.41068902882149,3.01813932376916));
#42976=CARTESIAN_POINT('Ctrl Pts',(-54.567,2.44513556400026,2.98451344500101));
#42977=CARTESIAN_POINT('Ctrl Pts',(-54.567,2.47896732919389,2.95019513230726));
#42978=CARTESIAN_POINT('Ctrl Pts',(-54.567,2.51216950552106,2.91520763695931));
#42979=CARTESIAN_POINT('Ctrl Pts',(-54.567,2.5293304452325,2.89712393387901));
#42980=CARTESIAN_POINT('Ctrl Pts',(-54.567,2.54632471679035,2.87885960856721));
#42981=CARTESIAN_POINT('Ctrl Pts',(-54.567,2.56313473931103,2.86043519067462));
#42982=CARTESIAN_POINT('Ctrl Pts',(-54.567,2.64622234210827,2.76936804821556));
#42983=CARTESIAN_POINT('Ctrl Pts',(-54.567,2.72489683748954,2.67430520513737));
#42984=CARTESIAN_POINT('Ctrl Pts',(-54.567,2.79896338868084,2.57567350309106));
#42985=CARTESIAN_POINT('Ctrl Pts',(-54.567,2.86377162097323,2.48937076380055));
#42986=CARTESIAN_POINT('Ctrl Pts',(-54.567,2.92505136680962,2.40033466336044));
#42987=CARTESIAN_POINT('Ctrl Pts',(-54.567,2.98264010850768,2.30883708534923));
#42988=CARTESIAN_POINT('Ctrl Pts',(-54.567,3.00783518300059,2.26880689496932));
#42989=CARTESIAN_POINT('Ctrl Pts',(-54.567,3.03232337259389,2.22830544226294));
#42990=CARTESIAN_POINT('Ctrl Pts',(-54.567,3.05608912160428,2.187355097956));
#42991=CARTESIAN_POINT('Ctrl Pts',(-54.567,3.07031897932052,2.16283588029263));
#42992=CARTESIAN_POINT('Ctrl Pts',(-54.567,3.08428981350088,2.13815572847739));
#42993=CARTESIAN_POINT('Ctrl Pts',(-54.567,3.09799807180379,2.1133194287978));
#42994=CARTESIAN_POINT('Ctrl Pts',(-54.567,3.108666220358,2.09399112839202));
#42995=CARTESIAN_POINT('Ctrl Pts',(-54.567,3.1191765774848,2.07456573812209));
#42996=CARTESIAN_POINT('Ctrl Pts',(-54.567,3.12951637983522,2.05506685410723));
#42997=CARTESIAN_POINT('Ctrl Pts',(-54.567,3.18521374551435,1.95003230542785));
#42998=CARTESIAN_POINT('Ctrl Pts',(-54.567,3.23603690595946,1.84274166201074));
#42999=CARTESIAN_POINT('Ctrl Pts',(-54.567,3.2818109194263,1.7335719482421));
#43000=CARTESIAN_POINT('Ctrl Pts',(-54.567,3.3272497182131,1.62520171190402));
#43001=CARTESIAN_POINT('Ctrl Pts',(-54.567,3.36771328199207,1.51497896136699));
#43002=CARTESIAN_POINT('Ctrl Pts',(-54.567,3.40298086689944,1.4032605963081));
#43003=CARTESIAN_POINT('Ctrl Pts',(-54.567,3.43720657024157,1.29484263600781));
#43004=CARTESIAN_POINT('Ctrl Pts',(-54.567,3.46653877479758,1.18501538926984));
#43005=CARTESIAN_POINT('Ctrl Pts',(-54.567,3.49072735193707,1.0741054881589));
#43006=CARTESIAN_POINT('Ctrl Pts',(-54.567,3.50702181451284,0.999391823832429));
#43007=CARTESIAN_POINT('Ctrl Pts',(-54.567,3.5209811379261,0.924186878286872));
#43008=CARTESIAN_POINT('Ctrl Pts',(-54.567,3.53251580228219,0.848593054092502));
#43009=CARTESIAN_POINT('Ctrl Pts',(-54.567,3.53818712754629,0.811425334969612));
#43010=CARTESIAN_POINT('Ctrl Pts',(-54.567,3.54327213639131,0.774163649634371));
#43011=CARTESIAN_POINT('Ctrl Pts',(-54.567,3.54775921107122,0.736820478666499));
#43012=CARTESIAN_POINT('Ctrl Pts',(-54.567,3.54974618674968,0.720284098560792));
#43013=CARTESIAN_POINT('Ctrl Pts',(-54.567,3.55161489769857,0.703739936148487));
#43014=CARTESIAN_POINT('Ctrl Pts',(-54.567,3.55336423854053,0.687193590734354));
#43015=CARTESIAN_POINT('Ctrl Pts',(-54.567,3.56511848569491,0.576014666173494));
#43016=CARTESIAN_POINT('Ctrl Pts',(-54.567,3.57149546524957,0.464671209704678));
#43017=CARTESIAN_POINT('Ctrl Pts',(-54.567,3.57229788708192,0.353479489050023));
#43018=CARTESIAN_POINT('Ctrl Pts',(-54.567,3.57275184924506,0.290573880059895));
#43019=CARTESIAN_POINT('Ctrl Pts',(-54.567,3.57142069612182,0.227716836591344));
#43020=CARTESIAN_POINT('Ctrl Pts',(-54.567,3.56826131091937,0.164966495916737));
#43021=CARTESIAN_POINT('Ctrl Pts',(-54.567,3.56256734722735,0.051875454917302));
#43022=CARTESIAN_POINT('Ctrl Pts',(-54.567,3.55093778082866,-0.0608703175100407));
#43023=CARTESIAN_POINT('Ctrl Pts',(-54.567,3.53358690749236,-0.172913290391381));
#43024=CARTESIAN_POINT('Ctrl Pts',(-54.567,3.51616267006857,-0.28543001063441));
#43025=CARTESIAN_POINT('Ctrl Pts',(-54.567,3.49296810100612,-0.397238776827455));
#43026=CARTESIAN_POINT('Ctrl Pts',(-54.567,3.46417552856231,-0.507950709219032));
#43027=CARTESIAN_POINT('Ctrl Pts',(-54.567,3.45518320814962,-0.54252758391528));
#43028=CARTESIAN_POINT('Ctrl Pts',(-54.567,3.44564456424833,-0.576997229641806));
#43029=CARTESIAN_POINT('Ctrl Pts',(-54.567,3.4355640867651,-0.611347076759574));
#43030=CARTESIAN_POINT('Ctrl Pts',(-54.567,3.43116972567637,-0.626321132485534));
#43031=CARTESIAN_POINT('Ctrl Pts',(-54.567,3.42667284595602,-0.6412706901372));
#43032=CARTESIAN_POINT('Ctrl Pts',(-54.567,3.42207748879482,-0.656183497321861));
#43033=CARTESIAN_POINT('Ctrl Pts',(-54.567,3.38928802295434,-0.762591544534128));
#43034=CARTESIAN_POINT('Ctrl Pts',(-54.567,3.35144238687093,-0.867290076268274));
#43035=CARTESIAN_POINT('Ctrl Pts',(-54.567,3.30877634235103,-0.96995281167844));
#43036=CARTESIAN_POINT('Ctrl Pts',(-54.567,3.26607183263496,-1.07270810177234));
#43037=CARTESIAN_POINT('Ctrl Pts',(-54.567,3.21853763250597,-1.17342467286773));
#43038=CARTESIAN_POINT('Ctrl Pts',(-54.567,3.16636553468308,-1.2717482204815));
#43039=CARTESIAN_POINT('Ctrl Pts',(-54.567,3.11483633831456,-1.36886015586578));
#43040=CARTESIAN_POINT('Ctrl Pts',(-54.567,3.05878222358417,-1.4636383033807));
#43041=CARTESIAN_POINT('Ctrl Pts',(-54.567,2.99835357830501,-1.5557047498662));
#43042=CARTESIAN_POINT('Ctrl Pts',(-54.567,2.96245358513743,-1.61040041256928));
#43043=CARTESIAN_POINT('Ctrl Pts',(-54.567,2.92500902671214,-1.66413826114627));
#43044=CARTESIAN_POINT('Ctrl Pts',(-54.567,2.88604689933135,-1.71683148033191));
#43045=CARTESIAN_POINT('Ctrl Pts',(-54.567,2.87319267374389,-1.73421581152415));
#43046=CARTESIAN_POINT('Ctrl Pts',(-54.567,2.86017324527383,-1.75148639042203));
#43047=CARTESIAN_POINT('Ctrl Pts',(-54.567,2.84698951658492,-1.76863994674457));
#43048=CARTESIAN_POINT('Ctrl Pts',(-54.567,2.83376235824213,-1.78585001007142));
#43049=CARTESIAN_POINT('Ctrl Pts',(-54.567,2.820366499874,-1.80294627458048));
#43050=CARTESIAN_POINT('Ctrl Pts',(-54.567,2.80682238333785,-1.81990133392153));
#43051=CARTESIAN_POINT('Ctrl Pts',(-54.567,2.7396855052284,-1.90394592621961));
#43052=CARTESIAN_POINT('Ctrl Pts',(-54.567,2.66883293323538,-1.98462632727596));
#43053=CARTESIAN_POINT('Ctrl Pts',(-54.567,2.59444135432091,-2.06162312908462));
#43054=CARTESIAN_POINT('Ctrl Pts',(-54.567,2.52108087456256,-2.13755272223168));
#43055=CARTESIAN_POINT('Ctrl Pts',(-54.567,2.44427822116883,-2.20990063504143));
#43056=CARTESIAN_POINT('Ctrl Pts',(-54.567,2.36417413831495,-2.27831994080785));
#43057=CARTESIAN_POINT('Ctrl Pts',(-54.567,2.28654079774992,-2.34462891129411));
#43058=CARTESIAN_POINT('Ctrl Pts',(-54.567,2.2058060012744,-2.40724817445458));
#43059=CARTESIAN_POINT('Ctrl Pts',(-54.567,2.1220790745464,-2.46581789968667));
#43060=CARTESIAN_POINT('Ctrl Pts',(-54.567,2.04133558314445,-2.52230061427447));
#43061=CARTESIAN_POINT('Ctrl Pts',(-54.567,1.95780896462242,-2.57501739905895));
#43062=CARTESIAN_POINT('Ctrl Pts',(-54.567,1.87158653173864,-2.62360084935085));
#43063=CARTESIAN_POINT('Origin',(-54.567,0.,0.));
#43064=CARTESIAN_POINT('Origin',(-56.8777734492732,0.,0.));
#43065=CARTESIAN_POINT('Ctrl Pts',(-54.567,1.87158653173864,-2.62360084935085));
#43066=CARTESIAN_POINT('Ctrl Pts',(-54.5008422827573,2.74405176481089,-2.00121418560501));
#43067=CARTESIAN_POINT('Ctrl Pts',(-54.3685268482719,3.80418105204897,0.171604520928937));
#43068=CARTESIAN_POINT('Ctrl Pts',(-54.1700536965438,1.91525344717721,3.29560071974874));
#43069=CARTESIAN_POINT('Ctrl Pts',(-53.9715805448156,-1.72862424686986,
3.39318099076701));
#43070=CARTESIAN_POINT('Ctrl Pts',(-53.8324871290587,-3.17271035699792,
1.28805258441639));
#43071=CARTESIAN_POINT('Ctrl Pts',(-53.7595514305446,-3.22738947633959,
0.111495431728052));
#43072=CARTESIAN_POINT('Ctrl Pts',(-53.7527734492731,-3.22663436289375,
0.00208142861643813));
#43073=CARTESIAN_POINT('Ctrl Pts',(-54.9770630286919,2.2840585926085,-3.20180657528391));
#43074=CARTESIAN_POINT('Ctrl Pts',(-54.9109053114492,3.34880322426559,-2.44225440756606));
#43075=CARTESIAN_POINT('Ctrl Pts',(-54.7785898769639,4.64257049963806,0.209423809111752));
#43076=CARTESIAN_POINT('Ctrl Pts',(-54.5801167252356,2.33734909867248,4.02190602149484));
#43077=CARTESIAN_POINT('Ctrl Pts',(-54.3816435735076,-2.1095893764457,4.14099164896006));
#43078=CARTESIAN_POINT('Ctrl Pts',(-54.1831704217793,-4.62428608899499,
0.475171829894237));
#43079=CARTESIAN_POINT('Ctrl Pts',(-53.9846972700514,-2.90639616515588,
-3.6286483864793));
#43080=CARTESIAN_POINT('Ctrl Pts',(-53.7862241183231,1.47235844481099,-4.40916304885659));
#43081=CARTESIAN_POINT('Ctrl Pts',(-53.5877509665951,4.5031341736765,-1.15427358412515));
#43082=CARTESIAN_POINT('Ctrl Pts',(-53.3892778148669,3.41174088157173,3.15768914610369));
#43083=CARTESIAN_POINT('Ctrl Pts',(-53.1908046631387,-0.80286404893351,
4.57882123411569));
#43084=CARTESIAN_POINT('Ctrl Pts',(-52.9923315114107,-4.28249053334774,
1.80853540431148));
#43085=CARTESIAN_POINT('Ctrl Pts',(-52.7938583596825,-3.8418595301935,-2.61737787780216));
#43086=CARTESIAN_POINT('Ctrl Pts',(-52.5953852079544,0.115685074092492,
-4.64726406566888));
#43087=CARTESIAN_POINT('Ctrl Pts',(-52.3969120562262,3.96732629995167,-2.42297769608721));
#43088=CARTESIAN_POINT('Ctrl Pts',(-52.1984389044981,4.18720711106116,2.01935496417796));
#43089=CARTESIAN_POINT('Ctrl Pts',(-51.99996575277,0.574042118338133,4.61312905987137));
#43090=CARTESIAN_POINT('Ctrl Pts',(-51.8014926010419,-3.56461093282257,
2.98396398628069));
#43091=CARTESIAN_POINT('Ctrl Pts',(-51.6030194493137,-4.44015505970837,
-1.37677681431043));
#43092=CARTESIAN_POINT('Ctrl Pts',(-51.4045462975856,-1.25110101055297,
-4.47719062196251));
#43093=CARTESIAN_POINT('Ctrl Pts',(-51.2060731458575,3.08323341148789,-3.47910369919806));
#43094=CARTESIAN_POINT('Ctrl Pts',(-51.0075999941293,4.59512037410658,0.703817700242058));
#43095=CARTESIAN_POINT('Ctrl Pts',(-50.8091268424013,1.90055122225936,4.24245158453203));
#43096=CARTESIAN_POINT('Ctrl Pts',(-50.610653690673,-2.53381679938504,3.89746879408851));
#43097=CARTESIAN_POINT('Ctrl Pts',(-50.412180538945,-4.64868321197714,-0.0153272752145113));
#43098=CARTESIAN_POINT('Ctrl Pts',(-50.2137073872168,-2.50806113711531,
-3.91409246682743));
#43099=CARTESIAN_POINT('Ctrl Pts',(-50.0152342354887,1.92848535238818,-4.22982680231204));
#43100=CARTESIAN_POINT('Ctrl Pts',(-49.8167610837606,4.59966155680488,-0.673501363724546));
#43101=CARTESIAN_POINT('Ctrl Pts',(-49.6182879320324,3.06022458354438,3.49935937277421));
#43102=CARTESIAN_POINT('Ctrl Pts',(-49.4198147803042,-1.28059718662182,
4.46884340414282));
#43103=CARTESIAN_POINT('Ctrl Pts',(-49.2213416285762,-4.44913718740654,
1.34746755487186));
#43104=CARTESIAN_POINT('Ctrl Pts',(-49.022868476848,-3.54485673436904,-3.007404405193));
#43105=CARTESIAN_POINT('Ctrl Pts',(-48.8243953251199,0.604449530452811,
-4.60924411256357));
#43106=CARTESIAN_POINT('Ctrl Pts',(-48.6259221733918,4.20043178948642,-1.99169859811178));
#43107=CARTESIAN_POINT('Ctrl Pts',(-48.4274490216636,3.9512630032017,2.44908374772434));
#43108=CARTESIAN_POINT('Ctrl Pts',(-48.2289758699355,0.0850367741389765,
4.64793064394765));
#43109=CARTESIAN_POINT('Ctrl Pts',(-48.0305027182074,-3.85903365222682,
2.59197796959199));
#43110=CARTESIAN_POINT('Ctrl Pts',(-47.8320295664792,-4.27047504771653,
-1.83671810322143));
#43111=CARTESIAN_POINT('Ctrl Pts',(-47.6335564147511,-0.772646535574469,
-4.58404928583278));
#43112=CARTESIAN_POINT('Ctrl Pts',(-47.435083263023,3.43247655551004,-3.13505904565577));
#43113=CARTESIAN_POINT('Ctrl Pts',(-47.2366101112949,4.49544867810111,1.18382080841386));
#43114=CARTESIAN_POINT('Ctrl Pts',(-47.0381369595668,1.44320597277678,4.41900973567803));
#43115=CARTESIAN_POINT('Ctrl Pts',(-46.8396638078386,-2.93017351870171,
3.60895742205062));
#43116=CARTESIAN_POINT('Ctrl Pts',(-46.6411906561104,-4.62121930425517,
-0.504799629412044));
#43117=CARTESIAN_POINT('Ctrl Pts',(-46.4427175043824,-2.08191756152741,
-4.15645399239292));
#43118=CARTESIAN_POINT('Ctrl Pts',(-46.2442443526542,2.36320907948709,-4.00321537898037));
#43119=CARTESIAN_POINT('Ctrl Pts',(-46.0457712009261,4.64501149154437,-0.185361180660728));
#43120=CARTESIAN_POINT('Ctrl Pts',(-45.847298049198,2.67468657781142,3.8021759867674));
#43121=CARTESIAN_POINT('Ctrl Pts',(-45.6488248974699,-1.74409468659784,
4.30913265612192));
#43122=CARTESIAN_POINT('Ctrl Pts',(-45.4503517457417,-4.56630020751363,
0.871431545639821));
#43123=CARTESIAN_POINT('Ctrl Pts',(-45.2518785940136,-3.20843213216912,
-3.36399372430151));
#43124=CARTESIAN_POINT('Ctrl Pts',(-45.0534054422854,1.08649260427824,-4.5199584450218));
#43125=CARTESIAN_POINT('Ctrl Pts',(-44.8549322905574,4.38682240800469,-1.5382716549762));
#43126=CARTESIAN_POINT('Ctrl Pts',(-44.6564591388291,3.67137583132355,2.85157676190709));
#43127=CARTESIAN_POINT('Ctrl Pts',(-44.4579859871011,-0.404914421209559,
4.63104036209702));
#43128=CARTESIAN_POINT('Ctrl Pts',(-44.2595128353729,-4.11053870700268,
2.17116606046336));
#43129=CARTESIAN_POINT('Ctrl Pts',(-44.0610396836449,-4.0533016970634,-2.27623282562621));
#43130=CARTESIAN_POINT('Ctrl Pts',(-43.8625665319166,-0.285599182974214,
-4.63992711478959));
#43131=CARTESIAN_POINT('Ctrl Pts',(-43.6640933801886,3.74354597605967,-2.75614840837764));
#43132=CARTESIAN_POINT('Ctrl Pts',(-43.4656202284604,4.34578160663879,1.65065827816515));
#43133=CARTESIAN_POINT('Ctrl Pts',(-43.2671470767323,0.969810346848859,
4.54642259529622));
#43134=CARTESIAN_POINT('Ctrl Pts',(-43.0686739250041,-3.29394280200141,
3.28030964102757));
#43135=CARTESIAN_POINT('Ctrl Pts',(-42.8702007732761,-4.54236127977997,
-0.988657942784552));
#43136=CARTESIAN_POINT('Ctrl Pts',(-42.6717276215479,-1.63262028765758,
-4.35259020816388));
#43137=CARTESIAN_POINT('Ctrl Pts',(-42.4732544698198,2.77165077192005,-3.73208286649562));
#43138=CARTESIAN_POINT('Ctrl Pts',(-42.2747813180916,4.63870270808269,0.304840466312254));
#43139=CARTESIAN_POINT('Ctrl Pts',(-42.0763081663635,2.25940249266056,4.06270733625183));
#43140=CARTESIAN_POINT('Ctrl Pts',(-41.8778350146354,-2.18819552923403,
4.10149861022962));
#43141=CARTESIAN_POINT('Ctrl Pts',(-41.6793618629072,-4.63267988371023,
0.38570405616468));
#43142=CARTESIAN_POINT('Ctrl Pts',(-41.4808887111792,-2.83632548869743,
-3.68317094988007));
#43143=CARTESIAN_POINT('Ctrl Pts',(-41.2824155594509,1.55645243234538,-4.38040481573579));
#43144=CARTESIAN_POINT('Ctrl Pts',(-41.0839424077229,4.52442571492474,-1.06773708093468));
#43145=CARTESIAN_POINT('Ctrl Pts',(-40.8854692559947,3.3506580672695,3.22235644212695));
#43146=CARTESIAN_POINT('Ctrl Pts',(-40.6869961042666,-0.890362428554528,
4.56264673952452));
#43147=CARTESIAN_POINT('Ctrl Pts',(-40.4885229525385,-4.31632909314358,
1.72620789117576));
#43148=CARTESIAN_POINT('Ctrl Pts',(-40.2900498008103,-3.79105022960651,
-2.69043280541915));
#43149=CARTESIAN_POINT('Ctrl Pts',(-40.0915766490822,0.204624413165435,
-4.64420277048838));
#43150=CARTESIAN_POINT('Ctrl Pts',(-39.8931034973541,4.01298217624216,-2.34658572761319));
#43151=CARTESIAN_POINT('Ctrl Pts',(-39.6946303456259,4.14778365198342,2.09913822799128));
#43152=CARTESIAN_POINT('Ctrl Pts',(-39.4961571938978,0.485629137374503,
4.62327317652853));
#43153=CARTESIAN_POINT('Ctrl Pts',(-39.2976840421697,-3.62107905142639,
2.91518044504901));
#43154=CARTESIAN_POINT('Ctrl Pts',(-39.0992108904416,-4.41298614415993,
-1.46152106222511));
#43155=CARTESIAN_POINT('Ctrl Pts',(-38.9007377387134,-1.16516610035691,
-4.50031982001882));
#43156=CARTESIAN_POINT('Ctrl Pts',(-38.7022645869853,3.14926801392388,-3.41944461869924));
#43157=CARTESIAN_POINT('Ctrl Pts',(-38.5037914352572,4.58080536839695,0.791651881031651));
#43158=CARTESIAN_POINT('Ctrl Pts',(-38.305318283529,1.81899084063146,4.27805596568979));
#43159=CARTESIAN_POINT('Ctrl Pts',(-38.106845131801,-2.60796072132454,3.84825043362611));
#43160=CARTESIAN_POINT('Ctrl Pts',(-37.9083719800727,-4.64753798551651,
-0.104312976452023));
#43161=CARTESIAN_POINT('Ctrl Pts',(-37.7098988283447,-2.43267512575256,
-3.9613864058458));
#43162=CARTESIAN_POINT('Ctrl Pts',(-37.5114256766164,2.00910243504338,-4.19213524702842));
#43163=CARTESIAN_POINT('Ctrl Pts',(-37.3129525248885,4.61171137808434,-0.585327847554368));
#43164=CARTESIAN_POINT('Ctrl Pts',(-37.1144793731602,2.99267652000514,3.55729922419876));
#43165=CARTESIAN_POINT('Ctrl Pts',(-36.9160062214322,-1.36590841908661,
4.44351040445992));
#43166=CARTESIAN_POINT('Ctrl Pts',(-36.7175330697039,-4.47411614729356,
1.26205198957974));
#43167=CARTESIAN_POINT('Ctrl Pts',(-36.5190599179759,-3.48663723117299,
-3.07471158681162));
#43168=CARTESIAN_POINT('Ctrl Pts',(-36.3205867662477,0.692572313122873,
-4.59682870193908));
#43169=CARTESIAN_POINT('Ctrl Pts',(-36.1221136145196,4.23778866642741,-1.91092588620662));
#43170=CARTESIAN_POINT('Ctrl Pts',(-35.9236404627915,3.90365681526734,2.52427296315037));
#43171=CARTESIAN_POINT('Ctrl Pts',(-35.7251673110634,-0.00395291531700801,
4.64870679849092));
#43172=CARTESIAN_POINT('Ctrl Pts',(-35.5266941593352,-3.90794407590074,
2.51763055739075));
#43173=CARTESIAN_POINT('Ctrl Pts',(-35.3282210076071,-4.23453272132453,
-1.91813011964965));
#43174=CARTESIAN_POINT('Ctrl Pts',(-35.129747855879,-0.684753713175434,
-4.59799987779117));
#43175=CARTESIAN_POINT('Ctrl Pts',(-34.9312747041509,3.49186119850797,-3.06877758956716));
#43176=CARTESIAN_POINT('Ctrl Pts',(-34.7328015524227,4.4719633680656,1.26965907178053));
#43177=CARTESIAN_POINT('Ctrl Pts',(-34.5343284006946,1.35834958624193,4.44582691132163));
#43178=CARTESIAN_POINT('Ctrl Pts',(-34.3358552489664,-2.99872191450223,
3.55220458354517));
#43179=CARTESIAN_POINT('Ctrl Pts',(-34.1373820972383,-4.61070927103869,
-0.593169909750221));
#43180=CARTESIAN_POINT('Ctrl Pts',(-33.9389089455102,-2.00197017332486,
-4.19554596554403));
#43181=CARTESIAN_POINT('Ctrl Pts',(-33.7404357937821,2.43940854108479,-3.95724354741501));
#43182=CARTESIAN_POINT('Ctrl Pts',(-33.5419626420539,4.64770866458143,-0.0964089884288398));
#43183=CARTESIAN_POINT('Ctrl Pts',(-33.3434894903258,2.60141242142668,3.85268009799961));
#43184=CARTESIAN_POINT('Ctrl Pts',(-33.1450163385977,-1.82626368761961,
4.27495631172498));
#43185=CARTESIAN_POINT('Ctrl Pts',(-32.9465431868696,-4.58214506712391,
0.783860387892622));
#43186=CARTESIAN_POINT('Ctrl Pts',(-32.7480700351414,-3.14344818000384,
-3.42479547761697));
#43187=CARTESIAN_POINT('Ctrl Pts',(-32.5495968834133,1.17281788595065,-4.4983317719205));
#43188=CARTESIAN_POINT('Ctrl Pts',(-32.3511237316851,4.41546529883954,-1.45401400220878));
#43189=CARTESIAN_POINT('Ctrl Pts',(-32.1526505799571,3.61611611226858,2.92133441880021));
#43190=CARTESIAN_POINT('Ctrl Pts',(-31.9541774282288,-0.49349100632212,
4.62244060541122));
#43191=CARTESIAN_POINT('Ctrl Pts',(-31.7557042765008,-4.15134755404042,
2.09208126262768));
#43192=CARTESIAN_POINT('Ctrl Pts',(-31.5572311247726,-4.00898565116478,
-2.35340701380574));
#43193=CARTESIAN_POINT('Ctrl Pts',(-31.3587579730445,-0.196725952115783,
-4.64454404905792));
#43194=CARTESIAN_POINT('Ctrl Pts',(-31.1602848213164,3.79562023287763,-2.68398166380569));
#43195=CARTESIAN_POINT('Ctrl Pts',(-30.9618116695882,4.31338717518866,1.7335459615462));
#43196=CARTESIAN_POINT('Ctrl Pts',(-30.7633385178601,0.88260167414833,4.56415433663957));
#43197=CARTESIAN_POINT('Ctrl Pts',(-30.564865366132,-3.3561333235221,3.2166534843871));
#43198=CARTESIAN_POINT('Ctrl Pts',(-30.3663922144039,-4.52260332466425,
-1.07543000312019));
#43199=CARTESIAN_POINT('Ctrl Pts',(-30.1679190626757,-1.54900064449623,
-4.38304546260082));
#43200=CARTESIAN_POINT('Ctrl Pts',(-29.9694459109476,2.8425851730912,-3.6783420256411));
#43201=CARTESIAN_POINT('Ctrl Pts',(-29.7709727592195,4.63201723661572,0.3935820671347));
#43202=CARTESIAN_POINT('Ctrl Pts',(-29.5724996074913,2.18121714975723,4.10521403455169));
#43203=CARTESIAN_POINT('Ctrl Pts',(-29.3740264557632,-2.26630847004096,
4.05885900746697));
#43204=CARTESIAN_POINT('Ctrl Pts',(-29.175553304035,-4.63921442707336,0.296951214022621));
#43205=CARTESIAN_POINT('Ctrl Pts',(-28.977080152307,-2.76529979572438,-3.73679107840429));
#43206=CARTESIAN_POINT('Ctrl Pts',(-28.7786070005788,1.64002016084422,-4.34980739756368));
#43207=CARTESIAN_POINT('Ctrl Pts',(-28.5801338488507,4.54403607253222,-0.980931544707037));
#43208=CARTESIAN_POINT('Ctrl Pts',(-28.3816606971225,3.2883593788168,3.2859067423807));
#43209=CARTESIAN_POINT('Ctrl Pts',(-28.1831875453944,-0.977540819649672,
4.54476671236201));
#43210=CARTESIAN_POINT('Ctrl Pts',(-27.9847143936663,-4.34858251477885,
1.6432652360574));
#43211=CARTESIAN_POINT('Ctrl Pts',(-27.7862412419382,-3.7388533176929,-2.76251088552642));
#43212=CARTESIAN_POINT('Ctrl Pts',(-27.58776809021,0.29348966371279,-4.63943470060404));
#43213=CARTESIAN_POINT('Ctrl Pts',(-27.3892949384819,4.05716691174368,-2.26933628493606));
#43214=CARTESIAN_POINT('Ctrl Pts',(-27.1908217867538,4.10684036836924,2.17815350988125));
#43215=CARTESIAN_POINT('Ctrl Pts',(-26.9923486350256,0.397038055173797,
4.63172228297628));
#43216=CARTESIAN_POINT('Ctrl Pts',(-26.7938754832975,-3.67622005718519,
2.84532891157148));
#43217=CARTESIAN_POINT('Ctrl Pts',(-26.5954023315694,-4.38420000193776,
-1.54572988160424));
#43218=CARTESIAN_POINT('Ctrl Pts',(-26.3969291798412,-1.07880416411046,
-4.52179965272383));
#43219=CARTESIAN_POINT('Ctrl Pts',(-26.1984560281132,3.21414846959147,-3.35853243832749));
#43220=CARTESIAN_POINT('Ctrl Pts',(-25.9999828763849,4.56481160377853,0.879195965575385));
#43221=CARTESIAN_POINT('Ctrl Pts',(-25.8015097246569,1.73676383642218,4.31209251992246));
#43222=CARTESIAN_POINT('Ctrl Pts',(-25.6030365729287,-2.68114888191185,
3.79762178170733));
#43223=CARTESIAN_POINT('Ctrl Pts',(-25.4045634212006,-4.64468953980158,
-0.193260453101312));
#43224=CARTESIAN_POINT('Ctrl Pts',(-25.2060902694725,-2.35639759233519,
-4.00722858228877));
#43225=CARTESIAN_POINT('Ctrl Pts',(-25.0076171177443,2.08898322585505,-4.15290736785344));
#43226=CARTESIAN_POINT('Ctrl Pts',(-24.8091439660162,4.6220711091526,-0.496939821117236));
#43227=CARTESIAN_POINT('Ctrl Pts',(-24.6106708142881,2.92403170659736,3.61393540377918));
#43228=CARTESIAN_POINT('Ctrl Pts',(-24.41219766256,-1.45071907627053,4.41654895655195));
#43229=CARTESIAN_POINT('Ctrl Pts',(-24.2137245108318,-4.49745544249288,
1.17617391004329));
#43230=CARTESIAN_POINT('Ctrl Pts',(-24.0152513591037,-3.4271399524689,-3.14089195453562));
#43231=CARTESIAN_POINT('Ctrl Pts',(-23.8167782073755,0.780441283340165,
-4.58272865519371));
#43232=CARTESIAN_POINT('Ctrl Pts',(-23.6183050556475,4.27359248746764,-1.82945286217911));
#43233=CARTESIAN_POINT('Ctrl Pts',(-23.4198319039193,3.85462002336901,2.59853708830907));
#43234=CARTESIAN_POINT('Ctrl Pts',(-23.2213587521912,-0.092941156116394,
4.64777930471908));
#43235=CARTESIAN_POINT('Ctrl Pts',(-23.022885600463,-3.95542232442586,2.44236048922118));
#43236=CARTESIAN_POINT('Ctrl Pts',(-22.8244124487349,-4.19703853226137,
-1.99883918377353));
#43237=CARTESIAN_POINT('Ctrl Pts',(-22.6259392970068,-0.596609943671765,
-4.61026540439779));
#43238=CARTESIAN_POINT('Ctrl Pts',(-22.4274661452787,3.54996615153713,-3.0013714943032));
#43239=CARTESIAN_POINT('Ctrl Pts',(-22.2289929935505,4.44683918227362,1.35503203315327));
#43240=CARTESIAN_POINT('Ctrl Pts',(-22.0305198418224,1.27299539459941,4.47101478964274));
#43241=CARTESIAN_POINT('Ctrl Pts',(-21.8320466900943,-3.06617134498456,
3.4941499405536));
#43242=CARTESIAN_POINT('Ctrl Pts',(-21.6335735383661,-4.59850951475821,
-0.681322806423914));
#43243=CARTESIAN_POINT('Ctrl Pts',(-21.435100386638,-1.92128910729172,-4.2331003638087));
#43244=CARTESIAN_POINT('Ctrl Pts',(-21.2366272349099,2.51471401335639,-3.90982147353356));
#43245=CARTESIAN_POINT('Ctrl Pts',(-21.0381540831818,4.64870255509436,-0.00742146443297473));
#43246=CARTESIAN_POINT('Ctrl Pts',(-20.8396809314536,2.5271849048734,3.90177228710943));
#43247=CARTESIAN_POINT('Ctrl Pts',(-20.6412077797255,-1.90776340335524,
4.23921329030442));
#43248=CARTESIAN_POINT('Ctrl Pts',(-20.4427346279974,-4.59631067181976,
0.696001962634392));
#43249=CARTESIAN_POINT('Ctrl Pts',(-20.2442614762692,-3.07731222354206,
-3.48434211906835));
#43250=CARTESIAN_POINT('Ctrl Pts',(-20.0457883245411,1.25871335578393,-4.47505655962543));
#43251=CARTESIAN_POINT('Ctrl Pts',(-19.847315172813,4.4424900192119,-1.36922348543914));
#43252=CARTESIAN_POINT('Ctrl Pts',(-19.6488420210848,3.55953116656451,2.99002147118228));
#43253=CARTESIAN_POINT('Ctrl Pts',(-19.4503688693567,-0.581886737885667,
4.61214682638659));
#43254=CARTESIAN_POINT('Ctrl Pts',(-19.2518957176286,-4.19063502393284,
2.01222976323844));
#43255=CARTESIAN_POINT('Ctrl Pts',(-19.0534225659004,-3.96320040061246,
-2.42971873031846));
#43256=CARTESIAN_POINT('Ctrl Pts',(-18.8549494141723,-0.107780625542997,
-4.64745886056377));
#43257=CARTESIAN_POINT('Ctrl Pts',(-18.6564762624442,3.84630347875288,-2.61083129926249));
#43258=CARTESIAN_POINT('Ctrl Pts',(-18.4580031107161,4.27941198265269,1.81579833863889));
#43259=CARTESIAN_POINT('Ctrl Pts',(-18.2595299589879,0.79506954743727,4.58021341627364));
#43260=CARTESIAN_POINT('Ctrl Pts',(-18.0610568072598,-3.417093896341,3.15181849532368));
#43261=CARTESIAN_POINT('Ctrl Pts',(-17.8625836555317,-4.50118793536699,
-1.16180794212383));
#43262=CARTESIAN_POINT('Ctrl Pts',(-17.6641105038036,-1.46481332682715,
-4.41189442772884));
#43263=CARTESIAN_POINT('Ctrl Pts',(-17.4656373520754,2.91247782960961,-3.62325315371527));
#43264=CARTESIAN_POINT('Ctrl Pts',(-17.2671642003473,4.62363423318624,0.482179428826549));
#43265=CARTESIAN_POINT('Ctrl Pts',(-17.0686910486191,2.1022324389674,4.14621626262165));
#43266=CARTESIAN_POINT('Ctrl Pts',(-16.870217896891,-2.34359085887269,4.01473192256763));
#43267=CARTESIAN_POINT('Ctrl Pts',(-16.6717447451629,-4.64404880086273,
0.208089545822435));
#43268=CARTESIAN_POINT('Ctrl Pts',(-16.4732715934348,-2.69326068148164,
-3.78904175557095));
#43269=CARTESIAN_POINT('Ctrl Pts',(-16.2747984417066,1.72298685819398,-4.317615871099));
#43270=CARTESIAN_POINT('Ctrl Pts',(-16.0763252899785,4.56198114132962,-0.893766518744185));
#43271=CARTESIAN_POINT('Ctrl Pts',(-15.8778521382504,3.22485557931545,3.34825283042266));
#43272=CARTESIAN_POINT('Ctrl Pts',(-15.6793789865222,-1.06436096363523,
4.52522112862619));
#43273=CARTESIAN_POINT('Ctrl Pts',(-15.4809058347941,-4.37924227701401,
1.55972036054167));
#43274=CARTESIAN_POINT('Ctrl Pts',(-15.282432683066,-3.68528619865666,-2.83357656643789));
#43275=CARTESIAN_POINT('Ctrl Pts',(-15.0839595313379,0.382247356783641,
-4.63296638042055));
#43276=CARTESIAN_POINT('Ctrl Pts',(-14.8854863796097,4.09986478522412,-2.19125518065658));
#43277=CARTESIAN_POINT('Ctrl Pts',(-14.6870132278816,4.06439201850983,2.25637054664095));
#43278=CARTESIAN_POINT('Ctrl Pts',(-14.4885400761535,0.308301467299323,
4.63847396555551));
#43279=CARTESIAN_POINT('Ctrl Pts',(-14.2900669244253,-3.73001380952726,
2.77443462792171));
#43280=CARTESIAN_POINT('Ctrl Pts',(-14.0915937726972,-4.3538071472935,-1.62937222513801));
#43281=CARTESIAN_POINT('Ctrl Pts',(-13.8931206209691,-0.992046869976568,
-4.54162234577525));
#43282=CARTESIAN_POINT('Ctrl Pts',(-13.6946474692409,3.2778510108686,-3.29638943003145));
#43283=CARTESIAN_POINT('Ctrl Pts',(-13.4961743175128,4.54714493657699,0.966417844225444));
#43284=CARTESIAN_POINT('Ctrl Pts',(-13.2977011657847,1.65390034664457,4.34454878753181));
#43285=CARTESIAN_POINT('Ctrl Pts',(-13.0992280140565,-2.75335446067982,
3.74560138532248));
#43286=CARTESIAN_POINT('Ctrl Pts',(-12.9007548623284,-4.64013891800504,
-0.282137104064989));
#43287=CARTESIAN_POINT('Ctrl Pts',(-12.7022817106003,-2.27925649127012,
-4.05160219800491));
#43288=CARTESIAN_POINT('Ctrl Pts',(-12.5038085588722,2.16809845047511,-4.11215753989588));
#43289=CARTESIAN_POINT('Ctrl Pts',(-12.305335407144,4.63073695329427,-0.408369677216674));
#43290=CARTESIAN_POINT('Ctrl Pts',(-12.1068622554159,2.85431530018207,3.66924715589203));
#43291=CARTESIAN_POINT('Ctrl Pts',(-11.9083891036878,-1.53499807696976,
4.38796894104485));
#43292=CARTESIAN_POINT('Ctrl Pts',(-11.7099159519597,-4.51914651965373,
1.08986478875911));
#43293=CARTESIAN_POINT('Ctrl Pts',(-11.5114428002315,-3.36638670270264,
-3.20592125476317));
#43294=CARTESIAN_POINT('Ctrl Pts',(-11.3129696485034,0.868024239072622,
-4.56694913966179));
#43295=CARTESIAN_POINT('Ctrl Pts',(-11.1144964967753,4.30783013129569,-1.74730938410351));
#43296=CARTESIAN_POINT('Ctrl Pts',(-10.9160233450471,3.80417059840855,2.67184890704529));
#43297=CARTESIAN_POINT('Ctrl Pts',(-10.717550193319,-0.181895336035743,
4.64514850253505));
#43298=CARTESIAN_POINT('Ctrl Pts',(-10.5190770415909,-4.00145099807289,
2.36619534990175));
#43299=CARTESIAN_POINT('Ctrl Pts',(-10.3206038898628,-4.15800622131905,
-2.07881571750535));
#43300=CARTESIAN_POINT('Ctrl Pts',(-10.1221307381346,-0.508247529807154,
-4.62084137060774));
#43301=CARTESIAN_POINT('Ctrl Pts',(-9.92365758640649,3.60677012041613,-2.93286546270854));
#43302=CARTESIAN_POINT('Ctrl Pts',(-9.72518443467835,4.4200853281841,1.43990840522821));
#43303=CARTESIAN_POINT('Ctrl Pts',(-9.52671128295023,1.18717467827454,4.49456413984039));
#43304=CARTESIAN_POINT('Ctrl Pts',(-9.32823813122209,-3.13249709142274,
3.43481476881992));
#43305=CARTESIAN_POINT('Ctrl Pts',(-9.12976497949398,-4.58462450635486,
-0.769226013344334));
#43306=CARTESIAN_POINT('Ctrl Pts',(-8.93129182776583,-1.83990393125596,
-4.26910342432976));
#43307=CARTESIAN_POINT('Ctrl Pts',(-8.73281867603771,2.58909789851022,-3.86096653647828));
#43308=CARTESIAN_POINT('Ctrl Pts',(-8.53434552430957,4.64799279884426,0.0815687793655434));
#43309=CARTESIAN_POINT('Ctrl Pts',(-8.33587237258145,2.45203123089627,3.94943456289434));
#43310=CARTESIAN_POINT('Ctrl Pts',(-8.13739922085332,-1.98856396595975,
4.20191669088779));
#43311=CARTESIAN_POINT('Ctrl Pts',(-7.93892606912519,-4.60879183022014,
0.607888468036587));
#43312=CARTESIAN_POINT('Ctrl Pts',(-7.74045291739705,-3.01004850015028,
-3.54261182612741));
#43313=CARTESIAN_POINT('Ctrl Pts',(-7.54197976566894,1.34414753498608,-4.45014133798747));
#43314=CARTESIAN_POINT('Ctrl Pts',(-7.34350661394079,4.46788666515927,-1.28393117851835));
#43315=CARTESIAN_POINT('Ctrl Pts',(-7.14503346221267,3.50164173134291,3.05761274676646));
#43316=CARTESIAN_POINT('Ctrl Pts',(-6.94656031048454,-0.670069220816254,
4.60016279746532));
#43317=CARTESIAN_POINT('Ctrl Pts',(-6.74808715875641,-4.22838671869335,
1.93164082610646));
#43318=CARTESIAN_POINT('Ctrl Pts',(-6.54961400702828,-3.91596272468331,
-2.50514000860802));
#43319=CARTESIAN_POINT('Ctrl Pts',(-6.35114085530016,-0.0187957997636384,
-4.64867048109021));
#43320=CARTESIAN_POINT('Ctrl Pts',(-6.15266770357202,3.89557713941664,-2.53672412274591));
#43321=CARTESIAN_POINT('Ctrl Pts',(-5.95419455184391,4.24386848014819,1.8973852657751));
#43322=CARTESIAN_POINT('Ctrl Pts',(-5.75572140011576,0.707246045382618,
4.59459394888022));
#43323=CARTESIAN_POINT('Ctrl Pts',(-5.55724824838764,-3.47680217990147,
3.08582843446728));
#43324=CARTESIAN_POINT('Ctrl Pts',(-5.35877509665951,-4.47812295987505,
-1.24776010426379));
#43325=CARTESIAN_POINT('Ctrl Pts',(-5.16030194493138,-1.38008918797814,
-4.43912653089702));
#43326=CARTESIAN_POINT('Ctrl Pts',(-4.96182879320324,2.98130312838602,-3.56683643984536));
#43327=CARTESIAN_POINT('Ctrl Pts',(-4.76335564147512,4.61355676801949,0.570600082934498));
#43328=CARTESIAN_POINT('Ctrl Pts',(-4.56488248974698,2.02247731019143,4.18569899305294));
#43329=CARTESIAN_POINT('Ctrl Pts',(-4.36640933801885,-2.42001438061241,
3.96913352904242));
#43330=CARTESIAN_POINT('Ctrl Pts',(-4.16793618629072,-4.64718121967184,
0.119151613750008));
#43331=CARTESIAN_POINT('Ctrl Pts',(-3.9694630345626,-2.62023457294503,-3.83990382567675));
#43332=CARTESIAN_POINT('Ctrl Pts',(-3.77098988283446,1.80532216910622,-4.2838420471841));
#43333=CARTESIAN_POINT('Ctrl Pts',(-3.57251673110634,4.57825424888385,-0.806273921550659));
#43334=CARTESIAN_POINT('Ctrl Pts',(-3.37404357937821,3.16017012504447,3.40937180891919));
#43335=CARTESIAN_POINT('Ctrl Pts',(-3.17557042765009,-1.15079139389106,
4.50401724481208));
#43336=CARTESIAN_POINT('Ctrl Pts',(-2.97709727592194,-4.40829647230588,
1.47560370320468));
#43337=CARTESIAN_POINT('Ctrl Pts',(-2.77862412419382,-3.6303697878378,-2.9036034622217));
#43338=CARTESIAN_POINT('Ctrl Pts',(-2.58015097246569,0.470867420796771,
-4.62480083442049));
#43339=CARTESIAN_POINT('Ctrl Pts',(-2.38167782073757,4.14105545114363,-2.11236977893991));
#43340=CARTESIAN_POINT('Ctrl Pts',(-2.18320466900942,4.02046314377869,2.33375828107032));
#43341=CARTESIAN_POINT('Ctrl Pts',(-1.98473151728131,0.219434708775458,
4.64353032567314));
#43342=CARTESIAN_POINT('Ctrl Pts',(-1.78625836555316,-3.78240772570626,
2.70251482356271));
#43343=CARTESIAN_POINT('Ctrl Pts',(-1.58778521382503,-4.32188158398657,
-1.71240070088942));
#43344=CARTESIAN_POINT('Ctrl Pts',(-1.3893120620969,-0.90480577337975,-4.55981265027423));
#43345=CARTESIAN_POINT('Ctrl Pts',(-1.19083891036878,3.34012231182713,-3.2329771300526));
#43346=CARTESIAN_POINT('Ctrl Pts',(-0.992365758640643,4.52825177242018,
1.05316839446738));
#43347=CARTESIAN_POINT('Ctrl Pts',(-0.793892606912516,1.5695887441549,4.37563724216484));
#43348=CARTESIAN_POINT('Ctrl Pts',(-0.595419455184388,-2.82293548626305,
3.69177659323615));
#43349=CARTESIAN_POINT('Ctrl Pts',(-0.396946303456266,-4.63702310608274,
-0.370061573871447));
#43350=CARTESIAN_POINT('Ctrl Pts',(-0.198473151728126,-2.19487812995514,
-4.09631897812866));
#43351=CARTESIAN_POINT('Ctrl Pts',(-0.0661577172427097,0.75551006232788,
-4.07532749258864));
#43352=CARTESIAN_POINT('Ctrl Pts',(0.,1.9005636551884,-3.44330463255532));
#43353=CARTESIAN_POINT('Ctrl Pts',(-54.8403753524613,2.14656790565188,-3.00907133330622));
#43354=CARTESIAN_POINT('Ctrl Pts',(-54.7742176352186,3.14721940444736,-2.29524100024571));
#43355=CARTESIAN_POINT('Ctrl Pts',(-54.6419022007332,4.36310735044169,0.19681737971748));
#43356=CARTESIAN_POINT('Ctrl Pts',(-54.443429049005,2.19665054817406,3.77980425424614));
#43357=CARTESIAN_POINT('Ctrl Pts',(-54.2449558972769,-1.98260099992042,
3.89172142956237));
#43358=CARTESIAN_POINT('Ctrl Pts',(-54.0464827455487,-4.34592358414638,
0.446568491290883));
#43359=CARTESIAN_POINT('Ctrl Pts',(-53.8480095938207,-2.7314433830302,-3.41021906903733));
#43360=CARTESIAN_POINT('Ctrl Pts',(-53.6495364420925,1.38372868081164,-4.14375004305525));
#43361=CARTESIAN_POINT('Ctrl Pts',(-53.4510632903644,4.23206450278455,-1.0847911861996));
#43362=CARTESIAN_POINT('Ctrl Pts',(-53.2525901386363,3.20636848042456,2.96760958715623));
#43363=CARTESIAN_POINT('Ctrl Pts',(-53.0541169869081,-0.754535021833214,
4.30319552163747));
#43364=CARTESIAN_POINT('Ctrl Pts',(-52.8556438351801,-4.02470267833369,
1.6996692062514));
#43365=CARTESIAN_POINT('Ctrl Pts',(-52.6571706834518,-3.61059580179964,
-2.45982277671647));
#43366=CARTESIAN_POINT('Ctrl Pts',(-52.4586975317238,0.108721320903615,
-4.36751838360758));
#43367=CARTESIAN_POINT('Ctrl Pts',(-52.2602243799956,3.72851000157542,-2.27712466543675));
#43368=CARTESIAN_POINT('Ctrl Pts',(-52.0617512282675,3.93515491590644,1.89779831841912));
#43369=CARTESIAN_POINT('Ctrl Pts',(-51.8632780765393,0.539487205671952,
4.33543816108556));
#43370=CARTESIAN_POINT('Ctrl Pts',(-51.6648049248112,-3.35003639980807,
2.80434194871354));
#43371=CARTESIAN_POINT('Ctrl Pts',(-51.4663317730831,-4.17287646566163,
-1.29390066104614));
#43372=CARTESIAN_POINT('Ctrl Pts',(-51.267858621355,-1.17579001023567,-4.20768264338388));
#43373=CARTESIAN_POINT('Ctrl Pts',(-51.0693854696268,2.89763577350922,-3.26967634074781));
#43374=CARTESIAN_POINT('Ctrl Pts',(-50.8709123178987,4.31851352219464,0.661450845288393));
#43375=CARTESIAN_POINT('Ctrl Pts',(-50.6724391661706,1.78614606032967,3.98707390524443));
#43376=CARTESIAN_POINT('Ctrl Pts',(-50.4739660144425,-2.38129172253409,
3.66285762271801));
#43377=CARTESIAN_POINT('Ctrl Pts',(-50.2754928627142,-4.36885210329787,
-0.0144046379382577));
#43378=CARTESIAN_POINT('Ctrl Pts',(-50.0770197109862,-2.35708644242635,
-3.6784806205214));
#43379=CARTESIAN_POINT('Ctrl Pts',(-49.878546559258,1.81239867372601,-3.9752090816288));
#43380=CARTESIAN_POINT('Ctrl Pts',(-49.68007340753,4.32278134486142,-0.632959424273409));
#43381=CARTESIAN_POINT('Ctrl Pts',(-49.4816002558018,2.87601197989481,3.28871270826757));
#43382=CARTESIAN_POINT('Ctrl Pts',(-49.2831271040736,-1.20351064099935,
4.19983789284593));
#43383=CARTESIAN_POINT('Ctrl Pts',(-49.0846539523456,-4.18131790718314,
1.26635569532051));
#43384=CARTESIAN_POINT('Ctrl Pts',(-48.8861808006174,-3.33147132072511,
-2.82637135334204));
#43385=CARTESIAN_POINT('Ctrl Pts',(-48.6877076488893,0.568064219917555,
-4.33178707120854));
#43386=CARTESIAN_POINT('Ctrl Pts',(-48.4892344971611,3.94758352450775,-1.8718067488612));
#43387=CARTESIAN_POINT('Ctrl Pts',(-48.290761345433,3.71341364749161,2.30165924295085));
#43388=CARTESIAN_POINT('Ctrl Pts',(-48.0922881937049,0.0799179192503589,
4.36814483668739));
#43389=CARTESIAN_POINT('Ctrl Pts',(-47.8938150419767,-3.62673611417318,
2.43595183577544));
#43390=CARTESIAN_POINT('Ctrl Pts',(-47.6953418902486,-4.01341047422385,
-1.72615542563737));
#43391=CARTESIAN_POINT('Ctrl Pts',(-47.4968687385206,-0.726136475239662,
-4.30810886670719));
#43392=CARTESIAN_POINT('Ctrl Pts',(-47.2983955867923,3.22585595431062,-2.94634172324065));
#43393=CARTESIAN_POINT('Ctrl Pts',(-47.0999224350642,4.22484164160472,1.11255979229578));
#43394=CARTESIAN_POINT('Ctrl Pts',(-46.9014492833361,1.35633106455037,4.15300400088985));
#43395=CARTESIAN_POINT('Ctrl Pts',(-46.702976131608,-2.75378944024938,3.39171341755782));
#43396=CARTESIAN_POINT('Ctrl Pts',(-46.5045029798798,-4.34304140690395,
-0.474412822327436));
#43397=CARTESIAN_POINT('Ctrl Pts',(-46.3060298281518,-1.95659491146608,
-3.90625300518234));
#43398=CARTESIAN_POINT('Ctrl Pts',(-46.1075566764235,2.22095386729056,-3.76223870952363));
#43399=CARTESIAN_POINT('Ctrl Pts',(-45.9090835246954,4.36540140493793,-0.17420321993839));
#43400=CARTESIAN_POINT('Ctrl Pts',(-45.7106103729674,2.513681734868,3.57330104019546));
#43401=CARTESIAN_POINT('Ctrl Pts',(-45.5121372212391,-1.63910754775918,
4.04974105776527));
#43402=CARTESIAN_POINT('Ctrl Pts',(-45.3136640695111,-4.29142820798936,
0.818975044640645));
#43403=CARTESIAN_POINT('Ctrl Pts',(-45.1151909177829,-3.01529805963144,
-3.16149550049559));
#43404=CARTESIAN_POINT('Ctrl Pts',(-44.9167177660548,1.02109033525629,-4.24787602400507));
#43405=CARTESIAN_POINT('Ctrl Pts',(-44.7182446143267,4.12275421448949,-1.44567419392479));
#43406=CARTESIAN_POINT('Ctrl Pts',(-44.5197714625986,3.45037450204169,2.67992387648073));
#43407=CARTESIAN_POINT('Ctrl Pts',(-44.3212983108704,-0.380540282073574,
4.35227127851542));
#43408=CARTESIAN_POINT('Ctrl Pts',(-44.1228251591423,-3.86310162617809,
2.04047102745693));
#43409=CARTESIAN_POINT('Ctrl Pts',(-43.9243520074141,-3.80931004265721,
-2.13921321681172));
#43410=CARTESIAN_POINT('Ctrl Pts',(-43.725878855686,-0.268407317586806,
-4.36062308620417));
#43411=CARTESIAN_POINT('Ctrl Pts',(-43.5274057039579,3.51820030867284,-2.59023990705981));
#43412=CARTESIAN_POINT('Ctrl Pts',(-43.3289325522297,4.08418389614513,1.55129561674739));
#43413=CARTESIAN_POINT('Ctrl Pts',(-43.1304594005017,0.911431857243973,
4.27274714413007));
#43414=CARTESIAN_POINT('Ctrl Pts',(-42.9319862487735,-3.09566134805425,
3.08284884582977));
#43415=CARTESIAN_POINT('Ctrl Pts',(-42.7335130970454,-4.26893030266636,
-0.92914490745409));
#43416=CARTESIAN_POINT('Ctrl Pts',(-42.5350399453172,-1.53434343713571,
-4.09058264859536));
#43417=CARTESIAN_POINT('Ctrl Pts',(-42.3365667935891,2.60480909374755,-3.50742722992238));
#43418=CARTESIAN_POINT('Ctrl Pts',(-42.138093641861,4.35947238361319,0.286490356879277));
#43419=CARTESIAN_POINT('Ctrl Pts',(-41.9396204901329,2.12339599885507,3.81814950206473));
#43420=CARTESIAN_POINT('Ctrl Pts',(-41.7411473384047,-2.05647539408362,
3.85460570507537));
#43421=CARTESIAN_POINT('Ctrl Pts',(-41.5426741866766,-4.35381210784742,
0.362486299923509));
#43422=CARTESIAN_POINT('Ctrl Pts',(-41.3442010349485,-2.66559066554748,
-3.46145960424458));
#43423=CARTESIAN_POINT('Ctrl Pts',(-41.1457278832203,1.46276056523167,-4.11672293418855));
#43424=CARTESIAN_POINT('Ctrl Pts',(-40.9472547314922,4.25207438311479,-1.00346381525687));
#43425=CARTESIAN_POINT('Ctrl Pts',(-40.748781579764,3.1489625937313,3.02838418489993));
#43426=CARTESIAN_POINT('Ctrl Pts',(-40.550308428036,-0.836766368305163,
4.28799466335307));
#43427=CARTESIAN_POINT('Ctrl Pts',(-40.3518352763078,-4.05650429965212,
1.62229746192699));
#43428=CARTESIAN_POINT('Ctrl Pts',(-40.1533621245797,-3.56284500665734,
-2.5284801060336));
#43429=CARTESIAN_POINT('Ctrl Pts',(-39.9548889728515,0.192306887150334,
-4.36464136547615));
#43430=CARTESIAN_POINT('Ctrl Pts',(-39.7564158211234,3.77141758681283,-2.20533117103754));
#43431=CARTESIAN_POINT('Ctrl Pts',(-39.5579426693953,3.89810458267071,1.97277896649182));
#43432=CARTESIAN_POINT('Ctrl Pts',(-39.3594695176672,0.456396312997958,
4.3449716447352));
#43433=CARTESIAN_POINT('Ctrl Pts',(-39.160996365939,-3.40310537600674,2.73969888634954));
#43434=CARTESIAN_POINT('Ctrl Pts',(-38.9625232142109,-4.14734300415746,
-1.37354366291613));
#43435=CARTESIAN_POINT('Ctrl Pts',(-38.7640500624828,-1.09502801892821,
-4.22941956133854));
#43436=CARTESIAN_POINT('Ctrl Pts',(-38.5655769107546,2.95969537159059,-3.21360848509214));
#43437=CARTESIAN_POINT('Ctrl Pts',(-38.3671037590266,4.30506021940944,0.743997779115886));
#43438=CARTESIAN_POINT('Ctrl Pts',(-38.1686306072984,1.70949526943414,4.02053505293178));
#43439=CARTESIAN_POINT('Ctrl Pts',(-37.9701574555703,-2.45097249331184,
3.61660199981967));
#43440=CARTESIAN_POINT('Ctrl Pts',(-37.7716843038421,-4.36777581463652,
-0.0980337755429264));
#43441=CARTESIAN_POINT('Ctrl Pts',(-37.573211152114,-2.28623835076616,-3.72292766402423));
#43442=CARTESIAN_POINT('Ctrl Pts',(-37.3747380003859,1.88816294826562,-3.93978639888863));
#43443=CARTESIAN_POINT('Ctrl Pts',(-37.1762648486577,4.33410581775851,-0.550093581623009));
#43444=CARTESIAN_POINT('Ctrl Pts',(-36.9777916969296,2.81253002468074,3.34316482518291));
#43445=CARTESIAN_POINT('Ctrl Pts',(-36.7793185452015,-1.28368649734259,
4.17602983282103));
#43446=CARTESIAN_POINT('Ctrl Pts',(-36.5808453934733,-4.20479323911358,
1.18608178654579));
#43447=CARTESIAN_POINT('Ctrl Pts',(-36.3823722417453,-3.2767563858946,-2.88962692671043));
#43448=CARTESIAN_POINT('Ctrl Pts',(-36.1838990900171,0.650882383010416,
-4.32011901590195));
#43449=CARTESIAN_POINT('Ctrl Pts',(-35.985425938289,3.98269167512894,-1.79589621329561));
#43450=CARTESIAN_POINT('Ctrl Pts',(-35.7869527865608,3.66867315113963,2.37232238495911));
#43451=CARTESIAN_POINT('Ctrl Pts',(-35.5884796348327,-0.00371496649886586,
4.36887427000306));
#43452=CARTESIAN_POINT('Ctrl Pts',(-35.3900064831046,-3.67270233677799,
2.36607982399083));
#43453=CARTESIAN_POINT('Ctrl Pts',(-35.1915333313765,-3.97963172417899,
-1.80266678229203));
#43454=CARTESIAN_POINT('Ctrl Pts',(-34.9930601796483,-0.643534429780106,
-4.3212196919109));
#43455=CARTESIAN_POINT('Ctrl Pts',(-34.7945870279202,3.28166589244464,-2.88405013105466));
#43456=CARTESIAN_POINT('Ctrl Pts',(-34.5961138761921,4.20277004810898,1.19323095450504));
#43457=CARTESIAN_POINT('Ctrl Pts',(-34.3976407244639,1.27658267433185,4.17820689574687));
#43458=CARTESIAN_POINT('Ctrl Pts',(-34.1991675727358,-2.8182115119447,3.33837686039389));
#43459=CARTESIAN_POINT('Ctrl Pts',(-34.0006944210077,-4.33316403332743,
-0.557463584773404));
#43460=CARTESIAN_POINT('Ctrl Pts',(-33.8022212692795,-1.88146001859966,
-3.94299180654511));
#43461=CARTESIAN_POINT('Ctrl Pts',(-33.6037481175514,2.29256644291489,-3.71903418818535));
#43462=CARTESIAN_POINT('Ctrl Pts',(-33.4052749658233,4.3679362195421,-0.0906055742386371));
#43463=CARTESIAN_POINT('Ctrl Pts',(-33.2068018140952,2.44481837342964,3.62076501709402));
#43464=CARTESIAN_POINT('Ctrl Pts',(-33.008328662367,-1.71633032172986,4.01762198505305));
#43465=CARTESIAN_POINT('Ctrl Pts',(-32.8098555106389,-4.30631927392746,
0.736675300978531));
#43466=CARTESIAN_POINT('Ctrl Pts',(-32.6113823589108,-2.95422586710896,
-3.21863724488722));
#43467=CARTESIAN_POINT('Ctrl Pts',(-32.4129092071827,1.10221919932485,-4.22755118534484));
#43468=CARTESIAN_POINT('Ctrl Pts',(-32.2144360554545,4.14967292418903,-1.36648849622798));
#43469=CARTESIAN_POINT('Ctrl Pts',(-32.0159629037264,3.39844118483932,2.7454824168548));
#43470=CARTESIAN_POINT('Ctrl Pts',(-31.8174897519983,-0.463784930617257,
4.34418919088514));
#43471=CARTESIAN_POINT('Ctrl Pts',(-31.6190166002701,-3.90145395286594,
1.96614680065802));
#43472=CARTESIAN_POINT('Ctrl Pts',(-31.420543448542,-3.7676616356771,-2.21174184459168));
#43473=CARTESIAN_POINT('Ctrl Pts',(-31.2220702968138,-0.184883880119101,
-4.36496210051622));
#43474=CARTESIAN_POINT('Ctrl Pts',(-31.0235971450857,3.56713991501999,-2.52241729591716));
#43475=CARTESIAN_POINT('Ctrl Pts',(-30.8251239933576,4.05373947274123,1.62919381143267));
#43476=CARTESIAN_POINT('Ctrl Pts',(-30.6266508416295,0.829472778558662,
4.28941150948485));
#43477=CARTESIAN_POINT('Ctrl Pts',(-30.4281776899014,-3.15410826266673,
3.02302452114573));
#43478=CARTESIAN_POINT('Ctrl Pts',(-30.2297045381732,-4.25036169305628,
-1.01069365599607));
#43479=CARTESIAN_POINT('Ctrl Pts',(-30.0312313864451,-1.45575734355953,
-4.11920462525759));
#43480=CARTESIAN_POINT('Ctrl Pts',(-29.8327582347169,2.67147354336079,-3.45692136086352));
#43481=CARTESIAN_POINT('Ctrl Pts',(-29.6342850829888,4.35318934931119,0.369890087883597));
#43482=CARTESIAN_POINT('Ctrl Pts',(-29.4358119312607,2.04991708359791,3.85809747653482));
#43483=CARTESIAN_POINT('Ctrl Pts',(-29.2373387795326,-2.129886265545,3.81453282643021));
#43484=CARTESIAN_POINT('Ctrl Pts',(-29.0388656278044,-4.35995329928042,
0.279076004279576));
#43485=CARTESIAN_POINT('Ctrl Pts',(-28.8403924760763,-2.59884041951351,
-3.51185202734594));
#43486=CARTESIAN_POINT('Ctrl Pts',(-28.6419193243482,1.54129786918891,-4.08796735144797));
#43487=CARTESIAN_POINT('Ctrl Pts',(-28.44344617262,4.27050427996367,-0.921883605930295));
#43488=CARTESIAN_POINT('Ctrl Pts',(-28.244973020892,3.09041402337959,3.08810902530494));
#43489=CARTESIAN_POINT('Ctrl Pts',(-28.0464998691637,-0.918696988209928,
4.27119093835957));
#43490=CARTESIAN_POINT('Ctrl Pts',(-27.8480267174357,-4.08681620143686,
1.54434760457097));
#43491=CARTESIAN_POINT('Ctrl Pts',(-27.6495535657075,-3.5137901285336,-2.59621938993813));
#43492=CARTESIAN_POINT('Ctrl Pts',(-27.4510804139794,0.275822824688006,
-4.36016031327428));
#43493=CARTESIAN_POINT('Ctrl Pts',(-27.2526072622512,3.81294258772753,-2.13273181876311));
#43494=CARTESIAN_POINT('Ctrl Pts',(-27.0541341105232,3.85962591192093,2.04703786191156));
#43495=CARTESIAN_POINT('Ctrl Pts',(-26.855660958795,0.373138040029648,4.35291215063591));
#43496=CARTESIAN_POINT('Ctrl Pts',(-26.6571878070669,-3.45492712595231,
2.67405212036522));
#43497=CARTESIAN_POINT('Ctrl Pts',(-26.4587146553387,-4.1202896661995,-1.45268346678852));
#43498=CARTESIAN_POINT('Ctrl Pts',(-26.2602415036106,-1.01386470673626,
-4.24960639877456));
#43499=CARTESIAN_POINT('Ctrl Pts',(-26.0617683518825,3.02067029766771,-3.15636296088693));
#43500=CARTESIAN_POINT('Ctrl Pts',(-25.8632952001544,4.29002921191622,0.826272079267115));
#43501=CARTESIAN_POINT('Ctrl Pts',(-25.6648220484262,1.63221798382302,4.05252275025762));
#43502=CARTESIAN_POINT('Ctrl Pts',(-25.4663488966981,-2.51975503553682,
3.56902097905823));
#43503=CARTESIAN_POINT('Ctrl Pts',(-25.26787574497,-4.36509883333121,-0.181626989518244));
#43504=CARTESIAN_POINT('Ctrl Pts',(-25.0694025932418,-2.21455240291618,
-3.76601033493126));
#43505=CARTESIAN_POINT('Ctrl Pts',(-24.8709294415137,1.96323525262301,-3.90291987247102));
#43506=CARTESIAN_POINT('Ctrl Pts',(-24.6724562897855,4.34384193674173,-0.467026141318341));
#43507=CARTESIAN_POINT('Ctrl Pts',(-24.4739831380575,2.74801733931117,3.39639174579671));
#43508=CARTESIAN_POINT('Ctrl Pts',(-24.2755099863293,-1.3633919109241,4.15069135028104));
#43509=CARTESIAN_POINT('Ctrl Pts',(-24.0770368346012,-4.22672760724999,
1.1053732049321));
#43510=CARTESIAN_POINT('Ctrl Pts',(-23.878563682873,-3.22084059224854,-2.9518235156247));
#43511=CARTESIAN_POINT('Ctrl Pts',(-23.6800905311449,0.7334620120889,-4.30686773245864));
#43512=CARTESIAN_POINT('Ctrl Pts',(-23.4816173794168,4.01634025725961,-1.71932752144164));
#43513=CARTESIAN_POINT('Ctrl Pts',(-23.2831442276887,3.62258816714416,2.4421161232296));
#43514=CARTESIAN_POINT('Ctrl Pts',(-23.0846710759605,-0.0873464907944999,
4.36800260744161));
#43515=CARTESIAN_POINT('Ctrl Pts',(-22.8861979242324,-3.71732259513318,
2.29534069623296));
#43516=CARTESIAN_POINT('Ctrl Pts',(-22.6877247725042,-3.94439452704584,
-1.87851750140415));
#43517=CARTESIAN_POINT('Ctrl Pts',(-22.4892516207762,-0.560696543172442,
-4.33274688558486));
#43518=CARTESIAN_POINT('Ctrl Pts',(-22.290778469048,3.33627317254483,-2.82070159822491));
#43519=CARTESIAN_POINT('Ctrl Pts',(-22.0923053173199,4.17915823226011,1.27346482393652));
#43520=CARTESIAN_POINT('Ctrl Pts',(-21.8938321655917,1.19636644477205,4.20187857010344));
#43521=CARTESIAN_POINT('Ctrl Pts',(-21.6953590138636,-2.88160077139558,
3.28381686187937));
#43522=CARTESIAN_POINT('Ctrl Pts',(-21.4968858621355,-4.32169865088358,
-0.64031004913398));
#43523=CARTESIAN_POINT('Ctrl Pts',(-21.2984127104074,-1.8056356122114,-3.97828558853997));
#43524=CARTESIAN_POINT('Ctrl Pts',(-21.0999395586792,2.36333884359729,-3.67446672299738));
#43525=CARTESIAN_POINT('Ctrl Pts',(-20.9014664069511,4.36887028204107,-0.00697472359797444));
#43526=CARTESIAN_POINT('Ctrl Pts',(-20.702993255223,2.37505904008103,3.66690206362268));
#43527=CARTESIAN_POINT('Ctrl Pts',(-20.5045201034948,-1.79292409856378,
3.98403054266156));
#43528=CARTESIAN_POINT('Ctrl Pts',(-20.3060469517667,-4.31963216900934,
0.654105582097085));
#43529=CARTESIAN_POINT('Ctrl Pts',(-20.1075738000386,-2.89207101608637,
-3.27459942985154));
#43530=CARTESIAN_POINT('Ctrl Pts',(-19.9091006483104,1.1829441244129,-4.20567704259232));
#43531=CARTESIAN_POINT('Ctrl Pts',(-19.7106274965823,4.17507087045813,-1.28680201069282));
#43532=CARTESIAN_POINT('Ctrl Pts',(-19.5121543448542,3.34526241403874,2.81003479859068));
#43533=CARTESIAN_POINT('Ctrl Pts',(-19.3136811931261,-0.546859612232254,
4.33451505391088));
#43534=CARTESIAN_POINT('Ctrl Pts',(-19.1152080413979,-3.93837648289131,
1.89110202450305));
#43535=CARTESIAN_POINT('Ctrl Pts',(-18.9167348896698,-3.72463246396239,
-2.28345991785894));
#43536=CARTESIAN_POINT('Ctrl Pts',(-18.7182617379417,-0.101292686794748,
-4.36770145267196));
#43537=CARTESIAN_POINT('Ctrl Pts',(-18.5197885862136,3.61477224341217,-2.45367027457396));
#43538=CARTESIAN_POINT('Ctrl Pts',(-18.3213154344854,4.02180944339694,1.70649494258672));
#43539=CARTESIAN_POINT('Ctrl Pts',(-18.1228422827573,0.747209716429057,
4.30450390030546));
#43540=CARTESIAN_POINT('Ctrl Pts',(-17.9243691310291,-3.21139926629802,
2.96209232477511));
#43541=CARTESIAN_POINT('Ctrl Pts',(-17.725895979301,-4.23023541980685,-1.09187200764678));
#43542=CARTESIAN_POINT('Ctrl Pts',(-17.5274228275729,-1.37663774708501,
-4.14631700444764));
#43543=CARTESIAN_POINT('Ctrl Pts',(-17.3289496758448,2.7371589569525,-3.4051486065142));
#43544=CARTESIAN_POINT('Ctrl Pts',(-17.1304765241166,4.34531096730604,0.45315426234418));
#43545=CARTESIAN_POINT('Ctrl Pts',(-16.9320033723885,1.97568691902713,3.89663154353295));
#43546=CARTESIAN_POINT('Ctrl Pts',(-16.7335302206604,-2.20251658075459,
3.77306200579476));
#43547=CARTESIAN_POINT('Ctrl Pts',(-16.5350570689323,-4.36449666417209,
0.195563433446896));
#43548=CARTESIAN_POINT('Ctrl Pts',(-16.3365839172041,-2.53113775589293,
-3.56095743428143));
#43549=CARTESIAN_POINT('Ctrl Pts',(-16.138110765476,1.61927032153549,-4.05771361900581));
#43550=CARTESIAN_POINT('Ctrl Pts',(-15.9396376137479,4.28736913136016,-0.839965546633269));
#43551=CARTESIAN_POINT('Ctrl Pts',(-15.7411644620197,3.03073288457795,3.14670214199071));
#43552=CARTESIAN_POINT('Ctrl Pts',(-15.5426913102916,-1.00029092596905,
4.25282191626866));
#43553=CARTESIAN_POINT('Ctrl Pts',(-15.3442181585635,-4.11563037539103,
1.46583177794371));
#43554=CARTESIAN_POINT('Ctrl Pts',(-15.1457450068353,-3.46344752397278,
-2.66300721680542));
#43555=CARTESIAN_POINT('Ctrl Pts',(-14.9472718551072,0.359237679255288,
-4.35408135866501));
#43556=CARTESIAN_POINT('Ctrl Pts',(-14.7487987033791,3.85307022943922,-2.0593508674046));
#43557=CARTESIAN_POINT('Ctrl Pts',(-14.550325551651,3.81973277356145,2.12054656318871));
#43558=CARTESIAN_POINT('Ctrl Pts',(-14.3518523999228,0.289743020215,4.35925741042068));
#43559=CARTESIAN_POINT('Ctrl Pts',(-14.1533792481947,-3.50548272145052,
2.60742537336791));
#43560=CARTESIAN_POINT('Ctrl Pts',(-13.9549060964666,-4.0917263331258,-1.53129089427051));
#43561=CARTESIAN_POINT('Ctrl Pts',(-13.7564329447384,-0.932329835533015,
-4.26823584936986));
#43562=CARTESIAN_POINT('Ctrl Pts',(-13.5579597930103,3.08053821482908,-3.09796069940352));
#43563=CARTESIAN_POINT('Ctrl Pts',(-13.3594866412822,4.27342600351457,0.908243568959527));
#43564=CARTESIAN_POINT('Ctrl Pts',(-13.161013489554,1.55434252638836,4.08302528754496));
#43565=CARTESIAN_POINT('Ctrl Pts',(-12.9625403378259,-2.5876141432208,3.52013199097342));
#43566=CARTESIAN_POINT('Ctrl Pts',(-12.7640671860978,-4.36082213976002,
-0.265153641215291));
#43567=CARTESIAN_POINT('Ctrl Pts',(-12.5655940343697,-2.14205487054604,
-3.80771284626886));
#43568=CARTESIAN_POINT('Ctrl Pts',(-12.3671208826415,2.03758807464232,-3.86462301216384));
#43569=CARTESIAN_POINT('Ctrl Pts',(-12.1686477309134,4.35198613364198,-0.383787546252879));
#43570=CARTESIAN_POINT('Ctrl Pts',(-11.9701745791853,2.68249756631029,3.4483739638865));
#43571=CARTESIAN_POINT('Ctrl Pts',(-11.7717014274572,-1.44259767149734,
4.12383173107989));
#43572=CARTESIAN_POINT('Ctrl Pts',(-11.573228275729,-4.24711297311721,1.02425952846461));
#43573=CARTESIAN_POINT('Ctrl Pts',(-11.3747551240009,-3.16374443169717,
-3.0129383264475));
#43574=CARTESIAN_POINT('Ctrl Pts',(-11.1762819722727,0.815772843547351,
-4.29203807716119));
#43575=CARTESIAN_POINT('Ctrl Pts',(-10.9778088205446,4.04851693943592,-1.64212873404349));
#43576=CARTESIAN_POINT('Ctrl Pts',(-10.7793356688165,3.5751755846346,2.51101487990485));
#43577=CARTESIAN_POINT('Ctrl Pts',(-10.5808625170883,-0.170946004531315,
4.36553016844526));
#43578=CARTESIAN_POINT('Ctrl Pts',(-10.3823893653603,-3.76058053689973,
2.2237603768306));
#43579=CARTESIAN_POINT('Ctrl Pts',(-10.1839162136321,-3.9077117964787,-1.953679785362));
#43580=CARTESIAN_POINT('Ctrl Pts',(-9.98544306190399,-0.477653173671534,
-4.34268622326693));
#43581=CARTESIAN_POINT('Ctrl Pts',(-9.78696991017584,3.38965778224963,-2.75631934058907));
#43582=CARTESIAN_POINT('Ctrl Pts',(-9.58849675844771,4.15401484726687,1.35323199664997));
#43583=CARTESIAN_POINT('Ctrl Pts',(-9.3900236067196,1.11571177334673,4.22401034881386));
#43584=CARTESIAN_POINT('Ctrl Pts',(-9.19155045499144,-2.94393398783904,
3.22805341704829));
#43585=CARTESIAN_POINT('Ctrl Pts',(-8.99307730326333,-4.3086494613817,-0.722921854010561));
#43586=CARTESIAN_POINT('Ctrl Pts',(-8.79460415153519,-1.72914948027085,
-4.01212141677566));
#43587=CARTESIAN_POINT('Ctrl Pts',(-8.59613099980706,2.43324513281668,-3.62855264695096));
#43588=CARTESIAN_POINT('Ctrl Pts',(-8.39765784807894,4.36820325012155,0.0766586831246986));
#43589=CARTESIAN_POINT('Ctrl Pts',(-8.19918469635081,2.30442930007647,3.71169527157334));
#43590=CARTESIAN_POINT('Ctrl Pts',(-8.00071154462268,-1.86886080833417,
3.94897904111218));
#43591=CARTESIAN_POINT('Ctrl Pts',(-7.80223839289454,-4.33136201435319,
0.571296147973731));
#43592=CARTESIAN_POINT('Ctrl Pts',(-7.60376524116642,-2.828856284943,-3.32936154648439));
#43593=CARTESIAN_POINT('Ctrl Pts',(-7.40529208943829,1.26323552661883,-4.18226161213738));
#43594=CARTESIAN_POINT('Ctrl Pts',(-7.20681893771015,4.19893874551101,-1.2066439406557));
#43595=CARTESIAN_POINT('Ctrl Pts',(-7.00834578598203,3.29085767848375,2.87355736466697));
#43596=CARTESIAN_POINT('Ctrl Pts',(-6.80987263425389,-0.62973388188193,
4.32325241294972));
#43597=CARTESIAN_POINT('Ctrl Pts',(-6.61139948252577,-3.9738556849657,1.81536420124497));
#43598=CARTESIAN_POINT('Ctrl Pts',(-6.41292633079764,-3.68023829674828,
-2.35434115352581));
#43599=CARTESIAN_POINT('Ctrl Pts',(-6.21445317906951,-0.0176643719493505,
-4.3688401387566));
#43600=CARTESIAN_POINT('Ctrl Pts',(-6.01598002734139,3.66107983767315,-2.38402403729976));
#43601=CARTESIAN_POINT('Ctrl Pts',(-5.81750687561325,3.98840550972488,1.78317068106301));
#43602=CARTESIAN_POINT('Ctrl Pts',(-5.61903372388513,0.664672818521727,
4.31801878554499));
#43603=CARTESIAN_POINT('Ctrl Pts',(-5.42056057215698,-3.2675133631987,2.90007458705824));
#43604=CARTESIAN_POINT('Ctrl Pts',(-5.22208742042888,-4.20855885848927,
-1.17265021240391));
#43605=CARTESIAN_POINT('Ctrl Pts',(-5.02361426870072,-1.29701364379981,
-4.17190984994354));
#43606=CARTESIAN_POINT('Ctrl Pts',(-4.8251411169726,2.80184126323327,-3.35212794070143));
#43607=CARTESIAN_POINT('Ctrl Pts',(-4.62666796524447,4.33584012300842,0.536252366271593));
#43608=CARTESIAN_POINT('Ctrl Pts',(-4.42819481351634,1.90073271238126,3.9337375802369));
#43609=CARTESIAN_POINT('Ctrl Pts',(-4.2297216617882,-2.27433972904608,3.73020844310279));
#43610=CARTESIAN_POINT('Ctrl Pts',(-4.03124851006008,-4.36744052458988,
0.111979189505195));
#43611=CARTESIAN_POINT('Ctrl Pts',(-3.83277535833195,-2.46250751086917,
-3.60875782244023));
#43612=CARTESIAN_POINT('Ctrl Pts',(-3.63430220660381,1.69664939424318,-4.02597283674152));
#43613=CARTESIAN_POINT('Ctrl Pts',(-3.43582905487569,4.30266266652348,-0.757739634511082));
#43614=CARTESIAN_POINT('Ctrl Pts',(-3.23735590314757,2.96994122163641,3.20414201594641));
#43615=CARTESIAN_POINT('Ctrl Pts',(-3.03888275141944,-1.08151860912011,
4.23289441676501));
#43616=CARTESIAN_POINT('Ctrl Pts',(-2.8404095996913,-4.14293563075526,1.3867785883475));
#43617=CARTESIAN_POINT('Ctrl Pts',(-2.64193644796318,-3.41183684929971,
-2.72881878902532));
#43618=CARTESIAN_POINT('Ctrl Pts',(-2.44346329623505,0.442523189453244,
-4.34640734406986));
#43619=CARTESIAN_POINT('Ctrl Pts',(-2.24499014450692,3.89178139112368,-1.98521403391992));
#43620=CARTESIAN_POINT('Ctrl Pts',(-2.04651699277878,3.77844823167868,2.19327588263559));
#43621=CARTESIAN_POINT('Ctrl Pts',(-1.84804384105066,0.206225665474638,
4.36400939900059));
#43622=CARTESIAN_POINT('Ctrl Pts',(-1.64957068932251,-3.55472274501437,
2.53983483767964));
#43623=CARTESIAN_POINT('Ctrl Pts',(-1.45109753759439,-4.06172255398183,
-1.6093214062197));
#43624=CARTESIAN_POINT('Ctrl Pts',(-1.25262438586626,-0.850340284733118,
-4.28533117431376));
#43625=CARTESIAN_POINT('Ctrl Pts',(-1.05415123413814,3.13906104629816,-3.03836555223933));
#43626=CARTESIAN_POINT('Ctrl Pts',(-0.855678082409997,4.25567012809769,
0.989772102224669));
#43627=CARTESIAN_POINT('Ctrl Pts',(-0.657204930681874,1.47510612651486,
4.11224234842401));
#43628=CARTESIAN_POINT('Ctrl Pts',(-0.458731778953743,-2.65300668474432,
3.46954722419258));
#43629=CARTESIAN_POINT('Ctrl Pts',(-0.260258627225623,-4.35789388656455,
-0.347785429041922));
#43630=CARTESIAN_POINT('Ctrl Pts',(-0.0617854754974821,-2.06275573044676,
-3.84973786496513));
#43631=CARTESIAN_POINT('Ctrl Pts',(0.0705299589879341,0.710031545354443,
-3.83000997825599));
#43632=CARTESIAN_POINT('Ctrl Pts',(0.136687676230644,1.78615774484866,-3.23603222681993));
#43633=CARTESIAN_POINT('Ctrl Pts',(-54.7036876762306,2.00907721869526,-2.81633609132854));
#43634=CARTESIAN_POINT('Ctrl Pts',(-54.6375299589879,2.94563558462912,-2.14822759292536));
#43635=CARTESIAN_POINT('Ctrl Pts',(-54.5052145245025,4.08364420124533,0.184210950323209));
#43636=CARTESIAN_POINT('Ctrl Pts',(-54.3067413727744,2.05595199767563,3.53770248699744));
#43637=CARTESIAN_POINT('Ctrl Pts',(-54.1082682210462,-1.85561262339514,
3.64245121016469));
#43638=CARTESIAN_POINT('Ctrl Pts',(-53.9097950693181,-4.06756107929776,
0.417965152687526));
#43639=CARTESIAN_POINT('Ctrl Pts',(-53.7113219175901,-2.55649060090452,
-3.19178975159536));
#43640=CARTESIAN_POINT('Ctrl Pts',(-53.5128487658618,1.29509891681229,-3.87833703725392));
#43641=CARTESIAN_POINT('Ctrl Pts',(-53.3143756141338,3.9609948318926,-1.01530878827405));
#43642=CARTESIAN_POINT('Ctrl Pts',(-53.1159024624056,3.0009960792774,2.77753002820876));
#43643=CARTESIAN_POINT('Ctrl Pts',(-52.9174293106774,-0.706205994732919,
4.02756980915926));
#43644=CARTESIAN_POINT('Ctrl Pts',(-52.7189561589495,-3.76691482331964,
1.59080300819131));
#43645=CARTESIAN_POINT('Ctrl Pts',(-52.5204830072211,-3.37933207340578,
-2.30226767563077));
#43646=CARTESIAN_POINT('Ctrl Pts',(-52.3220098554932,0.101757567714737,
-4.08777270154628));
#43647=CARTESIAN_POINT('Ctrl Pts',(-52.1235367037649,3.48969370319916,-2.13127163478629));
#43648=CARTESIAN_POINT('Ctrl Pts',(-51.9250635520369,3.68310272075172,1.77624167266026));
#43649=CARTESIAN_POINT('Ctrl Pts',(-51.7265904003086,0.504932293005767,
4.05774726229975));
#43650=CARTESIAN_POINT('Ctrl Pts',(-51.5281172485807,-3.13546186679357,
2.62471991114639));
#43651=CARTESIAN_POINT('Ctrl Pts',(-51.3296440968524,-3.9055978716149,-1.21102450778185));
#43652=CARTESIAN_POINT('Ctrl Pts',(-51.1311709451244,-1.10047900991836,
-3.93817466480525));
#43653=CARTESIAN_POINT('Ctrl Pts',(-50.9326977933961,2.71203813553055,-3.06024898229756));
#43654=CARTESIAN_POINT('Ctrl Pts',(-50.734224641668,4.0419066702827,0.619083990334728));
#43655=CARTESIAN_POINT('Ctrl Pts',(-50.53575148994,1.67174089839997,3.73169622595682));
#43656=CARTESIAN_POINT('Ctrl Pts',(-50.3372783382118,-2.22876664568314,
3.4282464513475));
#43657=CARTESIAN_POINT('Ctrl Pts',(-50.1388051864837,-4.0890209946186,-0.0134820006620064));
#43658=CARTESIAN_POINT('Ctrl Pts',(-49.9403320347555,-2.20611174773739,
-3.44286877421536));
#43659=CARTESIAN_POINT('Ctrl Pts',(-49.7418588830274,1.69631199506383,-3.72059136094556));
#43660=CARTESIAN_POINT('Ctrl Pts',(-49.5433857312993,4.04590113291796,-0.59241748482227));
#43661=CARTESIAN_POINT('Ctrl Pts',(-49.3449125795711,2.69179937624523,3.07806604376094));
#43662=CARTESIAN_POINT('Ctrl Pts',(-49.146439427843,-1.12642409537688,3.93083238154904));
#43663=CARTESIAN_POINT('Ctrl Pts',(-48.9479662761149,-3.91349862695974,
1.18524383576916));
#43664=CARTESIAN_POINT('Ctrl Pts',(-48.7494931243867,-3.11808590708118,
-2.6453383014911));
#43665=CARTESIAN_POINT('Ctrl Pts',(-48.5510199726586,0.531678909382298,
-4.05433002985349));
#43666=CARTESIAN_POINT('Ctrl Pts',(-48.3525468209305,3.69473525952908,-1.75191489961062));
#43667=CARTESIAN_POINT('Ctrl Pts',(-48.1540736692024,3.47556429178153,2.15423473817737));
#43668=CARTESIAN_POINT('Ctrl Pts',(-47.9556005174742,0.074799064361738,
4.08835902942712));
#43669=CARTESIAN_POINT('Ctrl Pts',(-47.7571273657462,-3.39443857611954,
2.27992570195889));
#43670=CARTESIAN_POINT('Ctrl Pts',(-47.5586542140179,-3.75634590073117,
-1.61559274805332));
#43671=CARTESIAN_POINT('Ctrl Pts',(-47.3601810622899,-0.679626414904852,
-4.03216844758158));
#43672=CARTESIAN_POINT('Ctrl Pts',(-47.1617079105617,3.0192353531112,-2.75762440082553));
#43673=CARTESIAN_POINT('Ctrl Pts',(-46.9632347588336,3.95423460510833,1.04129877617769));
#43674=CARTESIAN_POINT('Ctrl Pts',(-46.7647616071054,1.26945615632396,3.88699826610166));
#43675=CARTESIAN_POINT('Ctrl Pts',(-46.5662884553774,-2.57740536179706,
3.17446941306502));
#43676=CARTESIAN_POINT('Ctrl Pts',(-46.3678153036492,-4.06486350955272,
-0.444026015242831));
#43677=CARTESIAN_POINT('Ctrl Pts',(-46.1693421519211,-1.83127226140475,
-3.65605201797175));
#43678=CARTESIAN_POINT('Ctrl Pts',(-45.970869000193,2.07869865509402,-3.52126204006689));
#43679=CARTESIAN_POINT('Ctrl Pts',(-45.7723958484648,4.08579131833148,-0.16304525921605));
#43680=CARTESIAN_POINT('Ctrl Pts',(-45.5739226967367,2.35267689192458,3.34442609362352));
#43681=CARTESIAN_POINT('Ctrl Pts',(-45.3754495450085,-1.53412040892052,
3.79034945940863));
#43682=CARTESIAN_POINT('Ctrl Pts',(-45.1769763932805,-4.01655620846509,
0.766518543641464));
#43683=CARTESIAN_POINT('Ctrl Pts',(-44.9785032415522,-2.82216398709376,
-2.95899727668966));
#43684=CARTESIAN_POINT('Ctrl Pts',(-44.7800300898242,0.955688066234348,
-3.97579360298834));
#43685=CARTESIAN_POINT('Ctrl Pts',(-44.581556938096,3.85868602097429,-1.35307673287339));
#43686=CARTESIAN_POINT('Ctrl Pts',(-44.3830837863679,3.22937317275983,2.50827099105437));
#43687=CARTESIAN_POINT('Ctrl Pts',(-44.1846106346398,-0.356166142937589,
4.07350219493382));
#43688=CARTESIAN_POINT('Ctrl Pts',(-43.9861374829116,-3.61566454535351,
1.9097759944505));
#43689=CARTESIAN_POINT('Ctrl Pts',(-43.7876643311835,-3.56531838825102,
-2.00219360799722));
#43690=CARTESIAN_POINT('Ctrl Pts',(-43.5891911794554,-0.251215452199397,
-4.08131905761874));
#43691=CARTESIAN_POINT('Ctrl Pts',(-43.3907180277272,3.29285464128601,-2.42433140574198));
#43692=CARTESIAN_POINT('Ctrl Pts',(-43.1922448759991,3.82258618565147,1.45193295532964));
#43693=CARTESIAN_POINT('Ctrl Pts',(-42.993771724271,0.853053367639089,3.99907169296392));
#43694=CARTESIAN_POINT('Ctrl Pts',(-42.7952985725428,-2.8973798941071,2.88538805063197));
#43695=CARTESIAN_POINT('Ctrl Pts',(-42.5968254208148,-3.99549932555275,
-0.869631872123631));
#43696=CARTESIAN_POINT('Ctrl Pts',(-42.3983522690866,-1.43606658661385,
-3.82857508902685));
#43697=CARTESIAN_POINT('Ctrl Pts',(-42.1998791173585,2.43796741557505,-3.28277159334914));
#43698=CARTESIAN_POINT('Ctrl Pts',(-42.0014059656304,4.08024205914369,0.268140247446303));
#43699=CARTESIAN_POINT('Ctrl Pts',(-41.8029328139022,1.98738950504959,3.57359166787763));
#43700=CARTESIAN_POINT('Ctrl Pts',(-41.6044596621741,-1.92475525893321,
3.60771279992113));
#43701=CARTESIAN_POINT('Ctrl Pts',(-41.405986510446,-4.0749443319846,0.339268543682336));
#43702=CARTESIAN_POINT('Ctrl Pts',(-41.2075133587178,-2.49485584239753,
-3.23974825860909));
#43703=CARTESIAN_POINT('Ctrl Pts',(-41.0090402069898,1.36906869811796,-3.85304105264131));
#43704=CARTESIAN_POINT('Ctrl Pts',(-40.8105670552615,3.97972305130484,-0.939190549579057));
#43705=CARTESIAN_POINT('Ctrl Pts',(-40.6120939035335,2.94726712019311,2.8344119276729));
#43706=CARTESIAN_POINT('Ctrl Pts',(-40.4136207518052,-0.783170308055804,
4.01334258718161));
#43707=CARTESIAN_POINT('Ctrl Pts',(-40.2151476000772,-3.79667950616066,
1.51838703267821));
#43708=CARTESIAN_POINT('Ctrl Pts',(-40.016674448349,-3.33463978370818,-2.36652740664806));
#43709=CARTESIAN_POINT('Ctrl Pts',(-39.818201296621,0.179989361135237,-4.08507996046391));
#43710=CARTESIAN_POINT('Ctrl Pts',(-39.6197281448927,3.52985299738349,-2.0640766144619));
#43711=CARTESIAN_POINT('Ctrl Pts',(-39.4212549931647,3.64842551335801,1.84641970499238));
#43712=CARTESIAN_POINT('Ctrl Pts',(-39.2227818414365,0.427163488621416,
4.06667011294186));
#43713=CARTESIAN_POINT('Ctrl Pts',(-39.0243086897084,-3.18513170058709,
2.56421732765008));
#43714=CARTESIAN_POINT('Ctrl Pts',(-38.8258355379803,-3.88169986415499,
-1.28556626360714));
#43715=CARTESIAN_POINT('Ctrl Pts',(-38.6273623862521,-1.02488993749952,
-3.95851930265825));
#43716=CARTESIAN_POINT('Ctrl Pts',(-38.428889234524,2.7701227292573,-3.00777235148504));
#43717=CARTESIAN_POINT('Ctrl Pts',(-38.2304160827959,4.02931507042192,0.696343677200124));
#43718=CARTESIAN_POINT('Ctrl Pts',(-38.0319429310678,1.59999969823682,3.76301414017378));
#43719=CARTESIAN_POINT('Ctrl Pts',(-37.8334697793396,-2.29398426529913,
3.38495356601323));
#43720=CARTESIAN_POINT('Ctrl Pts',(-37.6349966276115,-4.08801364375652,
-0.0917545746338272));
#43721=CARTESIAN_POINT('Ctrl Pts',(-37.4365234758833,-2.13980157577975,
-3.48446892220266));
#43722=CARTESIAN_POINT('Ctrl Pts',(-37.2380503241552,1.76722346148785,-3.68743755074885));
#43723=CARTESIAN_POINT('Ctrl Pts',(-37.0395771724271,4.05650025743267,-0.514859315691648));
#43724=CARTESIAN_POINT('Ctrl Pts',(-36.841104020699,2.63238352935634,3.12903042616705));
#43725=CARTESIAN_POINT('Ctrl Pts',(-36.6426308689709,-1.20146457559858,
3.90854926118213));
#43726=CARTESIAN_POINT('Ctrl Pts',(-36.4441577172427,-3.9354703309336,1.11011158351183));
#43727=CARTESIAN_POINT('Ctrl Pts',(-36.2456845655146,-3.06687554061621,
-2.70454226660923));
#43728=CARTESIAN_POINT('Ctrl Pts',(-36.0472114137865,0.609192452897957,
-4.04340932986483));
#43729=CARTESIAN_POINT('Ctrl Pts',(-35.8487382620583,3.72759468383047,-1.68086654038461));
#43730=CARTESIAN_POINT('Ctrl Pts',(-35.6502651103302,3.43368948701192,2.22037180676785));
#43731=CARTESIAN_POINT('Ctrl Pts',(-35.451791958602,-0.00347701768072103,
4.08904174151521));
#43732=CARTESIAN_POINT('Ctrl Pts',(-35.2533188068739,-3.43746059765524,
2.21452909059092));
#43733=CARTESIAN_POINT('Ctrl Pts',(-35.0548456551458,-3.72473072703346,
-1.68720344493443));
#43734=CARTESIAN_POINT('Ctrl Pts',(-34.8563725034176,-0.602315146384778,
-4.04443950603062));
#43735=CARTESIAN_POINT('Ctrl Pts',(-34.6578993516896,3.07147058638131,-2.69932267254216));
#43736=CARTESIAN_POINT('Ctrl Pts',(-34.4594261999614,3.93357672815235,1.11680283722956));
#43737=CARTESIAN_POINT('Ctrl Pts',(-34.2609530482334,1.19481576242177,3.91058688017211));
#43738=CARTESIAN_POINT('Ctrl Pts',(-34.0624798965051,-2.63770110938717,
3.1245491372426));
#43739=CARTESIAN_POINT('Ctrl Pts',(-33.864006744777,-4.05561879561619,-0.521757259796585));
#43740=CARTESIAN_POINT('Ctrl Pts',(-33.6655335930489,-1.76094986387445,
-3.69043764754619));
#43741=CARTESIAN_POINT('Ctrl Pts',(-33.4670604413208,2.14572434474499,-3.48082482895569));
#43742=CARTESIAN_POINT('Ctrl Pts',(-33.2685872895926,4.08816377450278,-0.0848021600484351));
#43743=CARTESIAN_POINT('Ctrl Pts',(-33.0701141378645,2.28822432543259,3.38884993618843));
#43744=CARTESIAN_POINT('Ctrl Pts',(-32.8716409861364,-1.60639695584012,
3.76028765838113));
#43745=CARTESIAN_POINT('Ctrl Pts',(-32.6731678344083,-4.030493480731,0.689490214064437));
#43746=CARTESIAN_POINT('Ctrl Pts',(-32.4746946826801,-2.76500355421408,
-3.01247901215746));
#43747=CARTESIAN_POINT('Ctrl Pts',(-32.276221530952,1.03162051269905,-3.95677059876919));
#43748=CARTESIAN_POINT('Ctrl Pts',(-32.0777483792238,3.88388054953854,-1.27896299024718));
#43749=CARTESIAN_POINT('Ctrl Pts',(-31.8792752274958,3.18076625741006,2.56963041490939));
#43750=CARTESIAN_POINT('Ctrl Pts',(-31.6808020757676,-0.434078854912396,
4.06593777635907));
#43751=CARTESIAN_POINT('Ctrl Pts',(-31.4823289240395,-3.65156035169144,
1.84021233868835));
#43752=CARTESIAN_POINT('Ctrl Pts',(-31.2838557723113,-3.52633762018943,
-2.07007667537761));
#43753=CARTESIAN_POINT('Ctrl Pts',(-31.0853826205832,-0.173041808122419,
-4.08538015197453));
#43754=CARTESIAN_POINT('Ctrl Pts',(-30.8869094688551,3.33865959716237,-2.36085292802862));
#43755=CARTESIAN_POINT('Ctrl Pts',(-30.6884363171269,3.79409177029381,1.52484166131915));
#43756=CARTESIAN_POINT('Ctrl Pts',(-30.4899631653989,0.776343882968993,
4.01466868233013));
#43757=CARTESIAN_POINT('Ctrl Pts',(-30.2914900136707,-2.95208320181135,
2.82939555790436));
#43758=CARTESIAN_POINT('Ctrl Pts',(-30.0930168619426,-3.9781200614483,-0.945957308871949));
#43759=CARTESIAN_POINT('Ctrl Pts',(-29.8945437102144,-1.36251404262283,
-3.85536378791437));
#43760=CARTESIAN_POINT('Ctrl Pts',(-29.6960705584863,2.50036191363037,-3.23550069608593));
#43761=CARTESIAN_POINT('Ctrl Pts',(-29.4975974067582,4.07436146200666,0.346198108632488));
#43762=CARTESIAN_POINT('Ctrl Pts',(-29.29912425503,1.91861701743858,3.61098091851795));
#43763=CARTESIAN_POINT('Ctrl Pts',(-29.1006511033019,-1.99346406104904,
3.57020664539346));
#43764=CARTESIAN_POINT('Ctrl Pts',(-28.9021779515738,-4.08069217148748,
0.261200794536527));
#43765=CARTESIAN_POINT('Ctrl Pts',(-28.7037047998456,-2.43238104330263,
-3.28691297628758));
#43766=CARTESIAN_POINT('Ctrl Pts',(-28.5052316481175,1.44257557753361,-3.82612730533229));
#43767=CARTESIAN_POINT('Ctrl Pts',(-28.3067584963894,3.99697248739513,-0.862835667153545));
#43768=CARTESIAN_POINT('Ctrl Pts',(-28.1082853446613,2.89246866794238,2.89031130822918));
#43769=CARTESIAN_POINT('Ctrl Pts',(-27.9098121929331,-0.859853156770183,
3.99761516435712));
#43770=CARTESIAN_POINT('Ctrl Pts',(-27.711339041205,-3.82504988809487,1.44542997308453));
#43771=CARTESIAN_POINT('Ctrl Pts',(-27.5128658894769,-3.2887269393743,-2.42992789434984));
#43772=CARTESIAN_POINT('Ctrl Pts',(-27.3143927377487,0.258155985663226,
-4.0808859259445));
#43773=CARTESIAN_POINT('Ctrl Pts',(-27.1159195860206,3.56871826371137,-1.99612735259016));
#43774=CARTESIAN_POINT('Ctrl Pts',(-26.9174464342925,3.61241145547262,1.91592221394187));
#43775=CARTESIAN_POINT('Ctrl Pts',(-26.7189732825643,0.349238024885499,
4.07410201829554));
#43776=CARTESIAN_POINT('Ctrl Pts',(-26.5205001308362,-3.23363419471944,
2.50277532915898));
#43777=CARTESIAN_POINT('Ctrl Pts',(-26.3220269791081,-3.85637933046123,
-1.35963705197279));
#43778=CARTESIAN_POINT('Ctrl Pts',(-26.12355382738,-0.948925249362072,-3.97741314482529));
#43779=CARTESIAN_POINT('Ctrl Pts',(-25.9250806756518,2.82719212574396,-2.95419348344638));
#43780=CARTESIAN_POINT('Ctrl Pts',(-25.7266075239237,4.0152468200539,0.773348192958842));
#43781=CARTESIAN_POINT('Ctrl Pts',(-25.5281343721956,1.52767213122385,3.79295298059278));
#43782=CARTESIAN_POINT('Ctrl Pts',(-25.3296612204674,-2.35836118916179,
3.34042017640912));
#43783=CARTESIAN_POINT('Ctrl Pts',(-25.1311880687393,-4.08550812686082,
-0.169993525935175));
#43784=CARTESIAN_POINT('Ctrl Pts',(-24.9327149170112,-2.07270721349718,
-3.52479208757375));
#43785=CARTESIAN_POINT('Ctrl Pts',(-24.734241765283,1.83748727939098,-3.65293237708858));
#43786=CARTESIAN_POINT('Ctrl Pts',(-24.5357686135549,4.06561276433087,-0.437112461519451));
#43787=CARTESIAN_POINT('Ctrl Pts',(-24.3372954618268,2.57200297202499,3.17884808781425));
#43788=CARTESIAN_POINT('Ctrl Pts',(-24.1388223100987,-1.27606474557768,
3.88483374401012));
#43789=CARTESIAN_POINT('Ctrl Pts',(-23.9403491583705,-3.95599977200709,
1.03457249982091));
#43790=CARTESIAN_POINT('Ctrl Pts',(-23.7418760066424,-3.01454123202818,
-2.76275507671378));
#43791=CARTESIAN_POINT('Ctrl Pts',(-23.5434028549142,0.686482740837633,
-4.03100680972357));
#43792=CARTESIAN_POINT('Ctrl Pts',(-23.3449297031862,3.75908802705159,-1.60920218070417));
#43793=CARTESIAN_POINT('Ctrl Pts',(-23.146456551458,3.39055631091931,2.28569515815013));
#43794=CARTESIAN_POINT('Ctrl Pts',(-22.9479833997299,-0.0817518254726031,
4.08822591016416));
#43795=CARTESIAN_POINT('Ctrl Pts',(-22.7495102480017,-3.47922286584052,
2.14832090324472));
#43796=CARTESIAN_POINT('Ctrl Pts',(-22.5510370962737,-3.69175052183031,
-1.75819581903476));
#43797=CARTESIAN_POINT('Ctrl Pts',(-22.3525639445455,-0.524783142673121,
-4.05522836677194));
#43798=CARTESIAN_POINT('Ctrl Pts',(-22.1540907928174,3.12258019355253,-2.64003170214662));
#43799=CARTESIAN_POINT('Ctrl Pts',(-21.9556176410892,3.91147728224659,1.19189761471977));
#43800=CARTESIAN_POINT('Ctrl Pts',(-21.7571444893611,1.11973749494471,3.93274235056415));
#43801=CARTESIAN_POINT('Ctrl Pts',(-21.558671337633,-2.69703019780661,3.07348378320514));
#43802=CARTESIAN_POINT('Ctrl Pts',(-21.3601981859049,-4.04488778700894,
-0.599297291844044));
#43803=CARTESIAN_POINT('Ctrl Pts',(-21.1617250341767,-1.68998211713108,
-3.72347081327125));
#43804=CARTESIAN_POINT('Ctrl Pts',(-20.9632518824486,2.2119636738382,-3.43911197246119));
#43805=CARTESIAN_POINT('Ctrl Pts',(-20.7647787307204,4.08903800898778,-0.00652798276298151));
#43806=CARTESIAN_POINT('Ctrl Pts',(-20.5663055789923,2.22293317528866,3.43203184013592));
#43807=CARTESIAN_POINT('Ctrl Pts',(-20.3678324272642,-1.67808479377233,
3.72884779501869));
#43808=CARTESIAN_POINT('Ctrl Pts',(-20.1693592755361,-4.04295366619892,
0.612209201559777));
#43809=CARTESIAN_POINT('Ctrl Pts',(-19.970886123808,-2.70682980863068,-3.06485674063472));
#43810=CARTESIAN_POINT('Ctrl Pts',(-19.7724129720798,1.10717489304186,-3.93629752555922));
#43811=CARTESIAN_POINT('Ctrl Pts',(-19.5739398203517,3.90765172170437,-1.2043805359465));
#43812=CARTESIAN_POINT('Ctrl Pts',(-19.3754666686235,3.13099366151297,2.63004812599908));
#43813=CARTESIAN_POINT('Ctrl Pts',(-19.1769935168954,-0.511832486578831,
4.05688328143518));
#43814=CARTESIAN_POINT('Ctrl Pts',(-18.9785203651673,-3.6861179418498,1.76997428576766));
#43815=CARTESIAN_POINT('Ctrl Pts',(-18.7800472134392,-3.48606452731231,
-2.13720110539941));
#43816=CARTESIAN_POINT('Ctrl Pts',(-18.581574061711,-0.0948047480465078,
-4.08794404478016));
#43817=CARTESIAN_POINT('Ctrl Pts',(-18.3831009099829,3.38324100807146,-2.29650924988542));
#43818=CARTESIAN_POINT('Ctrl Pts',(-18.1846277582548,3.7642069041412,1.59719154653454));
#43819=CARTESIAN_POINT('Ctrl Pts',(-17.9861546065267,0.69934988542084,4.02879438433728));
#43820=CARTESIAN_POINT('Ctrl Pts',(-17.7876814547985,-3.00570463625504,
2.77236615422654));
#43821=CARTESIAN_POINT('Ctrl Pts',(-17.5892083030704,-3.95928290424672,
-1.02193607316972));
#43822=CARTESIAN_POINT('Ctrl Pts',(-17.3907351513422,-1.28846216734285,
-3.88073958116644));
#43823=CARTESIAN_POINT('Ctrl Pts',(-17.1922619996141,2.56184008429538,-3.18704405931314));
#43824=CARTESIAN_POINT('Ctrl Pts',(-16.993788847886,4.06698770142585,0.424129095861815));
#43825=CARTESIAN_POINT('Ctrl Pts',(-16.7953156961579,1.84914139908685,3.64704682444424));
#43826=CARTESIAN_POINT('Ctrl Pts',(-16.5968425444297,-2.06144230263648,
3.53139208902191));
#43827=CARTESIAN_POINT('Ctrl Pts',(-16.3983693927016,-4.08494452748146,
0.183037321071356));
#43828=CARTESIAN_POINT('Ctrl Pts',(-16.1998962409735,-2.36901483030422,
-3.33287311299191));
#43829=CARTESIAN_POINT('Ctrl Pts',(-16.0014230892454,1.515553784877,-3.79781136691262));
#43830=CARTESIAN_POINT('Ctrl Pts',(-15.8029499375172,4.0127571213907,-0.786164574522354));
#43831=CARTESIAN_POINT('Ctrl Pts',(-15.6044767857891,2.83661018984044,2.94515145355875));
#43832=CARTESIAN_POINT('Ctrl Pts',(-15.406003634061,-0.936220888302868,
3.98042270391114));
#43833=CARTESIAN_POINT('Ctrl Pts',(-15.2075304823328,-3.85201847376804,
1.37194319534574));
#43834=CARTESIAN_POINT('Ctrl Pts',(-15.0090573306047,-3.24160884928891,
-2.49243786717293));
#43835=CARTESIAN_POINT('Ctrl Pts',(-14.8105841788766,0.336228001726943,
-4.07519633690948));
#43836=CARTESIAN_POINT('Ctrl Pts',(-14.6121110271485,3.60627567365431,-1.92744655415262));
#43837=CARTESIAN_POINT('Ctrl Pts',(-14.4136378754203,3.57507352861307,1.98472257973647));
#43838=CARTESIAN_POINT('Ctrl Pts',(-14.2151647236922,0.271184573130672,
4.08004085528584));
#43839=CARTESIAN_POINT('Ctrl Pts',(-14.016691571964,-3.28095163337376,2.44041611881411));
#43840=CARTESIAN_POINT('Ctrl Pts',(-13.8182184202359,-3.8296455189581,-1.43320956340302));
#43841=CARTESIAN_POINT('Ctrl Pts',(-13.6197452685078,-0.87261280108946,
-3.99484935296447));
#43842=CARTESIAN_POINT('Ctrl Pts',(-13.4212721167797,2.88322541878955,-2.8995319687756));
#43843=CARTESIAN_POINT('Ctrl Pts',(-13.2227989650515,3.99970707045215,0.850069293693618));
#43844=CARTESIAN_POINT('Ctrl Pts',(-13.0243258133234,1.45478470613215,3.82150178755809));
#43845=CARTESIAN_POINT('Ctrl Pts',(-12.8258526615953,-2.42187382576178,
3.29466259662437));
#43846=CARTESIAN_POINT('Ctrl Pts',(-12.6273795098671,-4.081505361515,-0.248170178365596));
#43847=CARTESIAN_POINT('Ctrl Pts',(-12.428906358139,-2.00485324982196,-3.56382349453281));
#43848=CARTESIAN_POINT('Ctrl Pts',(-12.2304332064109,1.90707769880952,-3.61708848443179));
#43849=CARTESIAN_POINT('Ctrl Pts',(-12.0319600546828,4.07323531398969,-0.359205415289091));
#43850=CARTESIAN_POINT('Ctrl Pts',(-11.8334869029546,2.51067983243849,3.22750077188098));
#43851=CARTESIAN_POINT('Ctrl Pts',(-11.6350137512265,-1.35019726602492,
3.85969452111492));
#43852=CARTESIAN_POINT('Ctrl Pts',(-11.4365405994984,-3.97507942658069,
0.958654268170109));
#43853=CARTESIAN_POINT('Ctrl Pts',(-11.2380674477702,-2.96110216069169,
-2.81995539813183));
#43854=CARTESIAN_POINT('Ctrl Pts',(-11.0395942960421,0.763521448022078,
-4.0171270146606));
#43855=CARTESIAN_POINT('Ctrl Pts',(-10.841121144314,3.78920374757617,-1.53694808398346));
#43856=CARTESIAN_POINT('Ctrl Pts',(-10.6426479925859,3.34618057086064,2.35018085276441));
#43857=CARTESIAN_POINT('Ctrl Pts',(-10.4441748408577,-0.15999667302688,
4.08591183435546));
#43858=CARTESIAN_POINT('Ctrl Pts',(-10.2457016891296,-3.51971007572659,
2.08132540375945));
#43859=CARTESIAN_POINT('Ctrl Pts',(-10.0472285374015,-3.65741737163835,
-1.82854385321865));
#43860=CARTESIAN_POINT('Ctrl Pts',(-9.84875538567335,-0.44705881753592,
-4.06453107592611));
#43861=CARTESIAN_POINT('Ctrl Pts',(-9.65028223394518,3.17254544408314,-2.5797732184696));
#43862=CARTESIAN_POINT('Ctrl Pts',(-9.45180908221709,3.88794436634965,1.26655558807174));
#43863=CARTESIAN_POINT('Ctrl Pts',(-9.25333593048893,1.04424886841893,3.95345655778733));
#43864=CARTESIAN_POINT('Ctrl Pts',(-9.05486277876082,-2.75537088425535,
3.02129206527667));
#43865=CARTESIAN_POINT('Ctrl Pts',(-8.85638962703267,-4.03267441640854,
-0.676617694676789));
#43866=CARTESIAN_POINT('Ctrl Pts',(-8.65791647530455,-1.61839502928575,
-3.75513940922157));
#43867=CARTESIAN_POINT('Ctrl Pts',(-8.45944332357642,2.27739236712315,-3.39613875742363));
#43868=CARTESIAN_POINT('Ctrl Pts',(-8.26097017184829,4.08841370139886,0.0717485868838491));
#43869=CARTESIAN_POINT('Ctrl Pts',(-8.06249702012017,2.15682736925666,3.47395598025235));
#43870=CARTESIAN_POINT('Ctrl Pts',(-7.86402386839202,-1.74915765070859,
3.69604139133657));
#43871=CARTESIAN_POINT('Ctrl Pts',(-7.66555071666391,-4.05393219848626,
0.534703827910877));
#43872=CARTESIAN_POINT('Ctrl Pts',(-7.46707756493577,-2.64766406973572,
-3.11611126684138));
#43873=CARTESIAN_POINT('Ctrl Pts',(-7.26860441320765,1.18232351825157,-3.91438188628729));
#43874=CARTESIAN_POINT('Ctrl Pts',(-7.07013126147951,3.92999082586276,-1.12935670279306));
#43875=CARTESIAN_POINT('Ctrl Pts',(-6.87165810975138,3.08007362562457,2.68950198256747));
#43876=CARTESIAN_POINT('Ctrl Pts',(-6.67318495802325,-0.5893985429476,4.04634202843412));
#43877=CARTESIAN_POINT('Ctrl Pts',(-6.47471180629512,-3.71932465123805,
1.69908757638346));
#43878=CARTESIAN_POINT('Ctrl Pts',(-6.276238654567,-3.44451386881323,-2.20354229844359));
#43879=CARTESIAN_POINT('Ctrl Pts',(-6.07776550283886,-0.0165329441350717,
-4.08900979642298));
#43880=CARTESIAN_POINT('Ctrl Pts',(-5.87929235111075,3.42658253592967,-2.23132395185361));
#43881=CARTESIAN_POINT('Ctrl Pts',(-5.68081919938261,3.73294253930156,1.66895609635091));
#43882=CARTESIAN_POINT('Ctrl Pts',(-5.48234604765447,0.622099591660842,
4.04144362220976));
#43883=CARTESIAN_POINT('Ctrl Pts',(-5.28387289592636,-3.05822454649594,
2.71432073964919));
#43884=CARTESIAN_POINT('Ctrl Pts',(-5.08539974419822,-3.93899475710348,
-1.09754032054403));
#43885=CARTESIAN_POINT('Ctrl Pts',(-4.88692659247009,-1.21393809962148,
-3.90469316899007));
#43886=CARTESIAN_POINT('Ctrl Pts',(-4.68845344074195,2.62237939808053,-3.13741944155749));
#43887=CARTESIAN_POINT('Ctrl Pts',(-4.48998028901383,4.05812347799734,0.501904649608686));
#43888=CARTESIAN_POINT('Ctrl Pts',(-4.29150713728569,1.77898811457109,3.68177616742087));
#43889=CARTESIAN_POINT('Ctrl Pts',(-4.09303398555757,-2.12866507747974,
3.49128335716317));
#43890=CARTESIAN_POINT('Ctrl Pts',(-3.89456083382944,-4.08769982950793,
0.104806765260383));
#43891=CARTESIAN_POINT('Ctrl Pts',(-3.69608768210131,-2.30478044879331,
-3.37761181920371));
#43892=CARTESIAN_POINT('Ctrl Pts',(-3.49761453037318,1.58797661938014,-3.76810362629895));
#43893=CARTESIAN_POINT('Ctrl Pts',(-3.29914137864505,4.02707108416311,-0.709205347471504));
#43894=CARTESIAN_POINT('Ctrl Pts',(-3.10066822691692,2.77971231822834,2.99891222297364));
#43895=CARTESIAN_POINT('Ctrl Pts',(-2.9021950751888,-1.01224582434915,3.96177158871793));
#43896=CARTESIAN_POINT('Ctrl Pts',(-2.70372192346066,-3.87757478920465,
1.29795347349033));
#43897=CARTESIAN_POINT('Ctrl Pts',(-2.50524877173254,-3.19330391076162,
-2.55403411582895));
#43898=CARTESIAN_POINT('Ctrl Pts',(-2.3067756200044,0.414178958109714,-4.06801385371924));
#43899=CARTESIAN_POINT('Ctrl Pts',(-2.10830246827628,3.64250733110373,-1.85805828889993));
#43900=CARTESIAN_POINT('Ctrl Pts',(-1.90982931654813,3.53643331957866,2.05279348420085));
#43901=CARTESIAN_POINT('Ctrl Pts',(-1.71135616482002,0.193016622173817,
4.08448847232805));
#43902=CARTESIAN_POINT('Ctrl Pts',(-1.51288301309187,-3.32703776432247,
2.37715485179658));
#43903=CARTESIAN_POINT('Ctrl Pts',(-1.31440986136375,-3.80156352397709,
-1.50624211154998));
#43904=CARTESIAN_POINT('Ctrl Pts',(-1.11593670963562,-0.795874796086486,
-4.0108496983533));
#43905=CARTESIAN_POINT('Ctrl Pts',(-0.917463557907495,2.93799978076921,
-2.84375397442605));
#43906=CARTESIAN_POINT('Ctrl Pts',(-0.718990406179355,3.98308848377519,
0.926375809981952));
#43907=CARTESIAN_POINT('Ctrl Pts',(-0.520517254451229,1.38062350887484,
3.84884745468318));
#43908=CARTESIAN_POINT('Ctrl Pts',(-0.3220441027231,-2.4830778832256,3.247317855149));
#43909=CARTESIAN_POINT('Ctrl Pts',(-0.123570950994979,-4.07876466704636,
-0.325509284212394));
#43910=CARTESIAN_POINT('Ctrl Pts',(0.0749022007331616,-1.93063333093837,
-3.60315675180159));
#43911=CARTESIAN_POINT('Ctrl Pts',(0.207217635218578,0.664553028381002,
-3.58469246392335));
#43912=CARTESIAN_POINT('Ctrl Pts',(0.273375352461288,1.67175183450892,-3.02875982108454));
#43913=CARTESIAN_POINT('Ctrl Pts',(-54.567,1.87158653173864,-2.62360084935085));
#43914=CARTESIAN_POINT('Ctrl Pts',(-54.5008422827573,2.74405176481089,-2.00121418560501));
#43915=CARTESIAN_POINT('Ctrl Pts',(-54.3685268482719,3.80418105204897,0.171604520928937));
#43916=CARTESIAN_POINT('Ctrl Pts',(-54.1700536965438,1.91525344717721,3.29560071974874));
#43917=CARTESIAN_POINT('Ctrl Pts',(-53.9715805448156,-1.72862424686986,
3.39318099076701));
#43918=CARTESIAN_POINT('Ctrl Pts',(-53.7731073930875,-3.78919857444914,
0.38936181408417));
#43919=CARTESIAN_POINT('Ctrl Pts',(-53.5746342413594,-2.38153781877884,
-2.97336043415339));
#43920=CARTESIAN_POINT('Ctrl Pts',(-53.3761610896312,1.20646915281294,-3.61292403145259));
#43921=CARTESIAN_POINT('Ctrl Pts',(-53.1776879379031,3.68992516100066,-0.945826390348501));
#43922=CARTESIAN_POINT('Ctrl Pts',(-52.979214786175,2.79562367813024,2.58745046926129));
#43923=CARTESIAN_POINT('Ctrl Pts',(-52.7807416344468,-0.657876967632621,
3.75194409668105));
#43924=CARTESIAN_POINT('Ctrl Pts',(-52.5822684827187,-3.50912696830559,
1.48193681013123));
#43925=CARTESIAN_POINT('Ctrl Pts',(-52.3837953309905,-3.14806834501192,
-2.14471257454507));
#43926=CARTESIAN_POINT('Ctrl Pts',(-52.1853221792625,0.0947938145258543,
-3.80802701948498));
#43927=CARTESIAN_POINT('Ctrl Pts',(-51.9868490275343,3.25087740482292,-1.98541860413584));
#43928=CARTESIAN_POINT('Ctrl Pts',(-51.7883758758062,3.43105052559699,1.65468502690142));
#43929=CARTESIAN_POINT('Ctrl Pts',(-51.5899027240781,0.47037738033959,3.78005636351393));
#43930=CARTESIAN_POINT('Ctrl Pts',(-51.3914295723498,-2.92088733377907,
2.44509787357924));
#43931=CARTESIAN_POINT('Ctrl Pts',(-51.1929564206218,-3.63831927756816,
-1.12814835451757));
#43932=CARTESIAN_POINT('Ctrl Pts',(-50.9944832688937,-1.02516800960105,
-3.66866668622662));
#43933=CARTESIAN_POINT('Ctrl Pts',(-50.7960101171655,2.52644049755188,-2.85082162384731));
#43934=CARTESIAN_POINT('Ctrl Pts',(-50.5975369654374,3.76529981837076,0.576717135381059));
#43935=CARTESIAN_POINT('Ctrl Pts',(-50.3990638137093,1.55733573647028,3.47631854666922));
#43936=CARTESIAN_POINT('Ctrl Pts',(-50.2005906619811,-2.07624156883218,
3.19363527997699));
#43937=CARTESIAN_POINT('Ctrl Pts',(-50.002117510253,-3.80918988593932,-0.0125593633857515));
#43938=CARTESIAN_POINT('Ctrl Pts',(-49.8036443585249,-2.05513705304844,
-3.20725692790933));
#43939=CARTESIAN_POINT('Ctrl Pts',(-49.6051712067968,1.58022531640166,-3.46597364026232));
#43940=CARTESIAN_POINT('Ctrl Pts',(-49.4066980550686,3.7690209209745,-0.551875545371135));
#43941=CARTESIAN_POINT('Ctrl Pts',(-49.2082249033405,2.50758677259566,2.8674193792543));
#43942=CARTESIAN_POINT('Ctrl Pts',(-49.0097517516124,-1.04933754975442,
3.66182687025214));
#43943=CARTESIAN_POINT('Ctrl Pts',(-48.8112785998842,-3.64567934673634,
1.10413197621781));
#43944=CARTESIAN_POINT('Ctrl Pts',(-48.6128054481561,-2.90470049343726,
-2.46430524964014));
#43945=CARTESIAN_POINT('Ctrl Pts',(-48.414332296428,0.495293598847041,-3.77687298849846));
#43946=CARTESIAN_POINT('Ctrl Pts',(-48.2158591446999,3.44188699455041,-1.63202305036004));
#43947=CARTESIAN_POINT('Ctrl Pts',(-48.0173859929717,3.23771493607145,2.00681023340388));
#43948=CARTESIAN_POINT('Ctrl Pts',(-47.8189128412436,0.0696802094731201,
3.80857322216686));
#43949=CARTESIAN_POINT('Ctrl Pts',(-47.6204396895155,-3.1621410380659,2.12389956814232));
#43950=CARTESIAN_POINT('Ctrl Pts',(-47.4219665377873,-3.4992813272385,-1.50503007046925));
#43951=CARTESIAN_POINT('Ctrl Pts',(-47.2234933860592,-0.633116354570043,
-3.75622802845598));
#43952=CARTESIAN_POINT('Ctrl Pts',(-47.025020234331,2.81261475191178,-2.56890707841041));
#43953=CARTESIAN_POINT('Ctrl Pts',(-46.826547082603,3.68362756861194,0.970037760059602));
#43954=CARTESIAN_POINT('Ctrl Pts',(-46.6280739308748,1.18258124809755,3.62099253131349));
#43955=CARTESIAN_POINT('Ctrl Pts',(-46.4296007791467,-2.40102128334473,
2.95722540857222));
#43956=CARTESIAN_POINT('Ctrl Pts',(-46.2311276274185,-3.7866856122015,-0.41363920815822));
#43957=CARTESIAN_POINT('Ctrl Pts',(-46.0326544756905,-1.70594961134342,
-3.40585103076117));
#43958=CARTESIAN_POINT('Ctrl Pts',(-45.8341813239623,1.93644344289748,-3.28028537061014));
#43959=CARTESIAN_POINT('Ctrl Pts',(-45.6357081722341,3.80618123172504,-0.151887298493708));
#43960=CARTESIAN_POINT('Ctrl Pts',(-45.4372350205061,2.19167204898115,3.11555114705157));
#43961=CARTESIAN_POINT('Ctrl Pts',(-45.2387618687778,-1.42913327008184,
3.53095786105198));
#43962=CARTESIAN_POINT('Ctrl Pts',(-45.0402887170499,-3.74168420894083,
0.714062042642285));
#43963=CARTESIAN_POINT('Ctrl Pts',(-44.8418155653216,-2.62902991455607,
-2.75649905288374));
#43964=CARTESIAN_POINT('Ctrl Pts',(-44.6433424135935,0.890285797212397,
-3.70371118197161));
#43965=CARTESIAN_POINT('Ctrl Pts',(-44.4448692618654,3.5946178274591,-1.26047927182198));
#43966=CARTESIAN_POINT('Ctrl Pts',(-44.2463961101372,3.00837184347797,2.33661810562801));
#43967=CARTESIAN_POINT('Ctrl Pts',(-44.0479229584092,-0.331792003801605,
3.79473311135223));
#43968=CARTESIAN_POINT('Ctrl Pts',(-43.8494498066809,-3.36822746452892,
1.77908096144407));
#43969=CARTESIAN_POINT('Ctrl Pts',(-43.6509766549529,-3.32132673384483,
-1.86517399918272));
#43970=CARTESIAN_POINT('Ctrl Pts',(-43.4525035032247,-0.234023586811988,
-3.80201502903332));
#43971=CARTESIAN_POINT('Ctrl Pts',(-43.2540303514966,3.06750897389918,-2.25842290442415));
#43972=CARTESIAN_POINT('Ctrl Pts',(-43.0555571997685,3.5609884751578,1.35257029391188));
#43973=CARTESIAN_POINT('Ctrl Pts',(-42.8570840480403,0.794674878034206,
3.72539624179777));
#43974=CARTESIAN_POINT('Ctrl Pts',(-42.6586108963122,-2.69909844015994,
2.68792725543417));
#43975=CARTESIAN_POINT('Ctrl Pts',(-42.460137744584,-3.72206834843915,-0.810118836793174));
#43976=CARTESIAN_POINT('Ctrl Pts',(-42.261664592856,-1.33778973609199,-3.56656752945834));
#43977=CARTESIAN_POINT('Ctrl Pts',(-42.0631914411278,2.27112573740255,-3.05811595677589));
#43978=CARTESIAN_POINT('Ctrl Pts',(-41.8647182893997,3.80101173467418,0.249790138013328));
#43979=CARTESIAN_POINT('Ctrl Pts',(-41.6662451376716,1.8513830112441,3.32903383369054));
#43980=CARTESIAN_POINT('Ctrl Pts',(-41.4677719859434,-1.7930351237828,3.36081989476688));
#43981=CARTESIAN_POINT('Ctrl Pts',(-41.2692988342154,-3.7960765561218,0.316050787441167));
#43982=CARTESIAN_POINT('Ctrl Pts',(-41.0708256824871,-2.32412101924758,
-3.0180369129736));
#43983=CARTESIAN_POINT('Ctrl Pts',(-40.8723525307591,1.27537683100426,-3.58935917109407));
#43984=CARTESIAN_POINT('Ctrl Pts',(-40.6738793790308,3.70737171949489,-0.874917283901245));
#43985=CARTESIAN_POINT('Ctrl Pts',(-40.4754062273029,2.74557164665491,2.64043967044588));
#43986=CARTESIAN_POINT('Ctrl Pts',(-40.2769330755746,-0.72957424780644,
3.73869051101015));
#43987=CARTESIAN_POINT('Ctrl Pts',(-40.0784599238466,-3.5368547126692,1.41447660342944));
#43988=CARTESIAN_POINT('Ctrl Pts',(-39.8799867721184,-3.10643456075901,
-2.20457470726251));
#43989=CARTESIAN_POINT('Ctrl Pts',(-39.6815136203903,0.16767183512014,-3.80551855545168));
#43990=CARTESIAN_POINT('Ctrl Pts',(-39.4830404686621,3.28828840795416,-1.92282205788625));
#43991=CARTESIAN_POINT('Ctrl Pts',(-39.284567316934,3.39874644404531,1.72006044349292));
#43992=CARTESIAN_POINT('Ctrl Pts',(-39.0860941652058,0.397930664244868,
3.78836858114853));
#43993=CARTESIAN_POINT('Ctrl Pts',(-38.8876210134778,-2.96715802516744,
2.38873576895062));
#43994=CARTESIAN_POINT('Ctrl Pts',(-38.6891478617496,-3.61605672415252,
-1.19758886429816));
#43995=CARTESIAN_POINT('Ctrl Pts',(-38.4906747100216,-0.954751856070833,
-3.68761904397796));
#43996=CARTESIAN_POINT('Ctrl Pts',(-38.2922015582933,2.58055008692402,-2.80193621787794));
#43997=CARTESIAN_POINT('Ctrl Pts',(-38.0937284065653,3.7535699214344,0.648689575284357));
#43998=CARTESIAN_POINT('Ctrl Pts',(-37.895255254837,1.4905041270395,3.50549322741577));
#43999=CARTESIAN_POINT('Ctrl Pts',(-37.696782103109,-2.13699603728643,3.1533051322068));
#44000=CARTESIAN_POINT('Ctrl Pts',(-37.4983089513808,-3.80825147287653,
-0.0854753737247307));
#44001=CARTESIAN_POINT('Ctrl Pts',(-37.2998357996528,-1.99336480079335,
-3.24601018038109));
#44002=CARTESIAN_POINT('Ctrl Pts',(-37.1013626479246,1.64628397471009,-3.43508870260906));
#44003=CARTESIAN_POINT('Ctrl Pts',(-36.9028894961965,3.77889469710683,-0.479625049760291));
#44004=CARTESIAN_POINT('Ctrl Pts',(-36.7044163444683,2.45223703403194,2.9148960271512));
#44005=CARTESIAN_POINT('Ctrl Pts',(-36.5059431927402,-1.11924265385457,
3.64106868954325));
#44006=CARTESIAN_POINT('Ctrl Pts',(-36.3074700410121,-3.66614742275361,
1.03414138047787));
#44007=CARTESIAN_POINT('Ctrl Pts',(-36.108996889284,-2.85699469533783,-2.51945760650804));
#44008=CARTESIAN_POINT('Ctrl Pts',(-35.9105237375558,0.567502522785501,
-3.76669964382771));
#44009=CARTESIAN_POINT('Ctrl Pts',(-35.7120505858277,3.472497692532,-1.5658368674736));
#44010=CARTESIAN_POINT('Ctrl Pts',(-35.5135774340996,3.19870582288421,2.06842122857658));
#44011=CARTESIAN_POINT('Ctrl Pts',(-35.3151042823714,-0.00323906886257519,
3.80920921302736));
#44012=CARTESIAN_POINT('Ctrl Pts',(-35.1166311306433,-3.2022188585325,2.062978357191));
#44013=CARTESIAN_POINT('Ctrl Pts',(-34.9181579789152,-3.46982972988793,
-1.57174010757682));
#44014=CARTESIAN_POINT('Ctrl Pts',(-34.719684827187,-0.56109586298945,-3.76765932015034));
#44015=CARTESIAN_POINT('Ctrl Pts',(-34.521211675459,2.86127528031798,-2.51459521402966));
#44016=CARTESIAN_POINT('Ctrl Pts',(-34.3227385237307,3.66438340819573,1.04037471995407));
#44017=CARTESIAN_POINT('Ctrl Pts',(-34.1242653720026,1.1130488505117,3.64296686459735));
#44018=CARTESIAN_POINT('Ctrl Pts',(-33.9257922202745,-2.45719070682964,
2.91072141409131));
#44019=CARTESIAN_POINT('Ctrl Pts',(-33.7273190685464,-3.77807355790493,
-0.486050934819766));
#44020=CARTESIAN_POINT('Ctrl Pts',(-33.5288459168183,-1.64043970914924,
-3.43788348854727));
#44021=CARTESIAN_POINT('Ctrl Pts',(-33.3303727650901,1.99888224657508,-3.24261546972602));
#44022=CARTESIAN_POINT('Ctrl Pts',(-33.131899613362,3.80839132946346,-0.0789987458582374));
#44023=CARTESIAN_POINT('Ctrl Pts',(-32.9334264616339,2.13163027743554,3.15693485528285));
#44024=CARTESIAN_POINT('Ctrl Pts',(-32.7349533099058,-1.49646358995037,
3.50295333170919));
#44025=CARTESIAN_POINT('Ctrl Pts',(-32.5364801581776,-3.75466768753454,
0.642305127150348));
#44026=CARTESIAN_POINT('Ctrl Pts',(-32.3380070064495,-2.5757812413192,-2.8063207794277));
#44027=CARTESIAN_POINT('Ctrl Pts',(-32.1395338547213,0.961021826073252,
-3.68599001219353));
#44028=CARTESIAN_POINT('Ctrl Pts',(-31.9410607029932,3.61808817488804,-1.19143748426638));
#44029=CARTESIAN_POINT('Ctrl Pts',(-31.7425875512651,2.96309132998079,2.39377841296397));
#44030=CARTESIAN_POINT('Ctrl Pts',(-31.5441143995369,-0.404372779207533,
3.78768636183299));
#44031=CARTESIAN_POINT('Ctrl Pts',(-31.3456412478088,-3.40166675051695,
1.7142778767187));
#44032=CARTESIAN_POINT('Ctrl Pts',(-31.1471680960807,-3.28501360470175,
-1.92841150616356));
#44033=CARTESIAN_POINT('Ctrl Pts',(-30.9486949443525,-0.16119973612574,
-3.80579820343283));
#44034=CARTESIAN_POINT('Ctrl Pts',(-30.7502217926245,3.11017927930475,-2.19928856014008));
#44035=CARTESIAN_POINT('Ctrl Pts',(-30.5517486408963,3.53444406784637,1.42048951120562));
#44036=CARTESIAN_POINT('Ctrl Pts',(-30.3532754891682,0.723214987379329,
3.73992585517541));
#44037=CARTESIAN_POINT('Ctrl Pts',(-30.1548023374401,-2.75005814095598,
2.63576659466299));
#44038=CARTESIAN_POINT('Ctrl Pts',(-29.9563291857119,-3.70587842984033,
-0.881220961747833));
#44039=CARTESIAN_POINT('Ctrl Pts',(-29.7578560339838,-1.26927074168613,
-3.59152295057115));
#44040=CARTESIAN_POINT('Ctrl Pts',(-29.5593828822556,2.32925028389996,-3.01408003130834));
#44041=CARTESIAN_POINT('Ctrl Pts',(-29.3609097305275,3.79553357470212,0.322506129381382));
#44042=CARTESIAN_POINT('Ctrl Pts',(-29.1624365787994,1.78731695127927,3.36386436050109));
#44043=CARTESIAN_POINT('Ctrl Pts',(-28.9639634270713,-1.85704185655309,
3.32588046435669));
#44044=CARTESIAN_POINT('Ctrl Pts',(-28.7654902753432,-3.80143104369453,
0.243325584793488));
#44045=CARTESIAN_POINT('Ctrl Pts',(-28.567017123615,-2.26592166709176,-3.06197392522923));
#44046=CARTESIAN_POINT('Ctrl Pts',(-28.3685439718869,1.34385328587831,-3.56428725921659));
#44047=CARTESIAN_POINT('Ctrl Pts',(-28.1700708201588,3.72344069482658,-0.803787728376804));
#44048=CARTESIAN_POINT('Ctrl Pts',(-27.9715976684306,2.69452331250517,2.69251359115343));
#44049=CARTESIAN_POINT('Ctrl Pts',(-27.7731245167025,-0.801009325330438,
3.72403939035468));
#44050=CARTESIAN_POINT('Ctrl Pts',(-27.5746513649744,-3.56328357475288,
1.3465123415981));
#44051=CARTESIAN_POINT('Ctrl Pts',(-27.3761782132462,-3.063663750215,-2.26363639876154));
#44052=CARTESIAN_POINT('Ctrl Pts',(-27.1777050615181,0.240489146638442,
-3.80161153861474));
#44053=CARTESIAN_POINT('Ctrl Pts',(-26.9792319097899,3.32449393969521,-1.85952288641721));
#44054=CARTESIAN_POINT('Ctrl Pts',(-26.7807587580619,3.36519699902431,1.78480656597217));
#44055=CARTESIAN_POINT('Ctrl Pts',(-26.5822856063336,0.325338009741355,
3.79529188595517));
#44056=CARTESIAN_POINT('Ctrl Pts',(-26.3838124546056,-3.01234126348658,
2.33149853795273));
#44057=CARTESIAN_POINT('Ctrl Pts',(-26.1853393028774,-3.59246899472296,
-1.26659063715707));
#44058=CARTESIAN_POINT('Ctrl Pts',(-25.9868661511494,-0.883985791987881,
-3.70521989087602));
#44059=CARTESIAN_POINT('Ctrl Pts',(-25.7883929994212,2.63371395382021,-2.75202400600582));
#44060=CARTESIAN_POINT('Ctrl Pts',(-25.5899198476931,3.74046442819159,0.720424306650572));
#44061=CARTESIAN_POINT('Ctrl Pts',(-25.3914466959649,1.42312627862469,3.53338321092794));
#44062=CARTESIAN_POINT('Ctrl Pts',(-25.1929735442368,-2.19696734278675,
3.11181937376001));
#44063=CARTESIAN_POINT('Ctrl Pts',(-24.9945003925087,-3.80591742039044,
-0.158360062352112));
#44064=CARTESIAN_POINT('Ctrl Pts',(-24.7960272407805,-1.93086202407817,
-3.28357384021623));
#44065=CARTESIAN_POINT('Ctrl Pts',(-24.5975540890524,1.71173930615894,-3.40294488170616));
#44066=CARTESIAN_POINT('Ctrl Pts',(-24.3990809373243,3.78738359192001,-0.407198781720557));
#44067=CARTESIAN_POINT('Ctrl Pts',(-24.2006077855962,2.3959886047388,2.9613044298318));
#44068=CARTESIAN_POINT('Ctrl Pts',(-24.002134633868,-1.18873758023125,3.6189761377392));
#44069=CARTESIAN_POINT('Ctrl Pts',(-23.8036614821399,-3.6852719367642,0.963771794709725));
#44070=CARTESIAN_POINT('Ctrl Pts',(-23.6051883304118,-2.80824187180781,
-2.57368663780286));
#44071=CARTESIAN_POINT('Ctrl Pts',(-23.4067151786836,0.639503469586358,
-3.7551458869885));
#44072=CARTESIAN_POINT('Ctrl Pts',(-23.2082420269555,3.50183579684358,-1.4990768399667));
#44073=CARTESIAN_POINT('Ctrl Pts',(-23.0097688752274,3.15852445469445,2.12927419307066));
#44074=CARTESIAN_POINT('Ctrl Pts',(-22.8112957234992,-0.0761571601507046,
3.80844921288671));
#44075=CARTESIAN_POINT('Ctrl Pts',(-22.6128225717711,-3.24112313654785,
2.00130111025649));
#44076=CARTESIAN_POINT('Ctrl Pts',(-22.414349420043,-3.43910651661478,-1.63787413666537));
#44077=CARTESIAN_POINT('Ctrl Pts',(-22.2158762683149,-0.488869742173803,
-3.77770984795902));
#44078=CARTESIAN_POINT('Ctrl Pts',(-22.0174031165867,2.90888721456023,-2.45936180606832));
#44079=CARTESIAN_POINT('Ctrl Pts',(-21.8189299648586,3.64379633223308,1.11033040550302));
#44080=CARTESIAN_POINT('Ctrl Pts',(-21.6204568131305,1.04310854511736,3.66360613102486));
#44081=CARTESIAN_POINT('Ctrl Pts',(-21.4219836614024,-2.51245962421763,
2.8631507045309));
#44082=CARTESIAN_POINT('Ctrl Pts',(-21.2235105096742,-3.76807692313431,
-0.558284534554106));
#44083=CARTESIAN_POINT('Ctrl Pts',(-21.0250373579461,-1.57432862205077,
-3.46865603800252));
#44084=CARTESIAN_POINT('Ctrl Pts',(-20.8265642062179,2.06058850407911,-3.20375722192501));
#44085=CARTESIAN_POINT('Ctrl Pts',(-20.6280910544898,3.80920573593449,-0.00608124192798155));
#44086=CARTESIAN_POINT('Ctrl Pts',(-20.4296179027617,2.07080731049629,3.19716161664916));
#44087=CARTESIAN_POINT('Ctrl Pts',(-20.2311447510336,-1.56324548898088,
3.47366504737583));
#44088=CARTESIAN_POINT('Ctrl Pts',(-20.0326715993054,-3.76627516338849,
0.570312821022469));
#44089=CARTESIAN_POINT('Ctrl Pts',(-19.8341984475773,-2.52158860117499,
-2.8551140514179));
#44090=CARTESIAN_POINT('Ctrl Pts',(-19.6357252958492,1.03140566167082,-3.66691800852612));
#44091=CARTESIAN_POINT('Ctrl Pts',(-19.437252144121,3.64023257295061,-1.12195906120018));
#44092=CARTESIAN_POINT('Ctrl Pts',(-19.2387789923929,2.9167249089872,2.45006145340748));
#44093=CARTESIAN_POINT('Ctrl Pts',(-19.0403058406648,-0.476805360925414,
3.77925150895946));
#44094=CARTESIAN_POINT('Ctrl Pts',(-18.8418326889367,-3.43385940080828,
1.64884654703227));
#44095=CARTESIAN_POINT('Ctrl Pts',(-18.6433595372085,-3.24749659066223,
-1.9909422929399));
#44096=CARTESIAN_POINT('Ctrl Pts',(-18.4448863854804,-0.088316809298266,
-3.80818663688835));
#44097=CARTESIAN_POINT('Ctrl Pts',(-18.2464132337523,3.15170977273075,-2.13934822519688));
#44098=CARTESIAN_POINT('Ctrl Pts',(-18.0479400820241,3.50660436488545,1.48788815048238));
#44099=CARTESIAN_POINT('Ctrl Pts',(-17.849466930296,0.651490054412623,3.7530848683691));
#44100=CARTESIAN_POINT('Ctrl Pts',(-17.6509937785678,-2.80001000621206,
2.58263998367796));
#44101=CARTESIAN_POINT('Ctrl Pts',(-17.4525206268398,-3.68833038868658,
-0.952000138692661));
#44102=CARTESIAN_POINT('Ctrl Pts',(-17.2540474751116,-1.2002865876007,-3.61516215788525));
#44103=CARTESIAN_POINT('Ctrl Pts',(-17.0555743233835,2.38652121163826,-2.96893951211207));
#44104=CARTESIAN_POINT('Ctrl Pts',(-16.8571011716553,3.78866443554566,0.395103929379446));
#44105=CARTESIAN_POINT('Ctrl Pts',(-16.6586280199273,1.72259587914657,3.39746210535554));
#44106=CARTESIAN_POINT('Ctrl Pts',(-16.4601548681991,-1.92036802451838,
3.28972217224905));
#44107=CARTESIAN_POINT('Ctrl Pts',(-16.261681716471,-3.80539239079082,0.170511208695819));
#44108=CARTESIAN_POINT('Ctrl Pts',(-16.0632085647428,-2.20689190471551,
-3.10478879170239));
#44109=CARTESIAN_POINT('Ctrl Pts',(-15.8647354130147,1.41183724821851,-3.53790911481943));
#44110=CARTESIAN_POINT('Ctrl Pts',(-15.6662622612865,3.73814511142124,-0.732363602411441));
#44111=CARTESIAN_POINT('Ctrl Pts',(-15.4677891095585,2.64248749510294,2.7436007651268));
#44112=CARTESIAN_POINT('Ctrl Pts',(-15.2693159578303,-0.872150850636688,
3.70802349155361));
#44113=CARTESIAN_POINT('Ctrl Pts',(-15.0708428061022,-3.58840657214504,
1.27805461274778));
#44114=CARTESIAN_POINT('Ctrl Pts',(-14.8723696543741,-3.01977017460503,
-2.32186851754045));
#44115=CARTESIAN_POINT('Ctrl Pts',(-14.6738965026459,0.313218324198597,
-3.79631131515394));
#44116=CARTESIAN_POINT('Ctrl Pts',(-14.4754233509178,3.35948111786941,-1.79554224090064));
#44117=CARTESIAN_POINT('Ctrl Pts',(-14.2769501991897,3.33041428366469,1.84889859628423));
#44118=CARTESIAN_POINT('Ctrl Pts',(-14.0784770474615,0.252626126046346,
3.80082430015101));
#44119=CARTESIAN_POINT('Ctrl Pts',(-13.8800038957334,-3.05642054529701,
2.27340686426031));
#44120=CARTESIAN_POINT('Ctrl Pts',(-13.6815307440053,-3.5675647047904,-1.33512823253552));
#44121=CARTESIAN_POINT('Ctrl Pts',(-13.4830575922771,-0.812895766645905,
-3.72146285655909));
#44122=CARTESIAN_POINT('Ctrl Pts',(-13.284584440549,2.68591262275001,-2.70110323814768));
#44123=CARTESIAN_POINT('Ctrl Pts',(-13.0861112888209,3.72598813738973,0.791895018427709));
#44124=CARTESIAN_POINT('Ctrl Pts',(-12.8876381370928,1.35522688587594,3.55997828757123));
#44125=CARTESIAN_POINT('Ctrl Pts',(-12.6891649853646,-2.25613350830277,
3.06919320227532));
#44126=CARTESIAN_POINT('Ctrl Pts',(-12.4906918336365,-3.80218858326998,
-0.231186715515902));
#44127=CARTESIAN_POINT('Ctrl Pts',(-12.2922186819084,-1.86765162909789,
-3.31993414279675));
#44128=CARTESIAN_POINT('Ctrl Pts',(-12.0937455301802,1.77656732297672,-3.36955395669975));
#44129=CARTESIAN_POINT('Ctrl Pts',(-11.8952723784521,3.7944844943374,-0.334623284325299));
#44130=CARTESIAN_POINT('Ctrl Pts',(-11.696799226724,2.33886209856671,3.00662757987545));
#44131=CARTESIAN_POINT('Ctrl Pts',(-11.4983260749959,-1.2577968605525,3.59555731114996));
#44132=CARTESIAN_POINT('Ctrl Pts',(-11.2998529232677,-3.70304588004417,
0.893049007875609));
#44133=CARTESIAN_POINT('Ctrl Pts',(-11.1013797715396,-2.75845988968622,
-2.62697246981617));
#44134=CARTESIAN_POINT('Ctrl Pts',(-10.9029066198115,0.711270052496804,
-3.74221595216));
#44135=CARTESIAN_POINT('Ctrl Pts',(-10.7044334680833,3.52989055571641,-1.43176743392344));
#44136=CARTESIAN_POINT('Ctrl Pts',(-10.5059603163552,3.11718555708669,2.18934682562397));
#44137=CARTESIAN_POINT('Ctrl Pts',(-10.3074871646271,-0.14904734152245,
3.80629350026567));
#44138=CARTESIAN_POINT('Ctrl Pts',(-10.1090140128989,-3.27883961455344,
1.9388904306883));
#44139=CARTESIAN_POINT('Ctrl Pts',(-9.91054086117081,-3.40712294679801,
-1.70340792107529));
#44140=CARTESIAN_POINT('Ctrl Pts',(-9.71206770944269,-0.416464461400303,
-3.78637592858529));
#44141=CARTESIAN_POINT('Ctrl Pts',(-9.51359455771457,2.95543310591665,-2.40322709635013));
#44142=CARTESIAN_POINT('Ctrl Pts',(-9.31512140598641,3.62187388543242,1.17987917949349));
#44143=CARTESIAN_POINT('Ctrl Pts',(-9.11664825425831,0.972785963491132,
3.6829027667608));
#44144=CARTESIAN_POINT('Ctrl Pts',(-8.91817510253016,-2.56680778067166,
2.81453071350504));
#44145=CARTESIAN_POINT('Ctrl Pts',(-8.71970195080203,-3.75669937143538,
-0.630313535343016));
#44146=CARTESIAN_POINT('Ctrl Pts',(-8.52122879907392,-1.50764057830064,
-3.49815740166747));
#44147=CARTESIAN_POINT('Ctrl Pts',(-8.32275564734576,2.12153960142961,-3.1637248678963));
#44148=CARTESIAN_POINT('Ctrl Pts',(-8.12428249561765,3.80862415267616,0.0668384906429997));
#44149=CARTESIAN_POINT('Ctrl Pts',(-7.92580934388952,2.00922543843686,3.23621668893135));
#44150=CARTESIAN_POINT('Ctrl Pts',(-7.72733619216139,-1.62945449308302,
3.44310374156095));
#44151=CARTESIAN_POINT('Ctrl Pts',(-7.52886304043325,-3.77650238261931,
0.498111507848026));
#44152=CARTESIAN_POINT('Ctrl Pts',(-7.33038988870514,-2.46647185452845,
-2.90286098719837));
#44153=CARTESIAN_POINT('Ctrl Pts',(-7.131916736977,1.10141150988432,-3.6465021604372));
#44154=CARTESIAN_POINT('Ctrl Pts',(-6.93344358524887,3.6610429062145,-1.05206946493042));
#44155=CARTESIAN_POINT('Ctrl Pts',(-6.73497043352074,2.86928957276539,2.50544660046798));
#44156=CARTESIAN_POINT('Ctrl Pts',(-6.5364972817926,-0.549063204013273,
3.76943164391853));
#44157=CARTESIAN_POINT('Ctrl Pts',(-6.3380241300645,-3.4647936175104,1.58281095152196));
#44158=CARTESIAN_POINT('Ctrl Pts',(-6.13955097833634,-3.20878944087819,
-2.05274344336138));
#44159=CARTESIAN_POINT('Ctrl Pts',(-5.94107782660823,-0.0154015163207855,
-3.80917945408937));
#44160=CARTESIAN_POINT('Ctrl Pts',(-5.74260467488009,3.19208523418617,-2.07862386640746));
#44161=CARTESIAN_POINT('Ctrl Pts',(-5.54413152315197,3.47747956887825,1.55474151163881));
#44162=CARTESIAN_POINT('Ctrl Pts',(-5.34565837142383,0.57952636479995,3.76486845887453));
#44163=CARTESIAN_POINT('Ctrl Pts',(-5.14718521969571,-2.84893572979317,
2.52856689224015));
#44164=CARTESIAN_POINT('Ctrl Pts',(-4.94871206796758,-3.6694306557177,-1.02243042868416));
#44165=CARTESIAN_POINT('Ctrl Pts',(-4.75023891623944,-1.13086255544314,
-3.6374764880366));
#44166=CARTESIAN_POINT('Ctrl Pts',(-4.55176576451131,2.44291753292778,-2.92271094241356));
#44167=CARTESIAN_POINT('Ctrl Pts',(-4.35329261278319,3.78040683298627,0.467556932945782));
#44168=CARTESIAN_POINT('Ctrl Pts',(-4.15481946105505,1.65724351676092,3.42981475460483));
#44169=CARTESIAN_POINT('Ctrl Pts',(-3.95634630932692,-1.98299042591341,
3.25235827122354));
#44170=CARTESIAN_POINT('Ctrl Pts',(-3.7578731575988,-3.80795913442598,0.0976343410155721));
#44171=CARTESIAN_POINT('Ctrl Pts',(-3.55940000587067,-2.14705338671746,
-3.1464658159672));
#44172=CARTESIAN_POINT('Ctrl Pts',(-3.36092685414253,1.47930384451711,-3.51023441585637));
#44173=CARTESIAN_POINT('Ctrl Pts',(-3.16245370241441,3.75147950180274,-0.66067106043193));
#44174=CARTESIAN_POINT('Ctrl Pts',(-2.96398055068628,2.58948341482026,2.79368243000086));
#44175=CARTESIAN_POINT('Ctrl Pts',(-2.76550739895815,-0.942973039578199,
3.69064876067085));
#44176=CARTESIAN_POINT('Ctrl Pts',(-2.56703424723002,-3.61221394765404,
1.20912835863316));
#44177=CARTESIAN_POINT('Ctrl Pts',(-2.36856109550189,-2.97477097222353,
-2.37924944263257));
#44178=CARTESIAN_POINT('Ctrl Pts',(-2.17008794377376,0.385834726766185,
-3.78962036336862));
#44179=CARTESIAN_POINT('Ctrl Pts',(-1.97161479204564,3.39323327108378,-1.73090254387995));
#44180=CARTESIAN_POINT('Ctrl Pts',(-1.77314164031749,3.29441840747864,1.91231108576612));
#44181=CARTESIAN_POINT('Ctrl Pts',(-1.57466848858938,0.179807578872998,
3.80496754565549));
#44182=CARTESIAN_POINT('Ctrl Pts',(-1.37619533686123,-3.09935278363057,
2.21447486591351));
#44183=CARTESIAN_POINT('Ctrl Pts',(-1.1777221851331,-3.54140449397235,-1.40316281688026));
#44184=CARTESIAN_POINT('Ctrl Pts',(-0.979249033404971,-0.741409307439854,
-3.73636822239283));
#44185=CARTESIAN_POINT('Ctrl Pts',(-0.780775881676852,2.73693851524025,
-2.64914239661277));
#44186=CARTESIAN_POINT('Ctrl Pts',(-0.58230272994871,3.7105068394527,0.862979517739233));
#44187=CARTESIAN_POINT('Ctrl Pts',(-0.383829578220586,1.28614089123481,
3.58545256094235));
#44188=CARTESIAN_POINT('Ctrl Pts',(-0.185356426492456,-2.31314908170687,
3.02508848610542));
#44189=CARTESIAN_POINT('Ctrl Pts',(0.0131167252356648,-3.79963544752816,
-0.303233139382865));
#44190=CARTESIAN_POINT('Ctrl Pts',(0.211589876963805,-1.79851093142999,
-3.35657563863806));
#44191=CARTESIAN_POINT('Ctrl Pts',(0.343905311449222,0.619074511407565,
-3.33937494959071));
#44192=CARTESIAN_POINT('Ctrl Pts',(0.410063028691932,1.55734592416918,-2.82148741534915));
#44193=CARTESIAN_POINT('',(0.,1.9005636551884,-3.44330463255532));
#44194=CARTESIAN_POINT('Ctrl Pts',(3.88578058618805E-15,-3.22782252806242,
-0.0460729527342081));
#44195=CARTESIAN_POINT('Ctrl Pts',(4.73555566111894E-15,-3.23478024525164,
-0.117033456944334));
#44196=CARTESIAN_POINT('Ctrl Pts',(8.03715949314405E-15,-3.23920846232986,
-0.188120433263497));
#44197=CARTESIAN_POINT('Ctrl Pts',(8.04911692853238E-15,-3.24105490347623,
-0.259217854133791));
#44198=CARTESIAN_POINT('Ctrl Pts',(8.01201932747411E-15,-3.24372057254421,
-0.361859736871017));
#44199=CARTESIAN_POINT('Ctrl Pts',(4.97629665024702E-15,-3.24100807231244,
-0.464523059622032));
#44200=CARTESIAN_POINT('Ctrl Pts',(6.38378239159465E-15,-3.2331868370857,
-0.566908454444247));
#44201=CARTESIAN_POINT('Ctrl Pts',(7.27024547280655E-15,-3.228260864428,
-0.631392853752119));
#44202=CARTESIAN_POINT('Ctrl Pts',(5.05793373854853E-15,-3.22130734435912,
-0.695767345230122));
#44203=CARTESIAN_POINT('Ctrl Pts',(7.88258347483861E-15,-3.21238338916487,
-0.759959157634126));
#44204=CARTESIAN_POINT('Ctrl Pts',(9.67722682972631E-15,-3.20671354745568,
-0.800743474389926));
#44205=CARTESIAN_POINT('Ctrl Pts',(1.25174804097342E-15,-3.20024814307216,
-0.841454073881994));
#44206=CARTESIAN_POINT('Ctrl Pts',(3.60822483003176E-15,-3.19300024485765,
-0.88207239965212));
#44207=CARTESIAN_POINT('Ctrl Pts',(4.76004307358495E-15,-3.18945755713433,
-0.901926161361911));
#44208=CARTESIAN_POINT('Ctrl Pts',(-5.96198962811207E-15,-3.18572918223731,
-0.921750470983836));
#44209=CARTESIAN_POINT('Ctrl Pts',(-6.21724893790088E-15,-3.18181839014642,
-0.94153660922562));
#44210=CARTESIAN_POINT('Ctrl Pts',(-7.56115075084112E-15,-3.16122865892243,
-1.04570764641999));
#44211=CARTESIAN_POINT('Ctrl Pts',(-1.36291055847055E-14,-3.13557667564011,
-1.14887664494683));
#44212=CARTESIAN_POINT('Ctrl Pts',(-1.38222766565832E-14,-3.10513969145318,
-1.25072883011327));
#44213=CARTESIAN_POINT('Ctrl Pts',(-1.40056860216817E-14,-3.07624080979882,
-1.34743401704262));
#44214=CARTESIAN_POINT('Ctrl Pts',(-1.64583170794824E-14,-3.04302772710359,
-1.44295273829285));
#44215=CARTESIAN_POINT('Ctrl Pts',(-1.72639680329212E-14,-3.00569631404638,
-1.5370185109656));
#44216=CARTESIAN_POINT('Ctrl Pts',(-1.76197494419365E-14,-2.98921048642918,
-1.57855865064864));
#44217=CARTESIAN_POINT('Ctrl Pts',(-1.1736135794431E-14,-2.97192100533988,
-1.6198154265008));
#44218=CARTESIAN_POINT('Ctrl Pts',(-1.15463194561016E-14,-2.95384239793326,
-1.66076562713157));
#44219=CARTESIAN_POINT('Ctrl Pts',(-1.14658401134983E-14,-2.94617733362913,
-1.67812791140723));
#44220=CARTESIAN_POINT('Ctrl Pts',(-4.64785945728864E-15,-2.93837039609743,
-1.69543508116795));
#44221=CARTESIAN_POINT('Ctrl Pts',(-4.94049245958195E-15,-2.93042261817385,
-1.71268534926259));
#44222=CARTESIAN_POINT('Ctrl Pts',(-5.23462946247637E-15,-2.92243399228478,
-1.73002427589328));
#44223=CARTESIAN_POINT('Ctrl Pts',(1.03171797750105E-14,-2.91430646083762,
-1.7472982787437));
#44224=CARTESIAN_POINT('Ctrl Pts',(1.02140518265514E-14,-2.90604442083402,
-1.76449962417443));
#44225=CARTESIAN_POINT('Ctrl Pts',(9.61224345561637E-15,-2.85783086757843,
-1.8648789473961));
#44226=CARTESIAN_POINT('Ctrl Pts',(-2.77542935576527E-15,-2.80501130232528,
-1.96284871204576));
#44227=CARTESIAN_POINT('Ctrl Pts',(-3.5527136788005E-15,-2.74787578078745,
-2.0580753587026));
#44228=CARTESIAN_POINT('Ctrl Pts',(-4.34191077239773E-15,-2.6898645920853,
-2.15476146254826));
#44229=CARTESIAN_POINT('Ctrl Pts',(5.09332848748403E-16,-2.62740391916529,
-2.24862058887149));
#44230=CARTESIAN_POINT('Ctrl Pts',(4.44089209850063E-16,-2.56074398374797,
-2.33929898513567));
#44231=CARTESIAN_POINT('Ctrl Pts',(3.79051966108302E-16,-2.49429492387408,
-2.42969052459493));
#44232=CARTESIAN_POINT('Ctrl Pts',(-2.96184435993952E-15,-2.42367274126983,
-2.51692230201439));
#44233=CARTESIAN_POINT('Ctrl Pts',(-3.63598040564739E-15,-2.34907746971602,
-2.60062625818245));
#44234=CARTESIAN_POINT('Ctrl Pts',(-4.06933452632506E-15,-2.3011254746896,
-2.65443357875728));
#44235=CARTESIAN_POINT('Ctrl Pts',(8.7125606268543E-15,-2.25153073404126,
-2.70678271127021));
#44236=CARTESIAN_POINT('Ctrl Pts',(8.90953977261688E-15,-2.20033702360218,
-2.75756942711216));
#44237=CARTESIAN_POINT('Ctrl Pts',(8.96738040010056E-15,-2.1853045879423,
-2.77248235355806));
#44238=CARTESIAN_POINT('Ctrl Pts',(1.50797221210893E-14,-2.17013423829745,
-2.78726052273648));
#44239=CARTESIAN_POINT('Ctrl Pts',(1.47659662275146E-14,-2.15482697246737,
-2.8019011892954));
#44240=CARTESIAN_POINT('Ctrl Pts',(1.45500706766672E-14,-2.14429403697187,
-2.81197543757644));
#44241=CARTESIAN_POINT('Ctrl Pts',(1.23807284931021E-14,-2.13369842184177,
-2.82198247550803));
#44242=CARTESIAN_POINT('Ctrl Pts',(1.20459198171829E-14,-2.12304672770763,
-2.8319158305085));
#44243=CARTESIAN_POINT('Ctrl Pts',(9.38291716989935E-15,-2.03832523833943,
-2.91092379107002));
#44244=CARTESIAN_POINT('Ctrl Pts',(1.9478406166701E-14,-1.94994848897902,
-2.98537883656598));
#44245=CARTESIAN_POINT('Ctrl Pts',(1.82354131794682E-14,-1.8581826378662,
-3.05491944709952));
#44246=CARTESIAN_POINT('Ctrl Pts',(1.75414617624024E-14,-1.80695061719345,
-3.09374332279233));
#44247=CARTESIAN_POINT('Ctrl Pts',(9.03667999584674E-15,-1.75466135551627,
-3.13103514774695));
#44248=CARTESIAN_POINT('Ctrl Pts',(9.79771819231701E-15,-1.7013548304381,
-3.16672887515648));
#44249=CARTESIAN_POINT('Ctrl Pts',(1.1086530334245E-14,-1.60913652867894,
-3.22847769334214));
#44250=CARTESIAN_POINT('Ctrl Pts',(1.24667943883469E-15,-1.51387584437434,
-3.28544626009495));
#44251=CARTESIAN_POINT('Ctrl Pts',(8.04911692853238E-16,-1.41595740939529,
-3.33768974045716));
#44252=CARTESIAN_POINT('Ctrl Pts',(3.54779253464665E-16,-1.31618492849516,
-3.39092242996767));
#44253=CARTESIAN_POINT('Ctrl Pts',(-6.5005489732385E-16,-1.21365248296573,
-3.43924970726973));
#44254=CARTESIAN_POINT('Ctrl Pts',(-1.41553435639707E-15,-1.10873353044733,
-3.48268730307254));
#44255=CARTESIAN_POINT('Ctrl Pts',(-1.66306814692421E-15,-1.07480579312247,
-3.49673375802702));
#44256=CARTESIAN_POINT('Ctrl Pts',(-3.87488146035897E-15,-1.04062828456681,
-3.51026855829844));
#44257=CARTESIAN_POINT('Ctrl Pts',(-3.7470027081099E-15,-1.0062130758155,
-3.52329122523045));
#44258=CARTESIAN_POINT('Ctrl Pts',(-3.6710391470737E-15,-0.985769477762066,
-3.53102705418518));
#44259=CARTESIAN_POINT('Ctrl Pts',(2.81238272578907E-15,-0.965237687041626,
-3.53858360073728));
#44260=CARTESIAN_POINT('Ctrl Pts',(3.24740234702858E-15,-0.94464775261746,
-3.54595111805713));
#44261=CARTESIAN_POINT('Ctrl Pts',(5.51531576371633E-15,-0.837305034612612,
-3.58436063009195));
#44262=CARTESIAN_POINT('Ctrl Pts',(-7.28433529689487E-15,-0.728255688796531,
-3.61768684857147));
#44263=CARTESIAN_POINT('Ctrl Pts',(-4.71844785465692E-15,-0.617912626483569,
-3.64600997081435));
#44264=CARTESIAN_POINT('Ctrl Pts',(-2.07020700373184E-15,-0.504028049778018,
-3.67524213747709));
#44265=CARTESIAN_POINT('Ctrl Pts',(2.29237048498726E-14,-0.388764785234235,
-3.6991452721761));
#44266=CARTESIAN_POINT('Ctrl Pts',(2.96290769696839E-14,-0.272542535137063,
-3.71776398168584));
#44267=CARTESIAN_POINT('Ctrl Pts',(3.63968142768708E-14,-0.155239327521797,
-3.73655585970681));
#44268=CARTESIAN_POINT('Ctrl Pts',(8.3301433537551E-15,-0.0369584030558998,
-3.74996479689759));
#44269=CARTESIAN_POINT('Ctrl Pts',(4.26048085699904E-15,0.0818921458507452,
-3.75798853653923));
#44270=CARTESIAN_POINT('Ctrl Pts',(1.60898338187825E-15,0.159326559784058,
-3.76321622444156));
#44271=CARTESIAN_POINT('Ctrl Pts',(1.07137817972841E-14,0.237003225132265,
-3.7661569708165));
#44272=CARTESIAN_POINT('Ctrl Pts',(9.54791801177635E-15,0.314812005453235,
-3.7667985805642));
#44273=CARTESIAN_POINT('Ctrl Pts',(9.15843836140906E-15,0.340805553697568,
-3.76701292287701));
#44274=CARTESIAN_POINT('Ctrl Pts',(-7.73214731083006E-15,0.366813855211389,
-3.76697059853649));
#44275=CARTESIAN_POINT('Ctrl Pts',(-8.49320613838245E-15,0.392832820121125,
-3.76667091810736));
#44276=CARTESIAN_POINT('Ctrl Pts',(-8.96735202530461E-15,0.409042848501716,
-3.76648421474395));
#44277=CARTESIAN_POINT('Ctrl Pts',(4.5316324873848E-15,0.425257015824682,
-3.76619761904271));
#44278=CARTESIAN_POINT('Ctrl Pts',(4.30211422042248E-15,0.441474332786118,
-3.76581094080709));
#44279=CARTESIAN_POINT('Ctrl Pts',(4.06095880866029E-15,0.458513907898259,
-3.76540465702687));
#44280=CARTESIAN_POINT('Ctrl Pts',(5.76983320580279E-15,0.475547853604313,
-3.76488808759821));
#44281=CARTESIAN_POINT('Ctrl Pts',(5.49560397189452E-15,0.492571736322231,
-3.76426150826196));
#44282=CARTESIAN_POINT('Ctrl Pts',(3.52265966451042E-15,0.615050189910908,
-3.75975357846556));
#44283=CARTESIAN_POINT('Ctrl Pts',(1.24955252947878E-14,0.737059901364942,
-3.74955414102053));
#44284=CARTESIAN_POINT('Ctrl Pts',(1.08801856413265E-14,0.858161021353391,
-3.73371021053407));
#44285=CARTESIAN_POINT('Ctrl Pts',(9.26218533919139E-15,0.979461608700677,
-3.71784018328675));
#44286=CARTESIAN_POINT('Ctrl Pts',(2.79921898071093E-16,1.09985150954407,
-3.69630721138857));
#44287=CARTESIAN_POINT('Ctrl Pts',(-1.64451785522601E-15,1.21890371977399,
-3.66910833103822));
#44288=CARTESIAN_POINT('Ctrl Pts',(-3.53245504367798E-15,1.33569776057229,
-3.64242535610503));
#44289=CARTESIAN_POINT('Ctrl Pts',(-9.40696534928934E-15,1.45120524179666,
-3.61028936199537));
#44290=CARTESIAN_POINT('Ctrl Pts',(-1.27606258892854E-14,1.56502432695476,
-3.57264846725809));
#44291=CARTESIAN_POINT('Ctrl Pts',(-1.61097959296429E-14,1.6786910101167,
-3.5350579730972));
#44292=CARTESIAN_POINT('Ctrl Pts',(-1.6278834459108E-16,1.79067467066081,
-3.49197745284248));
#44293=CARTESIAN_POINT('Ctrl Pts',(0.,1.9005636551884,-3.44330463255532));
#44294=CARTESIAN_POINT('Ctrl Pts',(0.,1.9005636551884,-3.44330463255532));
#44295=CARTESIAN_POINT('Ctrl Pts',(-0.0661577172427078,0.755510062327915,
-4.07532749258862));
#44296=CARTESIAN_POINT('Ctrl Pts',(-0.132315434485407,-0.719684033813403,
-4.08582323535868));
#44297=CARTESIAN_POINT('Ctrl Pts',(-0.198473151728118,-1.86430524457212,
-3.47002820603423));
#44298=CARTESIAN_POINT('Ctrl Pts',(-0.264630868970832,-3.00892645533091,
-2.85423317670973));
#44299=CARTESIAN_POINT('Ctrl Pts',(-0.330788586213552,-3.82297478070687,
-1.61214737529056));
#44300=CARTESIAN_POINT('Ctrl Pts',(-0.396946303456264,-3.92765100675819,
-0.314131446729717));
#44301=CARTESIAN_POINT('Ctrl Pts',(-0.402243028292546,-3.9360316037528,
-0.210209584047015));
#44302=CARTESIAN_POINT('Ctrl Pts',(-0.407539753128828,-3.93986516986432,
-0.105929212740074));
#44303=CARTESIAN_POINT('Ctrl Pts',(-0.41283647796511,-3.93929521061115,
-0.00160796147817999));
#44304=CARTESIAN_POINT('Origin',(4.677207419323,0.,0.));
#44305=CARTESIAN_POINT('',(4.53252091062694,6.5,-3.75277674973257));
#44306=CARTESIAN_POINT('',(4.53252091062694,-1.37874781034238E-15,-7.50555349946513));
#44307=CARTESIAN_POINT('Ctrl Pts',(4.53252091062694,6.5,-3.75277674973257));
#44308=CARTESIAN_POINT('Ctrl Pts',(5.61727242352805,3.24999999999854,-5.6291651245997));
#44309=CARTESIAN_POINT('Ctrl Pts',(4.53252091062694,-1.37874781034238E-15,
-7.50555349946513));
#44310=CARTESIAN_POINT('',(4.53252091062694,6.5,3.75277674973257));
#44311=CARTESIAN_POINT('Ctrl Pts',(4.53252091062694,6.5,3.75277674973257));
#44312=CARTESIAN_POINT('Ctrl Pts',(5.61727242352805,6.5,-1.69086966650411E-12));
#44313=CARTESIAN_POINT('Ctrl Pts',(4.53252091062694,6.5,-3.75277674973257));
#44314=CARTESIAN_POINT('',(4.53252091062694,4.5958260344746E-16,7.50555349946513));
#44315=CARTESIAN_POINT('Ctrl Pts',(4.53252091062694,4.5958260344746E-16,
7.50555349946513));
#44316=CARTESIAN_POINT('Ctrl Pts',(5.61727242352806,3.25000000000146,5.62916512459801));
#44317=CARTESIAN_POINT('Ctrl Pts',(4.53252091062694,6.5,3.75277674973257));
#44318=CARTESIAN_POINT('',(4.53252091062694,-6.5,3.75277674973257));
#44319=CARTESIAN_POINT('Ctrl Pts',(4.53252091062694,-6.5,3.75277674973257));
#44320=CARTESIAN_POINT('Ctrl Pts',(5.61727242352806,-3.24999999999854,5.6291651245997));
#44321=CARTESIAN_POINT('Ctrl Pts',(4.53252091062694,4.5958260344746E-16,
7.50555349946513));
#44322=CARTESIAN_POINT('',(5.11383749436743,-6.5,-8.18813977659918E-16));
#44323=CARTESIAN_POINT('Ctrl Pts',(5.11383749436743,-6.5,-8.41607535874056E-16));
#44324=CARTESIAN_POINT('Ctrl Pts',(5.11383749436757,-6.5,1.74166975080303));
#44325=CARTESIAN_POINT('Ctrl Pts',(4.53252091062694,-6.5,3.75277674973257));
#44326=CARTESIAN_POINT('',(5.3,-6.17797863635533,-7.56584176221328E-16));
#44327=CARTESIAN_POINT('',(4.677207419323,-7.25527674973257,-8.8851514484882E-16));
#44328=CARTESIAN_POINT('Origin',(5.3,0.,0.));
#44329=CARTESIAN_POINT('',(4.53252091062694,-6.5,-3.75277674973257));
#44330=CARTESIAN_POINT('Ctrl Pts',(4.53252091062694,-6.5,-3.75277674973257));
#44331=CARTESIAN_POINT('Ctrl Pts',(5.11383749436729,-6.5,-1.74166975080219));
#44332=CARTESIAN_POINT('Ctrl Pts',(5.11383749436743,-6.5,-8.41607535874056E-16));
#44333=CARTESIAN_POINT('Ctrl Pts',(4.53252091062694,-1.37874781034238E-15,
-7.50555349946513));
#44334=CARTESIAN_POINT('Ctrl Pts',(5.61727242352805,-3.25000000000146,-5.629165124598));
#44335=CARTESIAN_POINT('Ctrl Pts',(4.53252091062694,-6.5,-3.75277674973257));
#44336=CARTESIAN_POINT('Origin',(0.,4.5958260344746E-16,7.50555349946513));
#44337=CARTESIAN_POINT('',(0.,4.5958260344746E-16,7.50555349946513));
#44338=CARTESIAN_POINT('',(0.,4.5958260344746E-16,7.50555349946513));
#44339=CARTESIAN_POINT('',(0.,-6.5,3.75277674973257));
#44340=CARTESIAN_POINT('',(0.,4.5958260344746E-16,7.50555349946513));
#44341=CARTESIAN_POINT('',(0.,-6.5,3.75277674973257));
#44342=CARTESIAN_POINT('Origin',(0.,6.5,3.75277674973257));
#44343=CARTESIAN_POINT('',(0.,6.5,3.75277674973257));
#44344=CARTESIAN_POINT('',(0.,6.5,3.75277674973257));
#44345=CARTESIAN_POINT('',(0.,6.5,3.75277674973257));
#44346=CARTESIAN_POINT('Origin',(0.,6.5,-3.75277674973257));
#44347=CARTESIAN_POINT('',(0.,6.5,-3.75277674973257));
#44348=CARTESIAN_POINT('',(0.,6.5,-3.75277674973257));
#44349=CARTESIAN_POINT('',(0.,6.5,-3.75277674973257));
#44350=CARTESIAN_POINT('Origin',(0.,0.,-1.11022302462516E-15));
#44351=CARTESIAN_POINT('',(0.,-1.37874781034238E-15,-7.50555349946513));
#44352=CARTESIAN_POINT('',(0.,-1.37874781034238E-15,-7.50555349946513));
#44353=CARTESIAN_POINT('',(0.,-6.5,-3.75277674973257));
#44354=CARTESIAN_POINT('',(0.,-6.5,-3.75277674973257));
#44355=CARTESIAN_POINT('',(0.,-6.5,3.75277674973257));
#44356=CARTESIAN_POINT('Origin',(0.,0.,0.));
#44357=CARTESIAN_POINT('Origin',(0.,-1.37874781034238E-15,-7.50555349946513));
#44358=CARTESIAN_POINT('',(0.,-1.37874781034238E-15,-7.50555349946513));
#44359=CARTESIAN_POINT('Origin',(0.,-6.5,-3.75277674973257));
#44360=CARTESIAN_POINT('',(0.,-6.5,-3.75277674973257));
#44361=CARTESIAN_POINT('Origin',(0.,-6.5,3.75277674973257));
#44362=CARTESIAN_POINT('Origin',(5.3,0.,-1.11022302462516E-15));
#44363=CARTESIAN_POINT('Origin',(-55.,3.5,0.));
#44364=CARTESIAN_POINT('',(-55.,-3.5,-4.28626379701573E-16));
#44365=CARTESIAN_POINT('Origin',(-55.,0.,0.));
#44366=CARTESIAN_POINT('Origin',(-54.75,0.,0.));
#44367=CARTESIAN_POINT('',(-54.75,-3.75,-4.59242549680257E-16));
#44368=CARTESIAN_POINT('Origin',(-27.25,0.,0.));
#44369=CARTESIAN_POINT('',(0.,0.,0.));
#44370=CARTESIAN_POINT('Origin',(-54.75,0.,0.));
#44371=CARTESIAN_POINT('',(-109.162836477965,-3.93801241551785,0.0024295370903759));
#44372=CARTESIAN_POINT('',(-109.346163522035,-3.93703449438079,0.00416483169883862));
#44373=CARTESIAN_POINT('',(-54.75,-3.933,-4.81653586104654E-16));
#44374=CARTESIAN_POINT('',(-109.567,1.75072546723784,3.52562190316238));
#44375=CARTESIAN_POINT('Ctrl Pts',(-109.162836477965,-3.93801241551785,
0.0024295370903759));
#44376=CARTESIAN_POINT('Ctrl Pts',(-109.169080619277,-3.93882021117856,
0.125415509802713));
#44377=CARTESIAN_POINT('Ctrl Pts',(-109.17532476059,-3.93356178335156,0.248326376778116));
#44378=CARTESIAN_POINT('Ctrl Pts',(-109.181568901902,-3.92201207588029,
0.370636940123473));
#44379=CARTESIAN_POINT('Ctrl Pts',(-109.247860079135,-3.79939414225896,
1.66915195227987));
#44380=CARTESIAN_POINT('Ctrl Pts',(-109.314151256367,-2.96768025587816,
2.90000618657311));
#44381=CARTESIAN_POINT('Ctrl Pts',(-109.3804424336,-1.80872165918533,3.49932265847817));
#44382=CARTESIAN_POINT('Ctrl Pts',(-109.442628289066,-0.721535780237971,
4.06152428253533));
#44383=CARTESIAN_POINT('Ctrl Pts',(-109.504814144533,0.653618210307921,
4.06798663531537));
#44384=CARTESIAN_POINT('Ctrl Pts',(-109.567,1.75275645914439,3.52838181187396));
#44385=CARTESIAN_POINT('',(-109.567,-1.74869447532986,3.5228619944515));
#44386=CARTESIAN_POINT('Origin',(-109.567,0.,0.));
#44387=CARTESIAN_POINT('Ctrl Pts',(-109.567,-1.74869447532986,3.5228619944515));
#44388=CARTESIAN_POINT('Ctrl Pts',(-109.500708822768,-2.92256775530673,
2.9401693648038));
#44389=CARTESIAN_POINT('Ctrl Pts',(-109.434417645535,-3.77202868504578,
1.72965923743315));
#44390=CARTESIAN_POINT('Ctrl Pts',(-109.368126468303,-3.91512454167974,
0.435231098702328));
#44391=CARTESIAN_POINT('Ctrl Pts',(-109.360805486213,-3.93092758285667,
0.292278663473746));
#44392=CARTESIAN_POINT('Ctrl Pts',(-109.353484504124,-3.93811560100482,
0.148302741059963));
#44393=CARTESIAN_POINT('Ctrl Pts',(-109.346163522035,-3.93703449438079,
0.00416483169883862));
#44394=CARTESIAN_POINT('Origin',(-54.75,0.,0.));
#44395=CARTESIAN_POINT('',(-107.912836477965,-3.92799297266711,0.00241250680657806));
#44396=CARTESIAN_POINT('',(-108.096163522035,-3.92761091684392,0.00216275952952855));
#44397=CARTESIAN_POINT('',(-54.75,-3.933,-4.81653586104654E-16));
#44398=CARTESIAN_POINT('Ctrl Pts',(-107.912836477965,-3.92799297266711,
0.00241250680657806));
#44399=CARTESIAN_POINT('Ctrl Pts',(-107.938000222549,-3.93076900949478,
0.501336754196634));
#44400=CARTESIAN_POINT('Ctrl Pts',(-107.963163967133,-3.8426867303152,0.9993162840385));
#44401=CARTESIAN_POINT('Ctrl Pts',(-107.988327711717,-3.65926185083382,
1.45927211247531));
#44402=CARTESIAN_POINT('Ctrl Pts',(-108.05461888895,-3.17604874421936,2.67097624657527));
#44403=CARTESIAN_POINT('Ctrl Pts',(-108.120910066182,-2.03115577349008,
3.61879500835267));
#44404=CARTESIAN_POINT('Ctrl Pts',(-108.187201243415,-0.75054268099906,
3.8673339509319));
#44405=CARTESIAN_POINT('Ctrl Pts',(-108.253492420647,0.530070411491968,
4.11587289351112));
#44406=CARTESIAN_POINT('Ctrl Pts',(-108.31978359788,1.94640362574474,3.66513201689217));
#44407=CARTESIAN_POINT('Ctrl Pts',(-108.386074775112,2.84778208996043,2.72211706459808));
#44408=CARTESIAN_POINT('Ctrl Pts',(-108.452365952345,3.74916055417613,1.77910211230399));
#44409=CARTESIAN_POINT('Ctrl Pts',(-108.518657129577,4.13558426835475,0.343813084334772));
#44410=CARTESIAN_POINT('Ctrl Pts',(-108.58494830681,3.82954854862144,-0.924253883068262));
#44411=CARTESIAN_POINT('Ctrl Pts',(-108.651239484042,3.52351282888813,-2.1923208504713));
#44412=CARTESIAN_POINT('Ctrl Pts',(-108.717530661275,2.52501767524288,-3.29316575730815));
#44413=CARTESIAN_POINT('Ctrl Pts',(-108.783821838507,1.29273734961643,-3.72129137538108));
#44414=CARTESIAN_POINT('Ctrl Pts',(-108.85011301574,0.0604570239899871,
-4.149416993454));
#44415=CARTESIAN_POINT('Ctrl Pts',(-108.916404192972,-1.40560847361764,
-3.90482332276299));
#44416=CARTESIAN_POINT('Ctrl Pts',(-108.982695370205,-2.43188023199054,
-3.09943859240772));
#44417=CARTESIAN_POINT('Ctrl Pts',(-109.042742406125,-3.36148473912884,
-2.36991517990962));
#44418=CARTESIAN_POINT('Ctrl Pts',(-109.102789442045,-3.93024421607646,
-1.180270013047));
#44419=CARTESIAN_POINT('Ctrl Pts',(-109.162836477965,-3.93801241551785,
0.0024295370903759));
#44420=CARTESIAN_POINT('Ctrl Pts',(-109.346163522035,-3.93703449438079,
0.00416483169883862));
#44421=CARTESIAN_POINT('Ctrl Pts',(-109.287193326892,-3.92832622712764,
-1.15685981483869));
#44422=CARTESIAN_POINT('Ctrl Pts',(-109.228223131748,-3.38309787307521,
-2.32839455203784));
#44423=CARTESIAN_POINT('Ctrl Pts',(-109.169252936605,-2.48212429262528,
-3.06019835595209));
#44424=CARTESIAN_POINT('Ctrl Pts',(-109.102961759373,-1.469297403408,-3.8828535217847));
#44425=CARTESIAN_POINT('Ctrl Pts',(-109.03667058214,-0.00691284144458862,
-4.14981770335895));
#44426=CARTESIAN_POINT('Ctrl Pts',(-108.970379404908,1.23227169689118,-3.74142213250333));
#44427=CARTESIAN_POINT('Ctrl Pts',(-108.904088227675,2.47145623522696,-3.33302656164771));
#44428=CARTESIAN_POINT('Ctrl Pts',(-108.837797050443,3.48744074993509,-2.24927123836224));
#44429=CARTESIAN_POINT('Ctrl Pts',(-108.77150587321,3.81396665854964,-0.986513452623214));
#44430=CARTESIAN_POINT('Ctrl Pts',(-108.705214695978,4.14049256716419,0.276244333115812));
#44431=CARTESIAN_POINT('Ctrl Pts',(-108.638923518745,3.77755986968516,1.71800458130839));
#44432=CARTESIAN_POINT('Ctrl Pts',(-108.572632341513,2.89164421227576,2.67562232022101));
#44433=CARTESIAN_POINT('Ctrl Pts',(-108.50634116428,2.00572855486636,3.63324005913362));
#44434=CARTESIAN_POINT('Ctrl Pts',(-108.440049987048,0.596829937526585,
4.10671528876627));
#44435=CARTESIAN_POINT('Ctrl Pts',(-108.373758809815,-0.687666737997685,
3.87895524761894));
#44436=CARTESIAN_POINT('Ctrl Pts',(-108.307467632583,-1.97216341352196,
3.65119520647162));
#44437=CARTESIAN_POINT('Ctrl Pts',(-108.24117645535,-3.13225814723073,2.72219989454433));
#44438=CARTESIAN_POINT('Ctrl Pts',(-108.174885278118,-3.63507393339194,
1.51852718954578));
#44439=CARTESIAN_POINT('Ctrl Pts',(-108.148644692757,-3.8341076677211,1.04206746019844));
#44440=CARTESIAN_POINT('Ctrl Pts',(-108.122404107396,-3.9301537168598,0.522569095592642));
#44441=CARTESIAN_POINT('Ctrl Pts',(-108.096163522035,-3.92761091684392,
0.00216275952952855));
#44442=CARTESIAN_POINT('Origin',(-54.75,0.,0.));
#44443=CARTESIAN_POINT('',(-106.662836477965,-3.9292423024608,-0.00304753711075328));
#44444=CARTESIAN_POINT('',(-106.846163522035,-3.92976983246225,-0.00322859656514467));
#44445=CARTESIAN_POINT('',(-54.75,-3.933,-4.81653586104654E-16));
#44446=CARTESIAN_POINT('Ctrl Pts',(-106.662836477965,-3.9292423024608,-0.00304753711075328));
#44447=CARTESIAN_POINT('Ctrl Pts',(-106.706919825821,-3.92295993091212,
0.870298256322931));
#44448=CARTESIAN_POINT('Ctrl Pts',(-106.751003173677,-3.63576905577679,
1.74739404838634));
#44449=CARTESIAN_POINT('Ctrl Pts',(-106.795086521533,-3.10063925105004,
2.43016447487287));
#44450=CARTESIAN_POINT('Ctrl Pts',(-106.861377698765,-2.29592757526039,
3.45689355859143));
#44451=CARTESIAN_POINT('Ctrl Pts',(-106.927668875998,-0.930546250520585,
4.0441905019856));
#44452=CARTESIAN_POINT('Ctrl Pts',(-106.99396005323,0.368247256980288,3.92225124680251));
#44453=CARTESIAN_POINT('Ctrl Pts',(-107.060251230463,1.66704076448116,3.80031199161943));
#44454=CARTESIAN_POINT('Ctrl Pts',(-107.126542407695,2.8992464547431,2.96913653785908));
#44455=CARTESIAN_POINT('Ctrl Pts',(-107.192833584928,3.49878754932471,1.81056630634775));
#44456=CARTESIAN_POINT('Ctrl Pts',(-107.25912476216,4.09832864390631,0.651996074836404));
#44457=CARTESIAN_POINT('Ctrl Pts',(-107.325415939392,4.06520514280758,-0.833968934425934));
#44458=CARTESIAN_POINT('Ctrl Pts',(-107.391707116625,3.41463443053716,-1.96467215928025));
#44459=CARTESIAN_POINT('Ctrl Pts',(-107.457998293857,2.76406371826674,-3.09537538413456));
#44460=CARTESIAN_POINT('Ctrl Pts',(-107.52428947109,1.49604579482464,-3.87081682458085));
#44461=CARTESIAN_POINT('Ctrl Pts',(-107.590580648323,0.193108614131911,
-3.93476300637775));
#44462=CARTESIAN_POINT('Ctrl Pts',(-107.656871825555,-1.10982856656081,
-3.99870918817465));
#44463=CARTESIAN_POINT('Ctrl Pts',(-107.723163002787,-2.44768500450416,
-3.35116011132216));
#44464=CARTESIAN_POINT('Ctrl Pts',(-107.78945418002,-3.20584660222602,-2.28959081968466));
#44465=CARTESIAN_POINT('Ctrl Pts',(-107.830581612668,-3.6762144754277,-1.6309870451541));
#44466=CARTESIAN_POINT('Ctrl Pts',(-107.871709045317,-3.92345583920203,
-0.813025486238145));
#44467=CARTESIAN_POINT('Ctrl Pts',(-107.912836477965,-3.92799297266711,
0.00241250680657806));
#44468=CARTESIAN_POINT('Ctrl Pts',(-108.096163522035,-3.92761091684392,
0.00216275952952855));
#44469=CARTESIAN_POINT('Ctrl Pts',(-108.056112930163,-3.92372988125552,
-0.792125229330703));
#44470=CARTESIAN_POINT('Ctrl Pts',(-108.016062338292,-3.69018182508964,
-1.58852837726987));
#44471=CARTESIAN_POINT('Ctrl Pts',(-107.976011746421,-3.24260701068257,
-2.23724918584132));
#44472=CARTESIAN_POINT('Ctrl Pts',(-107.909720569188,-2.50178746319835,
-3.3110027581601));
#44473=CARTESIAN_POINT('Ctrl Pts',(-107.843429391955,-1.17461152961626,
-3.98015980472787));
#44474=CARTESIAN_POINT('Ctrl Pts',(-107.777138214723,0.129194693027765,
-3.93737157699463));
#44475=CARTESIAN_POINT('Ctrl Pts',(-107.71084703749,1.43300091567179,-3.89458334926139));
#44476=CARTESIAN_POINT('Ctrl Pts',(-107.644555860258,2.71343742737774,-3.13984984722715));
#44477=CARTESIAN_POINT('Ctrl Pts',(-107.578264683026,3.38228103075617,-2.01986321819148));
#44478=CARTESIAN_POINT('Ctrl Pts',(-107.511973505793,4.0511246341346,-0.899876589155813));
#44479=CARTESIAN_POINT('Ctrl Pts',(-107.445682328561,4.10837532918551,0.585363166881283));
#44480=CARTESIAN_POINT('Ctrl Pts',(-107.379391151328,3.52772644721466,1.75351779922835));
#44481=CARTESIAN_POINT('Ctrl Pts',(-107.313099974096,2.94707756524382,2.92167243157543));
#44482=CARTESIAN_POINT('Ctrl Pts',(-107.246808796863,1.72852910625122,3.77274194023248));
#44483=CARTESIAN_POINT('Ctrl Pts',(-107.180517619631,0.431886470594226,
3.91575343066037));
#44484=CARTESIAN_POINT('Ctrl Pts',(-107.114226442398,-0.86475616506276,
4.05876492108826));
#44485=CARTESIAN_POINT('Ctrl Pts',(-107.047935265166,-2.23949297738414,
3.49371839328699));
#44486=CARTESIAN_POINT('Ctrl Pts',(-106.981644087933,-3.06077004551541,
2.48019187083103));
#44487=CARTESIAN_POINT('Ctrl Pts',(-106.9364838993,-3.62025667503408,1.78973726058977));
#44488=CARTESIAN_POINT('Ctrl Pts',(-106.891323710667,-3.92288946057965,
0.891148613896295));
#44489=CARTESIAN_POINT('Ctrl Pts',(-106.846163522035,-3.92976983246225,
-0.00322859656514467));
#44490=CARTESIAN_POINT('Origin',(-54.75,0.,0.));
#44491=CARTESIAN_POINT('',(-105.412836477965,-3.93906449910886,-0.0011929863556448));
#44492=CARTESIAN_POINT('',(-105.596163522035,-3.93929733158332,-0.000812073971306047));
#44493=CARTESIAN_POINT('',(-54.75,-3.933,-4.81653586104654E-16));
#44494=CARTESIAN_POINT('Ctrl Pts',(-105.412836477965,-3.93906449910886,
-0.0011929863556448));
#44495=CARTESIAN_POINT('Ctrl Pts',(-105.475839429093,-3.93412821791734,
1.23897268504913));
#44496=CARTESIAN_POINT('Ctrl Pts',(-105.53884238022,-3.29985743316472,2.48348604357577));
#44497=CARTESIAN_POINT('Ctrl Pts',(-105.601845331348,-2.29134164332814,
3.20459297925897));
#44498=CARTESIAN_POINT('Ctrl Pts',(-105.66813650858,-1.2301897802929,3.96333565434574));
#44499=CARTESIAN_POINT('Ctrl Pts',(-105.734427685813,0.245291424639117,
4.14261130709347));
#44500=CARTESIAN_POINT('Ctrl Pts',(-105.800718863045,1.45726439370239,3.66006053535915));
#44501=CARTESIAN_POINT('Ctrl Pts',(-105.867010040278,2.66923736276567,3.17750976362482));
#44502=CARTESIAN_POINT('Ctrl Pts',(-105.93330121751,3.61770209596021,2.03313256740845));
#44503=CARTESIAN_POINT('Ctrl Pts',(-105.999592394743,3.86693291628907,0.752656973826566));
#44504=CARTESIAN_POINT('Ctrl Pts',(-106.065883571975,4.11616373661792,-0.527818619755315));
#44505=CARTESIAN_POINT('Ctrl Pts',(-106.132174749208,3.66616064408109,-1.9443926107027));
#44506=CARTESIAN_POINT('Ctrl Pts',(-106.19846592644,2.72365553051665,-2.84628939344151));
#44507=CARTESIAN_POINT('Ctrl Pts',(-106.264757103673,1.7811504169522,-3.74818617618033));
#44508=CARTESIAN_POINT('Ctrl Pts',(-106.331048280905,0.346143282360121,
-4.13540575071056));
#44509=CARTESIAN_POINT('Ctrl Pts',(-106.397339458138,-0.922122139650376,
-3.83005915992413));
#44510=CARTESIAN_POINT('Ctrl Pts',(-106.46363063537,-2.19038756166086,-3.52471256913771));
#44511=CARTESIAN_POINT('Ctrl Pts',(-106.529921812603,-3.29191127108978,
-2.52679981303464));
#44512=CARTESIAN_POINT('Ctrl Pts',(-106.596212989835,-3.72065211238448,
-1.29476282296164));
#44513=CARTESIAN_POINT('Ctrl Pts',(-106.618420819212,-3.86428213749116,
-0.882025134426596));
#44514=CARTESIAN_POINT('Ctrl Pts',(-106.640628648588,-3.93240716725033,
-0.443012179332428));
#44515=CARTESIAN_POINT('Ctrl Pts',(-106.662836477965,-3.9292423024608,-0.00304753711075328));
#44516=CARTESIAN_POINT('Ctrl Pts',(-106.846163522035,-3.92976983246225,
-0.00322859656514467));
#44517=CARTESIAN_POINT('Ctrl Pts',(-106.825032533435,-3.93298924017984,
-0.421718315279691));
#44518=CARTESIAN_POINT('Ctrl Pts',(-106.803901544835,-3.87145616371382,
-0.839285975727229));
#44519=CARTESIAN_POINT('Ctrl Pts',(-106.782770556236,-3.74118562589317,
-1.23417777390522));
#44520=CARTESIAN_POINT('Ctrl Pts',(-106.716479379003,-3.3325068141985,-2.47301437907483));
#44521=CARTESIAN_POINT('Ctrl Pts',(-106.650188201771,-2.24733186686799,
-3.48868107230339));
#44522=CARTESIAN_POINT('Ctrl Pts',(-106.583897024538,-0.984191712527803,
-3.81458091516079));
#44523=CARTESIAN_POINT('Ctrl Pts',(-106.517605847306,0.278948441812384,
-4.14048075801819));
#44524=CARTESIAN_POINT('Ctrl Pts',(-106.451314670073,1.72005380316225,-3.77661375050442));
#44525=CARTESIAN_POINT('Ctrl Pts',(-106.385023492841,2.67707932403443,-2.89014003690369));
#44526=CARTESIAN_POINT('Ctrl Pts',(-106.318732315608,3.63410484490661,-2.00366632330296));
#44527=CARTESIAN_POINT('Ctrl Pts',(-106.252441138376,4.1070505253011,-0.594585903615262));
#44528=CARTESIAN_POINT('Ctrl Pts',(-106.186149961143,3.87864450964041,0.689767842792736));
#44529=CARTESIAN_POINT('Ctrl Pts',(-106.119858783911,3.65023849397972,1.97412158920074));
#44530=CARTESIAN_POINT('Ctrl Pts',(-106.053567606678,2.72048078226385,3.13374866232904));
#44531=CARTESIAN_POINT('Ctrl Pts',(-105.987276429446,1.51650308769314,3.63591539972664));
#44532=CARTESIAN_POINT('Ctrl Pts',(-105.920985252213,0.312525393122438,
4.13808213712423));
#44533=CARTESIAN_POINT('Ctrl Pts',(-105.854694074981,-1.1656722843031,3.98278853879111));
#44534=CARTESIAN_POINT('Ctrl Pts',(-105.788402897748,-2.2390044489117,3.24137653441947));
#44535=CARTESIAN_POINT('Ctrl Pts',(-105.724323105844,-3.27653168291185,
2.52469704645246));
#44536=CARTESIAN_POINT('Ctrl Pts',(-105.660243313939,-3.93575441738167,
1.26035117732303));
#44537=CARTESIAN_POINT('Ctrl Pts',(-105.596163522035,-3.93929733158332,
-0.000812073971306047));
#44538=CARTESIAN_POINT('Origin',(-54.75,0.,0.));
#44539=CARTESIAN_POINT('',(-104.162836477965,-3.93287283233362,0.00363418799115139));
#44540=CARTESIAN_POINT('',(-104.346163522035,-3.93222879534157,0.0036280465933886));
#44541=CARTESIAN_POINT('',(-54.75,-3.933,-4.81653586104654E-16));
#44542=CARTESIAN_POINT('Ctrl Pts',(-104.162836477965,-3.93287283233362,
0.00363418799115139));
#44543=CARTESIAN_POINT('Ctrl Pts',(-104.178467855132,-3.93572410183324,
0.312586993871509));
#44544=CARTESIAN_POINT('Ctrl Pts',(-104.194099232299,-3.90239986290354,
0.620931697066951));
#44545=CARTESIAN_POINT('Ctrl Pts',(-104.209730609466,-3.83056314357427,
0.920026454639353));
#44546=CARTESIAN_POINT('Ctrl Pts',(-104.276021786698,-3.52591047976832,
2.18845874770064));
#44547=CARTESIAN_POINT('Ctrl Pts',(-104.342312963931,-2.52860043113539,
3.29052826488843));
#44548=CARTESIAN_POINT('Ctrl Pts',(-104.408604141163,-1.29679825792208,
3.71994313838599));
#44549=CARTESIAN_POINT('Ctrl Pts',(-104.474895318396,-0.0649960847087633,
4.14935801188356));
#44550=CARTESIAN_POINT('Ctrl Pts',(-104.541186495628,1.40129821308494,3.9061182416909));
#44551=CARTESIAN_POINT('Ctrl Pts',(-104.607477672861,2.42846752975822,3.10196842832357));
#44552=CARTESIAN_POINT('Ctrl Pts',(-104.673768850093,3.45563684643151,2.29781861495623));
#44553=CARTESIAN_POINT('Ctrl Pts',(-104.740060027326,4.04368118198438,0.932758758414215));
#44554=CARTESIAN_POINT('Ctrl Pts',(-104.806351204558,3.92245236484942,-0.366101242486227));
#44555=CARTESIAN_POINT('Ctrl Pts',(-104.872642381791,3.80122354771446,-1.66496124338667));
#44556=CARTESIAN_POINT('Ctrl Pts',(-104.938933559023,2.97072157789166,-2.89762138864554));
#44557=CARTESIAN_POINT('Ctrl Pts',(-105.005224736256,1.8124799131427,-3.4977963407172));
#44558=CARTESIAN_POINT('Ctrl Pts',(-105.071515913488,0.654238248393729,
-4.09797129278886));
#44559=CARTESIAN_POINT('Ctrl Pts',(-105.137807090721,-0.83174311128142,
-4.0656610516733));
#44560=CARTESIAN_POINT('Ctrl Pts',(-105.204098267953,-1.96280280406628,
-3.41570897780247));
#44561=CARTESIAN_POINT('Ctrl Pts',(-105.270389445186,-3.09386249685114,
-2.76575690393164));
#44562=CARTESIAN_POINT('Ctrl Pts',(-105.336680622418,-3.87000052274572,
-1.49816299730554));
#44563=CARTESIAN_POINT('Ctrl Pts',(-105.402971799651,-3.93465827512377,
-0.195261195279577));
#44564=CARTESIAN_POINT('Ctrl Pts',(-105.406260025755,-3.93786547882909,
-0.130633655140379));
#44565=CARTESIAN_POINT('Ctrl Pts',(-105.40954825186,-3.93932213162264,-0.065919242222293));
#44566=CARTESIAN_POINT('Ctrl Pts',(-105.412836477965,-3.93906449910886,
-0.0011929863556448));
#44567=CARTESIAN_POINT('Ctrl Pts',(-105.596163522035,-3.93929733158332,
-0.000812073971306047));
#44568=CARTESIAN_POINT('Ctrl Pts',(-105.593952136707,-3.93941959709403,
-0.0443346546021957));
#44569=CARTESIAN_POINT('Ctrl Pts',(-105.591740751379,-3.93876099306918,
-0.0878534449543062));
#44570=CARTESIAN_POINT('Ctrl Pts',(-105.589529366051,-3.93731011969357,
-0.131345805750395));
#44571=CARTESIAN_POINT('Ctrl Pts',(-105.523238188818,-3.8938169740752,-1.43512573113845));
#44572=CARTESIAN_POINT('Ctrl Pts',(-105.456947011586,-3.13836403104679,
-2.7151551715044));
#44573=CARTESIAN_POINT('Ctrl Pts',(-105.390655834354,-2.01800715800226,
-3.38338731833911));
#44574=CARTESIAN_POINT('Ctrl Pts',(-105.324364657121,-0.897650284957724,
-4.05161946517383));
#44575=CARTESIAN_POINT('Ctrl Pts',(-105.258073479888,0.587610518102931,
-4.10805431847731));
#44576=CARTESIAN_POINT('Ctrl Pts',(-105.191782302656,1.7554449186165,-3.52676563254053));
#44577=CARTESIAN_POINT('Ctrl Pts',(-105.125491125424,2.92327931913007,-2.94547694660376));
#44578=CARTESIAN_POINT('Ctrl Pts',(-105.059199948191,3.77368731709656,-1.72646472142674));
#44579=CARTESIAN_POINT('Ctrl Pts',(-104.992908770959,3.9159906024442,-0.429744433298131));
#44580=CARTESIAN_POINT('Ctrl Pts',(-104.926617593726,4.05829388779184,0.866975854830487));
#44581=CARTESIAN_POINT('Ctrl Pts',(-104.860326416494,3.49249246052062,2.24140420591069));
#44582=CARTESIAN_POINT('Ctrl Pts',(-104.794035239261,2.47851607864565,3.06212682895171));
#44583=CARTESIAN_POINT('Ctrl Pts',(-104.727744062029,1.46453969677069,3.88284945199272));
#44584=CARTESIAN_POINT('Ctrl Pts',(-104.661452884796,0.00238836029199191,
4.14986634699456));
#44585=CARTESIAN_POINT('Ctrl Pts',(-104.595161707564,-1.2362241064848,3.7405096758632));
#44586=CARTESIAN_POINT('Ctrl Pts',(-104.528870530331,-2.47483657326161,
3.33115300473184));
#44587=CARTESIAN_POINT('Ctrl Pts',(-104.462579353099,-3.48991017033652,
2.24542276746725));
#44588=CARTESIAN_POINT('Ctrl Pts',(-104.396288175866,-3.81511904469398,
0.982104550990416));
#44589=CARTESIAN_POINT('Ctrl Pts',(-104.379579957922,-3.89708561968762,
0.663694213830095));
#44590=CARTESIAN_POINT('Ctrl Pts',(-104.362871739978,-3.93522812177383,
0.334002493099642));
#44591=CARTESIAN_POINT('Ctrl Pts',(-104.346163522035,-3.93222879534157,
0.0036280465933886));
#44592=CARTESIAN_POINT('Origin',(-54.75,0.,0.));
#44593=CARTESIAN_POINT('',(-102.912836477965,-3.92652662675955,-0.000460690130250907));
#44594=CARTESIAN_POINT('',(-103.096163522035,-3.92662908956275,-0.000809190342590051));
#44595=CARTESIAN_POINT('',(-54.75,-3.933,-4.81653586104654E-16));
#44596=CARTESIAN_POINT('Ctrl Pts',(-102.912836477965,-3.92652662675955,
-0.000460690130250907));
#44597=CARTESIAN_POINT('Ctrl Pts',(-102.947387458404,-3.92581264510619,
0.685223319963354));
#44598=CARTESIAN_POINT('Ctrl Pts',(-102.981938438842,-3.75521499743656,
1.371239773391));
#44599=CARTESIAN_POINT('Ctrl Pts',(-103.016489419281,-3.41678238161711,
1.96093366303795));
#44600=CARTESIAN_POINT('Ctrl Pts',(-103.082780596514,-2.76744924456302,
3.09234879670921));
#44601=CARTESIAN_POINT('Ctrl Pts',(-103.149071773746,-1.50028017576009,
3.86918024857726));
#44602=CARTESIAN_POINT('Ctrl Pts',(-103.215362950979,-0.197413946338789,
3.93455085212624));
#44603=CARTESIAN_POINT('Ctrl Pts',(-103.281654128211,1.10545228308254,3.99992145567523));
#44604=CARTESIAN_POINT('Ctrl Pts',(-103.347945305443,2.44401567312224,3.35383121090512));
#44605=CARTESIAN_POINT('Ctrl Pts',(-103.414236482676,3.20333882817959,2.29309463957116));
#44606=CARTESIAN_POINT('Ctrl Pts',(-103.480527659908,3.96266198323693,1.23235806823722));
#44607=CARTESIAN_POINT('Ctrl Pts',(-103.546818837141,4.14274490331193,-0.243024829660569));
#44608=CARTESIAN_POINT('Ctrl Pts',(-103.613110014373,3.6608573100401,-1.45526163616176));
#44609=CARTESIAN_POINT('Ctrl Pts',(-103.679401191606,3.17896971676828,-2.66749844266296));
#44610=CARTESIAN_POINT('Ctrl Pts',(-103.745692368838,2.03511161014963,-3.61658915776756));
#44611=CARTESIAN_POINT('Ctrl Pts',(-103.811983546071,0.754772578695459,
-3.86652053255643));
#44612=CARTESIAN_POINT('Ctrl Pts',(-103.878274723303,-0.525566452758725,
-4.1164519073453));
#44613=CARTESIAN_POINT('Ctrl Pts',(-103.944565900536,-1.94238640904844,
-3.66722394181842));
#44614=CARTESIAN_POINT('Ctrl Pts',(-104.010857077768,-2.84479874770382,
-2.72521242458757));
#44615=CARTESIAN_POINT('Ctrl Pts',(-104.061516877834,-3.53442337893724,
-2.00532605185032));
#44616=CARTESIAN_POINT('Ctrl Pts',(-104.112176677899,-3.92363214027932,
-0.997652340282243));
#44617=CARTESIAN_POINT('Ctrl Pts',(-104.162836477965,-3.93287283233362,
0.00363418799115139));
#44618=CARTESIAN_POINT('Ctrl Pts',(-104.346163522035,-3.93222879534157,
0.0036280465933886));
#44619=CARTESIAN_POINT('Ctrl Pts',(-104.296580562746,-3.92332805674193,
-0.976784274227112));
#44620=CARTESIAN_POINT('Ctrl Pts',(-104.246997603457,-3.55211073389444,
-1.96320903737145));
#44621=CARTESIAN_POINT('Ctrl Pts',(-104.197414644169,-2.88867477093556,
-2.67866025116411));
#44622=CARTESIAN_POINT('Ctrl Pts',(-104.131123466936,-2.00167747117968,
-3.63520064115272));
#44623=CARTESIAN_POINT('Ctrl Pts',(-104.064832289704,-0.592338720027921,
-4.10737522544087));
#44624=CARTESIAN_POINT('Ctrl Pts',(-103.998541112471,0.691889813476739,
-3.87826651489836));
#44625=CARTESIAN_POINT('Ctrl Pts',(-103.932249935239,1.97611834698141,-3.64915780435585));
#44626=CARTESIAN_POINT('Ctrl Pts',(-103.865958758006,3.13523666283897,-2.71876579898269));
#44627=CARTESIAN_POINT('Ctrl Pts',(-103.799667580774,3.63674461669093,-1.51451354141037));
#44628=CARTESIAN_POINT('Ctrl Pts',(-103.733376403541,4.1382525705429,-0.310261283838064));
#44629=CARTESIAN_POINT('Ctrl Pts',(-103.667085226309,3.98215016238928,1.16785122593339));
#44630=CARTESIAN_POINT('Ctrl Pts',(-103.600794049076,3.24015099882834,2.24077758353109));
#44631=CARTESIAN_POINT('Ctrl Pts',(-103.534502871844,2.4981518352674,3.31370394112879));
#44632=CARTESIAN_POINT('Ctrl Pts',(-103.468211694611,1.17025591629913,3.98144414655273));
#44633=CARTESIAN_POINT('Ctrl Pts',(-103.401920517379,-0.1335000096533,3.93723766385185));
#44634=CARTESIAN_POINT('Ctrl Pts',(-103.335629340146,-1.43725593560575,
3.89303118115098));
#44635=CARTESIAN_POINT('Ctrl Pts',(-103.269338162914,-2.71687186854237,
3.13687801032527));
#44636=CARTESIAN_POINT('Ctrl Pts',(-103.203046985682,-3.38449093516292,
2.0161556943744));
#44637=CARTESIAN_POINT('Ctrl Pts',(-103.167419164466,-3.74329905622377,
1.41382977451589));
#44638=CARTESIAN_POINT('Ctrl Pts',(-103.13179134325,-3.92533404230202,0.706199343721507));
#44639=CARTESIAN_POINT('Ctrl Pts',(-103.096163522035,-3.92662908956275,
-0.000809190342590051));
#44640=CARTESIAN_POINT('Origin',(-54.75,0.,0.));
#44641=CARTESIAN_POINT('',(-101.662836477965,-3.93456922033058,-0.0034735344748954));
#44642=CARTESIAN_POINT('',(-101.846163522035,-3.93520758847436,-0.00334434899688729));
#44643=CARTESIAN_POINT('',(-54.75,-3.933,-4.81653586104654E-16));
#44644=CARTESIAN_POINT('Ctrl Pts',(-101.662836477965,-3.93456922033058,
-0.0034735344748954));
#44645=CARTESIAN_POINT('Ctrl Pts',(-101.716307061675,-3.92483692582627,
1.05219970964738));
#44646=CARTESIAN_POINT('Ctrl Pts',(-101.769777645386,-3.48619833240327,
2.11500422185773));
#44647=CARTESIAN_POINT('Ctrl Pts',(-101.823248229096,-2.72676850018497,
2.84330726805342));
#44648=CARTESIAN_POINT('Ctrl Pts',(-101.889539406329,-1.78525086357474,
3.74623487729314));
#44649=CARTESIAN_POINT('Ctrl Pts',(-101.955830583561,-0.350668299552551,
4.13502456406624));
#44650=CARTESIAN_POINT('Ctrl Pts',(-102.022121760794,0.917930489175272,
3.83106594712348));
#44651=CARTESIAN_POINT('Ctrl Pts',(-102.088412938026,2.18652927790309,3.52710733018071));
#44652=CARTESIAN_POINT('Ctrl Pts',(-102.154704115259,3.28914429133654,2.53040040952208));
#44653=CARTESIAN_POINT('Ctrl Pts',(-102.220995292491,3.71923306031976,1.29883336775382));
#44654=CARTESIAN_POINT('Ctrl Pts',(-102.287286469724,4.14932182930299,0.0672663259855481));
#44655=CARTESIAN_POINT('Ctrl Pts',(-102.353577646956,3.90688435383597,-1.39916083689237));
#44656=CARTESIAN_POINT('Ctrl Pts',(-102.419868824189,3.1032966590433,-2.42676997676681));
#44657=CARTESIAN_POINT('Ctrl Pts',(-102.486160001421,2.29970896425063,-3.45437911664124));
#44658=CARTESIAN_POINT('Ctrl Pts',(-102.552451178654,0.934971050132315,
-4.04317023351221));
#44659=CARTESIAN_POINT('Ctrl Pts',(-102.618742355886,-0.363955084476125,
-3.92265208381421));
#44660=CARTESIAN_POINT('Ctrl Pts',(-102.685033533119,-1.66288121908456,
-3.80213393411621));
#44661=CARTESIAN_POINT('Ctrl Pts',(-102.751324710351,-2.89599557418311,
-2.97230651784925));
#44662=CARTESIAN_POINT('Ctrl Pts',(-102.817615887584,-3.49680414907977,
-1.81439340197853));
#44663=CARTESIAN_POINT('Ctrl Pts',(-102.849356084377,-3.78447112376253,
-1.25998493161789));
#44664=CARTESIAN_POINT('Ctrl Pts',(-102.881096281171,-3.9271825247369,-0.630363087758761));
#44665=CARTESIAN_POINT('Ctrl Pts',(-102.912836477965,-3.92652662675955,
-0.000460690130250907));
#44666=CARTESIAN_POINT('Ctrl Pts',(-103.096163522035,-3.92662908956275,
-0.000809190342590051));
#44667=CARTESIAN_POINT('Ctrl Pts',(-103.065500166018,-3.92774368186336,
-0.609301476630808));
#44668=CARTESIAN_POINT('Ctrl Pts',(-103.034836810001,-3.79497849937131,
-1.21733310439087));
#44669=CARTESIAN_POINT('Ctrl Pts',(-103.004173453984,-3.52580464015748,
-1.75737426679605));
#44670=CARTESIAN_POINT('Ctrl Pts',(-102.937882276752,-2.94387707822704,
-2.92489045093963));
#44671=CARTESIAN_POINT('Ctrl Pts',(-102.871591099519,-1.72439975406168,
-3.7746313581508));
#44672=CARTESIAN_POINT('Ctrl Pts',(-102.805299922287,-0.427601802340093,
-3.91622514327406));
#44673=CARTESIAN_POINT('Ctrl Pts',(-102.739008745054,0.869196149381524,
-4.05781892839732));
#44674=CARTESIAN_POINT('Ctrl Pts',(-102.672717567822,2.24331472865938,-3.49126559143261));
#44675=CARTESIAN_POINT('Ctrl Pts',(-102.606426390589,3.06348244945187,-2.47684031702992));
#44676=CARTESIAN_POINT('Ctrl Pts',(-102.540135213357,3.88365017024434,-1.46241504262724));
#44677=CARTESIAN_POINT('Ctrl Pts',(-102.473844036124,4.14986703255148,-0.000117830786606349));
#44678=CARTESIAN_POINT('Ctrl Pts',(-102.407552858892,3.73983273652221,1.23827047812727));
#44679=CARTESIAN_POINT('Ctrl Pts',(-102.341261681659,3.32979844049294,2.47665878704114));
#44680=CARTESIAN_POINT('Ctrl Pts',(-102.274970504427,2.24351298612724,3.49113819302825));
#44681=CARTESIAN_POINT('Ctrl Pts',(-102.208679327194,0.980017026380408,
3.81565581547556));
#44682=CARTESIAN_POINT('Ctrl Pts',(-102.142388149962,-0.283478933366429,
4.14017343792287));
#44683=CARTESIAN_POINT('Ctrl Pts',(-102.076096972729,-1.72418539849439,
3.7747292768304));
#44684=CARTESIAN_POINT('Ctrl Pts',(-102.009805795497,-2.68024033984199,
2.88720875498287));
#44685=CARTESIAN_POINT('Ctrl Pts',(-101.955258371009,-3.46692624430341,
2.1569161177485));
#44686=CARTESIAN_POINT('Ctrl Pts',(-101.900710946522,-3.92546652330563,
1.07313841850271));
#44687=CARTESIAN_POINT('Ctrl Pts',(-101.846163522035,-3.93520758847436,
-0.00334434899688729));
#44688=CARTESIAN_POINT('Origin',(-54.75,0.,0.));
#44689=CARTESIAN_POINT('',(-100.412836477965,-3.93811660215707,0.00210082759382085));
#44690=CARTESIAN_POINT('',(-100.596163522035,-3.93764551384021,0.00240487699158903));
#44691=CARTESIAN_POINT('',(-54.75,-3.933,-4.81653586104654E-16));
#44692=CARTESIAN_POINT('Ctrl Pts',(-100.412836477965,-3.93811660215707,
0.00210082759382085));
#44693=CARTESIAN_POINT('Ctrl Pts',(-100.418935487715,-3.93889166556813,
0.122231846672544));
#44694=CARTESIAN_POINT('Ctrl Pts',(-100.425034497464,-3.93387331381181,
0.242297225123603));
#44695=CARTESIAN_POINT('Ctrl Pts',(-100.431133507214,-3.92285062854615,
0.361808817307622));
#44696=CARTESIAN_POINT('Ctrl Pts',(-100.497424684447,-3.80304318233601,
1.66080069696202));
#44697=CARTESIAN_POINT('Ctrl Pts',(-100.563715861679,-2.97389056792372,
2.89436889351655));
#44698=CARTESIAN_POINT('Ctrl Pts',(-100.630007038912,-1.81630634760845,
3.4958109110482));
#44699=CARTESIAN_POINT('Ctrl Pts',(-100.696298216144,-0.658722127293182,
4.09725292857986));
#44700=CARTESIAN_POINT('Ctrl Pts',(-100.762589393376,0.827293698925068,
4.06656876708864));
#44701=CARTESIAN_POINT('Ctrl Pts',(-100.828880570609,1.95906393488388,3.41785476186507));
#44702=CARTESIAN_POINT('Ctrl Pts',(-100.895171747841,3.09083417084268,2.76914075664151));
#44703=CARTESIAN_POINT('Ctrl Pts',(-100.961462925074,3.86835881654205,1.50239690768561));
#44704=CARTESIAN_POINT('Ctrl Pts',(-101.027754102307,3.93444225151268,0.199566639692902));
#44705=CARTESIAN_POINT('Ctrl Pts',(-101.094045279539,4.0005256864833,-1.10326362829981));
#44706=CARTESIAN_POINT('Ctrl Pts',(-101.160336456771,3.35516791072517,-2.44218031532932));
#44707=CARTESIAN_POINT('Ctrl Pts',(-101.226627634004,2.29484694896928,-3.20208372079382));
#44708=CARTESIAN_POINT('Ctrl Pts',(-101.292918811236,1.23452598721339,-3.96198712625833));
#44709=CARTESIAN_POINT('Ctrl Pts',(-101.359209988469,-0.240758160540255,
-4.14287725015782));
#44710=CARTESIAN_POINT('Ctrl Pts',(-101.425501165701,-1.45325844223339,
-3.6616529838645));
#44711=CARTESIAN_POINT('Ctrl Pts',(-101.491792342934,-2.6657587239265,-3.1804287175712));
#44712=CARTESIAN_POINT('Ctrl Pts',(-101.558083520166,-3.61547513955912,
-2.03709006108511));
#44713=CARTESIAN_POINT('Ctrl Pts',(-101.624374697399,-3.8661069927763,-0.756887966988903));
#44714=CARTESIAN_POINT('Ctrl Pts',(-101.637195290921,-3.91457873891088,
-0.509299202394739));
#44715=CARTESIAN_POINT('Ctrl Pts',(-101.650015884443,-3.93690272378647,
-0.256591353952766));
#44716=CARTESIAN_POINT('Ctrl Pts',(-101.662836477965,-3.93456922033058,
-0.0034735344748954));
#44717=CARTESIAN_POINT('Ctrl Pts',(-101.846163522035,-3.93520758847436,
-0.00334434899688729));
#44718=CARTESIAN_POINT('Ctrl Pts',(-101.83441976929,-3.9373047848478,-0.235105015511939));
#44719=CARTESIAN_POINT('Ctrl Pts',(-101.822676016544,-3.91859939235631,
-0.466527549826132));
#44720=CARTESIAN_POINT('Ctrl Pts',(-101.810932263799,-3.87788737855351,
-0.694011637814258));
#44721=CARTESIAN_POINT('Ctrl Pts',(-101.744641086567,-3.64807605835022,
-1.9781146261613));
#44722=CARTESIAN_POINT('Ctrl Pts',(-101.678349909334,-2.71705000037639,
-3.1367237202528));
#44723=CARTESIAN_POINT('Ctrl Pts',(-101.612058732102,-1.51252353149032,
-3.6375727127928));
#44724=CARTESIAN_POINT('Ctrl Pts',(-101.545767554869,-0.307997062604245,
-4.13842170533278));
#44725=CARTESIAN_POINT('Ctrl Pts',(-101.479476377637,1.17002981719408,-3.98151059632128));
#44726=CARTESIAN_POINT('Ctrl Pts',(-101.413185200404,2.24255004192927,-3.23892451032891));
#44727=CARTESIAN_POINT('Ctrl Pts',(-101.346894023172,3.31507026666446,-2.49633842433654));
#44728=CARTESIAN_POINT('Ctrl Pts',(-101.280602845939,3.9820838363365,-1.16807736136331));
#44729=CARTESIAN_POINT('Ctrl Pts',(-101.214311668707,3.93716403225775,0.13565418261995));
#44730=CARTESIAN_POINT('Ctrl Pts',(-101.148020491474,3.892244228179,1.43938572660321));
#44731=CARTESIAN_POINT('Ctrl Pts',(-101.081729314242,3.13539105034946,2.71858775159648));
#44732=CARTESIAN_POINT('Ctrl Pts',(-101.015438137009,2.01430362567694,3.38559353404262));
#44733=CARTESIAN_POINT('Ctrl Pts',(-100.949146959777,0.893216201004411,
4.05259931648877));
#44734=CARTESIAN_POINT('Ctrl Pts',(-100.882855782545,-0.592105470511098,
4.10740885638778));
#44735=CARTESIAN_POINT('Ctrl Pts',(-100.816564605312,-1.75930308809024,
3.52484259484059));
#44736=CARTESIAN_POINT('Ctrl Pts',(-100.75027342808,-2.92650070566936,2.94227633329342));
#44737=CARTESIAN_POINT('Ctrl Pts',(-100.683982250847,-3.77557426931215,
1.72233427030002));
#44738=CARTESIAN_POINT('Ctrl Pts',(-100.617691073615,-3.91645851219133,
0.425459042036407));
#44739=CARTESIAN_POINT('Ctrl Pts',(-100.610515223088,-3.93170887144981,
0.285075612773802));
#44740=CARTESIAN_POINT('Ctrl Pts',(-100.603339372561,-3.93866101580183,
0.143790718436667));
#44741=CARTESIAN_POINT('Ctrl Pts',(-100.596163522035,-3.93764551384021,
0.00240487699158903));
#44742=CARTESIAN_POINT('Origin',(-54.75,0.,0.));
#44743=CARTESIAN_POINT('',(-99.162836477965,-3.92804752189454,0.0024429329458453));
#44744=CARTESIAN_POINT('',(-99.3461635220346,-3.92766917194721,0.00216747763683944));
#44745=CARTESIAN_POINT('',(-54.75,-3.933,-4.81653586104654E-16));
#44746=CARTESIAN_POINT('Ctrl Pts',(-99.162836477965,-3.92804752189454,0.0024429329458453));
#44747=CARTESIAN_POINT('Ctrl Pts',(-99.1878550909865,-3.93085117530156,
0.498471328175551));
#44748=CARTESIAN_POINT('Ctrl Pts',(-99.212873704008,-3.8438135452639,0.993552004141601));
#44749=CARTESIAN_POINT('Ctrl Pts',(-99.2378923170294,-3.66244756155688,
1.45125481326075));
#44750=CARTESIAN_POINT('Ctrl Pts',(-99.3041834942619,-3.18188676629823,
2.66401820718217));
#44751=CARTESIAN_POINT('Ctrl Pts',(-99.3704746714944,-2.03906790220586,
3.61436003905749));
#44752=CARTESIAN_POINT('Ctrl Pts',(-99.4367658487269,-0.759003128703129,
3.86569229566779));
#44753=CARTESIAN_POINT('Ctrl Pts',(-99.5030570259594,0.521061644799618,
4.11702455227809));
#44754=CARTESIAN_POINT('Ctrl Pts',(-99.5693482031918,1.93837232771275,3.66934723362335));
#44755=CARTESIAN_POINT('Ctrl Pts',(-99.6356393804243,2.84181493724338,2.72832375949535));
#44756=CARTESIAN_POINT('Ctrl Pts',(-99.7019305576568,3.74525754677402,1.78730028536734));
#44757=CARTESIAN_POINT('Ctrl Pts',(-99.7682217348893,4.13483208292217,0.352930655766074));
#44758=CARTESIAN_POINT('Ctrl Pts',(-99.8345129121218,3.83156760383002,-0.915834248893745));
#44759=CARTESIAN_POINT('Ctrl Pts',(-99.9008040893543,3.52830312473787,-2.18459915355355));
#44760=CARTESIAN_POINT('Ctrl Pts',(-99.9670952665867,2.53219963040542,-3.28775933327191));
#44761=CARTESIAN_POINT('Ctrl Pts',(-100.033386443819,1.30086808876499,-3.71852186894192));
#44762=CARTESIAN_POINT('Ctrl Pts',(-100.099677621052,0.0695365471245464,
-4.14928440461195));
#44763=CARTESIAN_POINT('Ctrl Pts',(-100.165968798284,-1.39702304182386,
-3.90764929623362));
#44764=CARTESIAN_POINT('Ctrl Pts',(-100.232259975517,-2.42507169729408,
-3.10462396066732));
#44765=CARTESIAN_POINT('Ctrl Pts',(-100.292452142999,-3.35853644228551,
-2.37547963846285));
#44766=CARTESIAN_POINT('Ctrl Pts',(-100.352644310482,-3.93046736915652,
-1.18349268955144));
#44767=CARTESIAN_POINT('Ctrl Pts',(-100.412836477965,-3.93811660215707,
0.00210082759382085));
#44768=CARTESIAN_POINT('Ctrl Pts',(-100.596163522035,-3.93764551384021,
0.00240487699158903));
#44769=CARTESIAN_POINT('Ctrl Pts',(-100.537048195329,-3.92927971385468,
-1.16234488717197));
#44770=CARTESIAN_POINT('Ctrl Pts',(-100.477932868623,-3.38018017500286,
-2.33394554618446));
#44771=CARTESIAN_POINT('Ctrl Pts',(-100.418817541917,-2.47516381373419,
-3.0648371521742));
#44772=CARTESIAN_POINT('Ctrl Pts',(-100.352526364685,-1.46028995028229,
-3.88444972458731));
#44773=CARTESIAN_POINT('Ctrl Pts',(-100.286235187452,0.00215269873712037,
-4.14986647587968));
#44774=CARTESIAN_POINT('Ctrl Pts',(-100.21994401022,1.24031647896784,-3.73915467802112));
#44775=CARTESIAN_POINT('Ctrl Pts',(-100.153652832987,2.47848025919858,-3.32844288016256));
#44776=CARTESIAN_POINT('Ctrl Pts',(-100.087361655755,3.49236517064062,-2.24160253315307));
#44777=CARTESIAN_POINT('Ctrl Pts',(-100.021070478522,3.81619144408645,-0.977929208198526));
#44778=CARTESIAN_POINT('Ctrl Pts',(-99.9547793012898,4.14001771753228,0.285744116755994));
#44779=CARTESIAN_POINT('Ctrl Pts',(-99.8884881240572,3.77378535298192,1.72625041965556));
#44780=CARTESIAN_POINT('Ctrl Pts',(-99.8221969468248,2.88574187469724,2.68181962607206));
#44781=CARTESIAN_POINT('Ctrl Pts',(-99.7559057695923,1.99769839641255,3.63738883248858));
#44782=CARTESIAN_POINT('Ctrl Pts',(-99.6896145923599,0.587843804393512,
4.10802094242204));
#44783=CARTESIAN_POINT('Ctrl Pts',(-99.6233234151274,-0.69613325437843,
3.877507081401));
#44784=CARTESIAN_POINT('Ctrl Pts',(-99.5570322378949,-1.98011031315038,
3.64699322037997));
#44785=CARTESIAN_POINT('Ctrl Pts',(-99.4907410606623,-3.13820983867523,
2.71533338840444));
#44786=CARTESIAN_POINT('Ctrl Pts',(-99.4244498834298,-3.63839971997988,
1.51053306875976));
#44787=CARTESIAN_POINT('Ctrl Pts',(-99.3983544296314,-3.83529895277289,
1.03626466095421));
#44788=CARTESIAN_POINT('Ctrl Pts',(-99.372258975833,-3.93024882717627,0.519670536064647));
#44789=CARTESIAN_POINT('Ctrl Pts',(-99.3461635220346,-3.92766917194721,
0.00216747763683944));
#44790=CARTESIAN_POINT('Origin',(-54.75,0.,0.));
#44791=CARTESIAN_POINT('',(-97.912836477965,-3.92917392440496,-0.00302087060105316));
#44792=CARTESIAN_POINT('',(-98.0961635220346,-3.92969678555117,-0.00320611983441186));
#44793=CARTESIAN_POINT('',(-54.75,-3.933,-4.81653586104654E-16));
#44794=CARTESIAN_POINT('Ctrl Pts',(-97.912836477965,-3.92917392440496,-0.00302087060105316));
#44795=CARTESIAN_POINT('Ctrl Pts',(-97.9567746942582,-3.9229741941987,0.867487733808038));
#44796=CARTESIAN_POINT('Ctrl Pts',(-98.0007129105514,-3.63782776715222,
1.74168435746078));
#44797=CARTESIAN_POINT('Ctrl Pts',(-98.0446511268447,-3.10595033290786,
2.42337269186479));
#44798=CARTESIAN_POINT('Ctrl Pts',(-98.1109423040771,-2.30348759695728,
3.45186055517975));
#44799=CARTESIAN_POINT('Ctrl Pts',(-98.1772334813097,-0.939394794011104,
4.04214470581234));
#44800=CARTESIAN_POINT('Ctrl Pts',(-98.2435246585422,0.359662441830008,
3.92304799895481));
#44801=CARTESIAN_POINT('Ctrl Pts',(-98.3098158357747,1.65871967767111,3.80395129209728));
#44802=CARTESIAN_POINT('Ctrl Pts',(-98.3761070130071,2.89274134640716,2.97547372774965));
#44803=CARTESIAN_POINT('Ctrl Pts',(-98.4423981902396,3.49481662652941,1.81821874951834));
#44804=CARTESIAN_POINT('Ctrl Pts',(-98.5086893674721,4.09689190665167,0.660963771287009));
#44805=CARTESIAN_POINT('Ctrl Pts',(-98.5749805447046,4.06702079816011,-0.825068620827995));
#44806=CARTESIAN_POINT('Ctrl Pts',(-98.6412717219371,3.41892611896252,-1.95719362027428));
#44807=CARTESIAN_POINT('Ctrl Pts',(-98.7075628991696,2.77083143976494,-3.08931861972053));
#44808=CARTESIAN_POINT('Ctrl Pts',(-98.773854076402,1.50451318986137,-3.86753622649808));
#44809=CARTESIAN_POINT('Ctrl Pts',(-98.8401452536345,0.201719273305738,
-3.9343324731069));
#44810=CARTESIAN_POINT('Ctrl Pts',(-98.906436430867,-1.10107464324994,-4.00112871971572));
#44811=CARTESIAN_POINT('Ctrl Pts',(-98.9727276080995,-2.44034422645769,
-3.35650360615575));
#44812=CARTESIAN_POINT('Ctrl Pts',(-99.039018785332,-3.20082765484909,-2.29659857139199));
#44813=CARTESIAN_POINT('Ctrl Pts',(-99.080291349543,-3.67430093500554,-1.63670685682111));
#44814=CARTESIAN_POINT('Ctrl Pts',(-99.121563913754,-3.92342240677856,-0.815842388268304));
#44815=CARTESIAN_POINT('Ctrl Pts',(-99.162836477965,-3.92804752189454,0.0024429329458453));
#44816=CARTESIAN_POINT('Ctrl Pts',(-99.3461635220346,-3.92766917194721,
0.00216747763683944));
#44817=CARTESIAN_POINT('Ctrl Pts',(-99.3059677986006,-3.92369564042928,
-0.794960250952785));
#44818=CARTESIAN_POINT('Ctrl Pts',(-99.2657720751666,-3.68832063477402,
-1.5942445423951));
#44819=CARTESIAN_POINT('Ctrl Pts',(-99.2255763517325,-3.23769705223747,
-2.24432182899406));
#44820=CARTESIAN_POINT('Ctrl Pts',(-99.1592851745001,-2.49452426610597,
-3.31643559978938));
#44821=CARTESIAN_POINT('Ctrl Pts',(-99.0929939972675,-1.16589845675849,
-3.98272233406624));
#44822=CARTESIAN_POINT('Ctrl Pts',(-99.026702820035,0.137808314975248,-3.9370892220637));
#44823=CARTESIAN_POINT('Ctrl Pts',(-98.9604116428025,1.441515086709,-3.89145611006115));
#44824=CARTESIAN_POINT('Ctrl Pts',(-98.89412046557,2.72030282082902,-3.1339031517792));
#44825=CARTESIAN_POINT('Ctrl Pts',(-98.8278292883375,3.38669511943069,-2.01245095398391));
#44826=CARTESIAN_POINT('Ctrl Pts',(-98.761538111105,4.05308741803236,-0.89099875618864));
#44827=CARTESIAN_POINT('Ctrl Pts',(-98.6952469338725,4.10708428111567,0.594352681119947));
#44828=CARTESIAN_POINT('Ctrl Pts',(-98.62895575664,3.52387949434503,1.76123138272662));
#44829=CARTESIAN_POINT('Ctrl Pts',(-98.5626645794076,2.94067470757438,2.92811008433328));
#44830=CARTESIAN_POINT('Ctrl Pts',(-98.4963734021752,1.72026827094977,3.77651605023802));
#44831=CARTESIAN_POINT('Ctrl Pts',(-98.4300822249427,0.423316154370067,
3.91669070869985));
#44832=CARTESIAN_POINT('Ctrl Pts',(-98.3637910477102,-0.873635962209635,
4.05686536716169));
#44833=CARTESIAN_POINT('Ctrl Pts',(-98.2974998704777,-2.24713375874445,
3.4888087181806));
#44834=CARTESIAN_POINT('Ctrl Pts',(-98.2312086932452,-3.06619093742357,
2.47348656948608));
#44835=CARTESIAN_POINT('Ctrl Pts',(-98.186193636175,-3.62237212444157,1.78403155637298));
#44836=CARTESIAN_POINT('Ctrl Pts',(-98.1411785791048,-3.92289542988313,
0.888338135617226));
#44837=CARTESIAN_POINT('Ctrl Pts',(-98.0961635220346,-3.92969678555117,
-0.00320611983441186));
#44838=CARTESIAN_POINT('Origin',(-54.75,0.,0.));
#44839=CARTESIAN_POINT('',(-96.662836477965,-3.93902708289076,-0.00124319021292452));
#44840=CARTESIAN_POINT('',(-96.8461635220347,-3.93927071217365,-0.000864176983421456));
#44841=CARTESIAN_POINT('',(-54.75,-3.933,-4.81653586104654E-16));
#44842=CARTESIAN_POINT('Ctrl Pts',(-96.662836477965,-3.93902708289076,-0.00124319021292452));
#44843=CARTESIAN_POINT('Ctrl Pts',(-96.72569429753,-3.9339187179751,1.23609700737983));
#44844=CARTESIAN_POINT('Ctrl Pts',(-96.788552117095,-3.30296517319286,2.47792445112764));
#44845=CARTESIAN_POINT('Ctrl Pts',(-96.85140993666,-2.29834950631729,3.1995706307218));
#44846=CARTESIAN_POINT('Ctrl Pts',(-96.9177011138925,-1.23886071583314,
3.96063385438585));
#44847=CARTESIAN_POINT('Ctrl Pts',(-96.9839922911249,0.236224606744862,
4.14313822324457));
#44848=CARTESIAN_POINT('Ctrl Pts',(-97.0502834683574,1.44925074984827,3.66324104287865));
#44849=CARTESIAN_POINT('Ctrl Pts',(-97.1165746455898,2.66227689295166,3.18334386251274));
#44850=CARTESIAN_POINT('Ctrl Pts',(-97.1828658228224,3.61324385658045,2.04104513292222));
#44851=CARTESIAN_POINT('Ctrl Pts',(-97.2491570000549,3.86527644134641,0.761118063206283));
#44852=CARTESIAN_POINT('Ctrl Pts',(-97.3154481772874,4.11730902611237,-0.518809006509664));
#44853=CARTESIAN_POINT('Ctrl Pts',(-97.3817393545198,3.67040723201546,-1.93636441635105));
#44854=CARTESIAN_POINT('Ctrl Pts',(-97.4480305317523,2.72987820206941,-2.84032175572288));
#44855=CARTESIAN_POINT('Ctrl Pts',(-97.5143217089848,1.78934917212336,-3.74427909509472));
#44856=CARTESIAN_POINT('Ctrl Pts',(-97.5806128862173,0.355192906328163,
-4.13463836399704));
#44857=CARTESIAN_POINT('Ctrl Pts',(-97.6469040634498,-0.913737734453005,
-3.8320681135391));
#44858=CARTESIAN_POINT('Ctrl Pts',(-97.7131952406823,-2.18266837523417,
-3.52949786308117));
#44859=CARTESIAN_POINT('Ctrl Pts',(-97.7794864179148,-3.28637339100131,
-2.53399809326299));
#44860=CARTESIAN_POINT('Ctrl Pts',(-97.8457775951473,-3.71780956440737,
-1.30290242035523));
#44861=CARTESIAN_POINT('Ctrl Pts',(-97.8681305560865,-3.86328708245033,
-0.887784834006066));
#44862=CARTESIAN_POINT('Ctrl Pts',(-97.8904835170257,-3.93232795155548,
-0.445880105072101));
#44863=CARTESIAN_POINT('Ctrl Pts',(-97.912836477965,-3.92917392440496,-0.00302087060105316));
#44864=CARTESIAN_POINT('Ctrl Pts',(-98.0961635220346,-3.92969678555117,
-0.00320611983441186));
#44865=CARTESIAN_POINT('Ctrl Pts',(-98.0748874018724,-3.93291140905446,
-0.424589628899468));
#44866=CARTESIAN_POINT('Ctrl Pts',(-98.0536112817101,-3.87051065061225,
-0.84504624412362));
#44867=CARTESIAN_POINT('Ctrl Pts',(-98.0323351615478,-3.73847550018669,
-1.24236210851359));
#44868=CARTESIAN_POINT('Ctrl Pts',(-97.9660439843153,-3.32708632344723,
-2.48030098941083));
#44869=CARTESIAN_POINT('Ctrl Pts',(-97.8997528070828,-2.23969140914483,
-3.49359110279734));
#44870=CARTESIAN_POINT('Ctrl Pts',(-97.8334616298503,-0.975841097269099,
-3.81672593030297));
#44871=CARTESIAN_POINT('Ctrl Pts',(-97.7671704526178,0.288009214606619,
-4.1398607578086));
#44872=CARTESIAN_POINT('Ctrl Pts',(-97.7008792753852,1.72831492405566,-3.77284029943335));
#44873=CARTESIAN_POINT('Ctrl Pts',(-97.6345880981528,2.68339810948706,-2.88427413055134));
#44874=CARTESIAN_POINT('Ctrl Pts',(-97.5682969209203,3.63848129491847,-1.99570796166933));
#44875=CARTESIAN_POINT('Ctrl Pts',(-97.5020057436879,4.10834195633222,-0.585596082280521));
#44876=CARTESIAN_POINT('Ctrl Pts',(-97.4357145664554,3.87712562349882,0.698254662551813));
#44877=CARTESIAN_POINT('Ctrl Pts',(-97.3694233892229,3.64590929066542,1.98210540738416));
#44878=CARTESIAN_POINT('Ctrl Pts',(-97.3031322119904,2.71361596358488,3.13969501766003));
#44879=CARTESIAN_POINT('Ctrl Pts',(-97.2368410347579,1.50854215384415,3.63922563799522));
#44880=CARTESIAN_POINT('Ctrl Pts',(-97.1705498575254,0.303468344103431,
4.1387562583304));
#44881=CARTESIAN_POINT('Ctrl Pts',(-97.1042586802929,-1.17438594829749,
3.98022788872488));
#44882=CARTESIAN_POINT('Ctrl Pts',(-97.0379675030604,-2.24609294421075,
3.23646862492642));
#44883=CARTESIAN_POINT('Ctrl Pts',(-96.9740328427185,-3.27970293018969,
2.51914849437028));
#44884=CARTESIAN_POINT('Ctrl Pts',(-96.9100981823766,-3.93552781346536,
1.25746548024999));
#44885=CARTESIAN_POINT('Ctrl Pts',(-96.8461635220347,-3.93927071217365,
-0.000864176983421456));
#44886=CARTESIAN_POINT('Origin',(-54.75,0.,0.));
#44887=CARTESIAN_POINT('',(-95.412836477965,-3.93296026185221,0.00363216645671877));
#44888=CARTESIAN_POINT('',(-95.5961635220347,-3.93231500343917,0.00363103561394379));
#44889=CARTESIAN_POINT('',(-54.75,-3.933,-4.81653586104654E-16));
#44890=CARTESIAN_POINT('Ctrl Pts',(-95.412836477965,-3.93296026185221,0.00363216645671877));
#44891=CARTESIAN_POINT('Ctrl Pts',(-95.4283227235693,-3.93578918688,0.309699076233004));
#44892=CARTESIAN_POINT('Ctrl Pts',(-95.4438089691735,-3.90308854705616,
0.615168125721136));
#44893=CARTESIAN_POINT('Ctrl Pts',(-95.4592952147778,-3.83256747610089,
0.911640946480624));
#44894=CARTESIAN_POINT('Ctrl Pts',(-95.5255863920103,-3.53069154485299,
2.18073694352288));
#44895=CARTESIAN_POINT('Ctrl Pts',(-95.5918775692427,-2.53579579755656,
3.28498646493961));
#44896=CARTESIAN_POINT('Ctrl Pts',(-95.6581687464752,-1.30493636191566,
3.71709614692932));
#44897=CARTESIAN_POINT('Ctrl Pts',(-95.7244599237077,-0.0740769262747676,
4.14920582891902));
#44898=CARTESIAN_POINT('Ctrl Pts',(-95.7907511009402,1.39274619771061,3.90917567148172));
#44899=CARTESIAN_POINT('Ctrl Pts',(-95.8570422781727,2.42167296098772,3.10727577536778));
#44900=CARTESIAN_POINT('Ctrl Pts',(-95.9233334554052,3.45059972426483,2.30537587925383));
#44901=CARTESIAN_POINT('Ctrl Pts',(-95.9896246326377,4.0416301268337,0.941606244463238));
#44902=CARTESIAN_POINT('Ctrl Pts',(-96.0559158098702,3.92324419498091,-0.357515958685805));
#44903=CARTESIAN_POINT('Ctrl Pts',(-96.1222069871026,3.80485826312812,-1.65663816183485));
#44904=CARTESIAN_POINT('Ctrl Pts',(-96.1884981643351,2.97705599685373,-2.89111293334231));
#44905=CARTESIAN_POINT('Ctrl Pts',(-96.2547893415676,1.82013060713598,-3.49382129582113));
#44906=CARTESIAN_POINT('Ctrl Pts',(-96.3210805188001,0.663205217418252,
-4.09652965829995));
#44907=CARTESIAN_POINT('Ctrl Pts',(-96.3873716960326,-0.822843295742819,
-4.0674716117501));
#44908=CARTESIAN_POINT('Ctrl Pts',(-96.4536628732651,-1.9553227197697,-3.41999645258864));
#44909=CARTESIAN_POINT('Ctrl Pts',(-96.5199540504975,-3.0878021437966,-2.77252129342716));
#44910=CARTESIAN_POINT('Ctrl Pts',(-96.58624522773,-3.86671247868932,-1.50662902165405));
#44911=CARTESIAN_POINT('Ctrl Pts',(-96.6525364049625,-3.93422151694052,
-0.203871846532809));
#44912=CARTESIAN_POINT('Ctrl Pts',(-96.65596976263,-3.93771795015805,-0.136399348338936));
#44913=CARTESIAN_POINT('Ctrl Pts',(-96.6594031202975,-3.93930610694812,
-0.0688279630241185));
#44914=CARTESIAN_POINT('Ctrl Pts',(-96.662836477965,-3.93902708289076,-0.00124319021292452));
#44915=CARTESIAN_POINT('Ctrl Pts',(-96.8461635220347,-3.93927071217365,
-0.000864176983421456));
#44916=CARTESIAN_POINT('Ctrl Pts',(-96.8438070051441,-3.93940866870581,
-0.0472439508851525));
#44917=CARTESIAN_POINT('Ctrl Pts',(-96.8414504882536,-3.93866075402094,
-0.0936191691598041));
#44918=CARTESIAN_POINT('Ctrl Pts',(-96.839093971363,-3.93701323328378,-0.139962406076981));
#44919=CARTESIAN_POINT('Ctrl Pts',(-96.7728027941305,-3.89066682701792,
-1.44364401529055));
#44920=CARTESIAN_POINT('Ctrl Pts',(-96.706511616898,-3.13241431506057,-2.72201707572629));
#44921=CARTESIAN_POINT('Ctrl Pts',(-96.6402204396655,-2.01059767985446,
-3.38779569099589));
#44922=CARTESIAN_POINT('Ctrl Pts',(-96.573929262433,-0.888781044648358,
-4.05357430626548));
#44923=CARTESIAN_POINT('Ctrl Pts',(-96.5076380852006,0.596599713806542,
-4.1067584763689));
#44924=CARTESIAN_POINT('Ctrl Pts',(-96.4413469079681,1.76315915013021,-3.52291533895985));
#44925=CARTESIAN_POINT('Ctrl Pts',(-96.3750557307357,2.92971858645389,-2.93907220155078));
#44926=CARTESIAN_POINT('Ctrl Pts',(-96.3087645535031,3.77745670064637,-1.71820175662924));
#44927=CARTESIAN_POINT('Ctrl Pts',(-96.2424733762706,3.91692173272892,-0.421173139982053));
#44928=CARTESIAN_POINT('Ctrl Pts',(-96.1761821990382,4.05638676481147,0.875855476665131));
#44929=CARTESIAN_POINT('Ctrl Pts',(-96.1098910218057,3.48757871478409,2.24904226503793));
#44930=CARTESIAN_POINT('Ctrl Pts',(-96.0435998445732,2.47180858478833,3.06754380479451));
#44931=CARTESIAN_POINT('Ctrl Pts',(-95.9773086673407,1.45603845479257,3.88604534455109));
#44932=CARTESIAN_POINT('Ctrl Pts',(-95.9110174901082,-0.00669375517154278,
4.14986163569144));
#44933=CARTESIAN_POINT('Ctrl Pts',(-95.8447263128757,-1.24440736615255,
3.73779520322231));
#44934=CARTESIAN_POINT('Ctrl Pts',(-95.7784351356432,-2.48212097713351,
3.3257287707532));
#44935=CARTESIAN_POINT('Ctrl Pts',(-95.7121439584108,-3.4948159891314,2.23777961467462));
#44936=CARTESIAN_POINT('Ctrl Pts',(-95.6458527811783,-3.81725927396492,
0.973752694217182));
#44937=CARTESIAN_POINT('Ctrl Pts',(-95.6292896947971,-3.8978228753777,0.657931072913059));
#44938=CARTESIAN_POINT('Ctrl Pts',(-95.6127266084159,-3.93529627055665,
0.331117480300956));
#44939=CARTESIAN_POINT('Ctrl Pts',(-95.5961635220347,-3.93231500343917,
0.00363103561394379));
#44940=CARTESIAN_POINT('Origin',(-54.75,0.,0.));
#44941=CARTESIAN_POINT('',(-94.162836477965,-3.92651713604259,-0.000413326683059989));
#44942=CARTESIAN_POINT('',(-94.3461635220346,-3.92661200070631,-0.000762584109358684));
#44943=CARTESIAN_POINT('',(-54.75,-3.933,-4.81653586104654E-16));
#44944=CARTESIAN_POINT('Ctrl Pts',(-94.162836477965,-3.92651713604259,-0.000413326683059989));
#44945=CARTESIAN_POINT('Ctrl Pts',(-94.197242326841,-3.92587933456817,0.682394578314803));
#44946=CARTESIAN_POINT('Ctrl Pts',(-94.231648175717,-3.75679084115549,1.36549820367841));
#44947=CARTESIAN_POINT('Ctrl Pts',(-94.266054024593,-3.42106576242298,1.95345123393027));
#44948=CARTESIAN_POINT('Ctrl Pts',(-94.3323452018255,-2.7742103171223,3.08628474352482));
#44949=CARTESIAN_POINT('Ctrl Pts',(-94.398636379058,-1.50874440243043,3.86588757336226));
#44950=CARTESIAN_POINT('Ctrl Pts',(-94.4649275562905,-0.206024358730012,
3.93410938304673));
#44951=CARTESIAN_POINT('Ctrl Pts',(-94.531218733523,1.09669568497042,4.0023311927312));
#44952=CARTESIAN_POINT('Ctrl Pts',(-94.5975099107554,2.43666985767939,3.35917198226269));
#44953=CARTESIAN_POINT('Ctrl Pts',(-94.6638010879879,3.19831264878829,2.300099753221));
#44954=CARTESIAN_POINT('Ctrl Pts',(-94.7300922652204,3.95995543989718,1.24102752417931));
#44955=CARTESIAN_POINT('Ctrl Pts',(-94.796383442453,4.14326684940601,-0.233957723435546));
#44956=CARTESIAN_POINT('Ctrl Pts',(-94.8626746196855,3.66403342759226,-1.44724625259593));
#44957=CARTESIAN_POINT('Ctrl Pts',(-94.928965796918,3.18480000577852,-2.66053478175629));
#44958=CARTESIAN_POINT('Ctrl Pts',(-94.9952569741504,2.04302175264223,-3.61212659246219));
#44959=CARTESIAN_POINT('Ctrl Pts',(-95.0615481513829,0.763232769865172,
-3.86485942993667));
#44960=CARTESIAN_POINT('Ctrl Pts',(-95.1278393286153,-0.516556212911885,
-4.11759226741114));
#44961=CARTESIAN_POINT('Ctrl Pts',(-95.1941305058479,-1.93435592532971,
-3.67146613165418));
#44962=CARTESIAN_POINT('Ctrl Pts',(-95.2604216830804,-2.83882772393893,
-2.73143182744182));
#44963=CARTESIAN_POINT('Ctrl Pts',(-95.3112266147086,-3.53200636107257,
-2.01099842216069));
#44964=CARTESIAN_POINT('Ctrl Pts',(-95.3620315463368,-3.92367955261569,
-1.00046584556025));
#44965=CARTESIAN_POINT('Ctrl Pts',(-95.412836477965,-3.93296026185221,0.00363216645671877));
#44966=CARTESIAN_POINT('Ctrl Pts',(-95.5961635220347,-3.93231500343917,
0.00363103561394379));
#44967=CARTESIAN_POINT('Ctrl Pts',(-95.5464354311834,-3.92336421258671,
-0.979596081550714));
#44968=CARTESIAN_POINT('Ctrl Pts',(-95.4967073403321,-3.54975216954202,
-1.96888833598873));
#44969=CARTESIAN_POINT('Ctrl Pts',(-95.4469792494808,-2.88280552298465,
-2.68497578961443));
#44970=CARTESIAN_POINT('Ctrl Pts',(-95.3806880722483,-1.9937169295017,-3.63957266815216));
#44971=CARTESIAN_POINT('Ctrl Pts',(-95.3143968950158,-0.583348184866643,
-4.10866174039123));
#44972=CARTESIAN_POINT('Ctrl Pts',(-95.2481057177833,0.700375861699437,
-3.87674300496115));
#44973=CARTESIAN_POINT('Ctrl Pts',(-95.1818145405509,1.98409990826552,-3.64482426953107));
#44974=CARTESIAN_POINT('Ctrl Pts',(-95.1155233633184,3.14117925676262,-2.71189772643183));
#44975=CARTESIAN_POINT('Ctrl Pts',(-95.049232186086,3.64005046659153,-1.50655078733948));
#44976=CARTESIAN_POINT('Ctrl Pts',(-94.9829410088535,4.13892167642045,-0.30120384824712));
#44977=CARTESIAN_POINT('Ctrl Pts',(-94.916649831621,3.97958474758117,1.17656348683836));
#44978=CARTESIAN_POINT('Ctrl Pts',(-94.8503586543885,3.23523922876354,2.24786338704912));
#44979=CARTESIAN_POINT('Ctrl Pts',(-94.784067477156,2.49089370994594,3.31916328725984));
#44980=CARTESIAN_POINT('Ctrl Pts',(-94.7177762999235,1.16153960115003,3.98399575259588));
#44981=CARTESIAN_POINT('Ctrl Pts',(-94.651485122691,-0.14211645528021,3.93693606594075));
#44982=CARTESIAN_POINT('Ctrl Pts',(-94.5851939454585,-1.44577251171053,
3.88987637928562));
#44983=CARTESIAN_POINT('Ctrl Pts',(-94.5189027682261,-2.72373051577518,
3.13092454063924));
#44984=CARTESIAN_POINT('Ctrl Pts',(-94.4526115909936,-3.3888952484088,2.00874380384326));
#44985=CARTESIAN_POINT('Ctrl Pts',(-94.4171289013406,-3.74492805339839,
1.40809085905339));
#44986=CARTESIAN_POINT('Ctrl Pts',(-94.3816462116876,-3.92539680852964,
0.703373559516597));
#44987=CARTESIAN_POINT('Ctrl Pts',(-94.3461635220346,-3.92661200070631,
-0.000762584109358684));
#44988=CARTESIAN_POINT('Origin',(-54.75,0.,0.));
#44989=CARTESIAN_POINT('',(-92.912836477965,-3.93448228467576,-0.0034881012485255));
#44990=CARTESIAN_POINT('',(-93.0961635220346,-3.9351223687927,-0.00336391575034791));
#44991=CARTESIAN_POINT('',(-54.75,-3.933,-4.81653586104654E-16));
#44992=CARTESIAN_POINT('Ctrl Pts',(-92.912836477965,-3.93448228467576,-0.0034881012485255));
#44993=CARTESIAN_POINT('Ctrl Pts',(-92.9661619301128,-3.92475942763249,
1.04937969788364));
#44994=CARTESIAN_POINT('Ctrl Pts',(-93.0194873822606,-3.48876179764117,
2.10935079459708));
#44995=CARTESIAN_POINT('Ctrl Pts',(-93.0728128344084,-2.73298463514744,
2.83733284233882));
#44996=CARTESIAN_POINT('Ctrl Pts',(-93.1391040116408,-1.79344533807233,
3.74231882942762));
#44997=CARTESIAN_POINT('Ctrl Pts',(-93.2053951888733,-0.359717087789233,
4.13424721303581));
#44998=CARTESIAN_POINT('Ctrl Pts',(-93.2716863661058,0.909543885604364,
3.83306569136588));
#44999=CARTESIAN_POINT('Ctrl Pts',(-93.3379775433383,2.17880485899794,3.53188416969595));
#45000=CARTESIAN_POINT('Ctrl Pts',(-93.4042687205708,3.28359855550202,2.53759274274792));
#45001=CARTESIAN_POINT('Ctrl Pts',(-93.4705598978033,3.71638161672134,1.30696991283736));
#45002=CARTESIAN_POINT('Ctrl Pts',(-93.5368510750358,4.14916467794067,0.0763470829267855));
#45003=CARTESIAN_POINT('Ctrl Pts',(-93.6031422522682,3.90993710387521,-1.39060714994632));
#45004=CARTESIAN_POINT('Ctrl Pts',(-93.6694334295007,3.10860028765036,-2.41997250517161));
#45005=CARTESIAN_POINT('Ctrl Pts',(-93.7357246067331,2.3072634714255,-3.4493378603969));
#45006=CARTESIAN_POINT('Ctrl Pts',(-93.8020157839657,0.943817413041241,
-4.04111433797437));
#45007=CARTESIAN_POINT('Ctrl Pts',(-93.8683069611982,-0.355369368517493,
-3.92343921656573));
#45008=CARTESIAN_POINT('Ctrl Pts',(-93.9345981384307,-1.65455615007621,
-3.80576409515709));
#45009=CARTESIAN_POINT('Ctrl Pts',(-94.0008893156632,-2.8894836548094,-2.97863737476235));
#45010=CARTESIAN_POINT('Ctrl Pts',(-94.0671804928956,-3.49282491922127,
-1.82204191988916));
#45011=CARTESIAN_POINT('Ctrl Pts',(-94.0990658212521,-3.78302544257763,
-1.26573220577906));
#45012=CARTESIAN_POINT('Ctrl Pts',(-94.1309511496085,-3.92710821314438,
-0.633199755923574));
#45013=CARTESIAN_POINT('Ctrl Pts',(-94.162836477965,-3.92651713604259,-0.000413326683059989));
#45014=CARTESIAN_POINT('Ctrl Pts',(-94.3461635220346,-3.92661200070631,
-0.000762584109358684));
#45015=CARTESIAN_POINT('Ctrl Pts',(-94.3153550344551,-3.92766711331045,
-0.612141536701368));
#45016=CARTESIAN_POINT('Ctrl Pts',(-94.2845465468755,-3.79358484768176,
-1.22308236195667));
#45017=CARTESIAN_POINT('Ctrl Pts',(-94.253738059296,-3.52195012897364,-1.76508638972403));
#45018=CARTESIAN_POINT('Ctrl Pts',(-94.1874468820636,-2.93746881570228,
-2.93132621154973));
#45019=CARTESIAN_POINT('Ctrl Pts',(-94.1211557048312,-1.71613472795704,
-3.77839622025559));
#45020=CARTESIAN_POINT('Ctrl Pts',(-94.0548645275987,-0.419029999513912,
-3.91715158420935));
#45021=CARTESIAN_POINT('Ctrl Pts',(-93.9885733503663,0.878074728929215,
-4.05590694816311));
#45022=CARTESIAN_POINT('Ctrl Pts',(-93.9222821731337,2.25095009807022,-3.48634766736474));
#45023=CARTESIAN_POINT('Ctrl Pts',(-93.8559909959012,3.06889575388203,-2.47012986014325));
#45024=CARTESIAN_POINT('Ctrl Pts',(-93.7896998186686,3.88684140969384,-1.45391205292175));
#45025=CARTESIAN_POINT('Ctrl Pts',(-93.7234086414362,4.14985735217646,0.00896428072286667));
#45026=CARTESIAN_POINT('Ctrl Pts',(-93.6571174642038,3.73711378733167,1.24645225127237));
#45027=CARTESIAN_POINT('Ctrl Pts',(-93.5908262869713,3.32437022248691,2.48394022182179));
#45028=CARTESIAN_POINT('Ctrl Pts',(-93.5245351097388,2.23586715031477,3.49603982927613));
#45029=CARTESIAN_POINT('Ctrl Pts',(-93.4582439325063,0.971663999667894,
3.81779147491267));
#45030=CARTESIAN_POINT('Ctrl Pts',(-93.3919527552738,-0.292539150979056,
4.13954312054923));
#45031=CARTESIAN_POINT('Ctrl Pts',(-93.3256615780413,-1.73244238010076,
3.77094680436794));
#45032=CARTESIAN_POINT('Ctrl Pts',(-93.2593704008089,-2.68655266598184,
2.88133605243684));
#45033=CARTESIAN_POINT('Ctrl Pts',(-93.2049681078841,-3.46954958083475,
2.15127110660222));
#45034=CARTESIAN_POINT('Ctrl Pts',(-93.1505658149594,-3.92537598800762,
1.07031477828723));
#45035=CARTESIAN_POINT('Ctrl Pts',(-93.0961635220346,-3.9351223687927,-0.00336391575034791));
#45036=CARTESIAN_POINT('Origin',(-54.75,0.,0.));
#45037=CARTESIAN_POINT('',(-91.662836477965,-3.93817602267047,0.00205778069578805));
#45038=CARTESIAN_POINT('',(-91.8461635220346,-3.93771195638885,0.00236553390519242));
#45039=CARTESIAN_POINT('',(-54.75,-3.933,-4.81653586104654E-16));
#45040=CARTESIAN_POINT('Ctrl Pts',(-91.662836477965,-3.93817602267047,0.00205778069578805));
#45041=CARTESIAN_POINT('Ctrl Pts',(-91.6687903561521,-3.93892001361361,
0.11932550450386));
#45042=CARTESIAN_POINT('Ctrl Pts',(-91.6747442343391,-3.93413809733793,
0.236531698311863));
#45043=CARTESIAN_POINT('Ctrl Pts',(-91.6806981125262,-3.92363306365089,
0.353222671967719));
#45044=CARTESIAN_POINT('Ctrl Pts',(-91.7469892897586,-3.80666878791298,
1.65247364301858));
#45045=CARTESIAN_POINT('Ctrl Pts',(-91.8132804669911,-2.9802178610021,2.88785351129623));
#45046=CARTESIAN_POINT('Ctrl Pts',(-91.8795716442236,-1.82395268720563,
3.49182749702814));
#45047=CARTESIAN_POINT('Ctrl Pts',(-91.9458628214561,-0.667687513409183,
4.09580148276003));
#45048=CARTESIAN_POINT('Ctrl Pts',(-92.0121539986886,0.818391907272832,
4.06836958594621));
#45049=CARTESIAN_POINT('Ctrl Pts',(-92.0784451759211,1.95157916331609,3.42213404814553));
#45050=CARTESIAN_POINT('Ctrl Pts',(-92.1447363531536,3.0847664193594,2.77589851034481));
#45051=CARTESIAN_POINT('Ctrl Pts',(-92.2110275303861,3.8650615107639,1.51085933155719));
#45052=CARTESIAN_POINT('Ctrl Pts',(-92.2773187076185,3.93399607145912,0.208176809252815));
#45053=CARTESIAN_POINT('Ctrl Pts',(-92.343609884851,4.00293063215433,-1.09450571305151));
#45054=CARTESIAN_POINT('Ctrl Pts',(-92.4099010620835,3.36050466214028,-2.43483157887261));
#45055=CARTESIAN_POINT('Ctrl Pts',(-92.476192239316,2.30184931157926,-3.19705370942506));
#45056=CARTESIAN_POINT('Ctrl Pts',(-92.5424834165485,1.24319396101821,-3.95927583997753));
#45057=CARTESIAN_POINT('Ctrl Pts',(-92.608774593781,-0.231690770089837,
-4.14339423526136));
#45058=CARTESIAN_POINT('Ctrl Pts',(-92.6750657710135,-1.44524132210368,
-3.66482471546054));
#45059=CARTESIAN_POINT('Ctrl Pts',(-92.741356948246,-2.6587918741175,-3.18625519565973));
#45060=CARTESIAN_POINT('Ctrl Pts',(-92.8076481254784,-3.61100824703711,
-2.04499776077428));
#45061=CARTESIAN_POINT('Ctrl Pts',(-92.8739393027109,-3.86444126156338,
-0.765347248046856));
#45062=CARTESIAN_POINT('Ctrl Pts',(-92.8869050277956,-3.91400958921899,
-0.515063613856148));
#45063=CARTESIAN_POINT('Ctrl Pts',(-92.8998707528803,-3.93684633198119,
-0.259485826242128));
#45064=CARTESIAN_POINT('Ctrl Pts',(-92.912836477965,-3.93448228467576,-0.0034881012485255));
#45065=CARTESIAN_POINT('Ctrl Pts',(-93.0961635220346,-3.9351223687927,-0.00336391575034791));
#45066=CARTESIAN_POINT('Ctrl Pts',(-93.0842746377269,-3.93725230831076,
-0.238001852698556));
#45067=CARTESIAN_POINT('Ctrl Pts',(-93.0723857534191,-3.91807827642478,
-0.472292223059233));
#45068=CARTESIAN_POINT('Ctrl Pts',(-93.0604968691114,-3.87635922590254,
-0.702496851186307));
#45069=CARTESIAN_POINT('Ctrl Pts',(-92.9942056918789,-3.64373815730172,
-1.98609381519739));
#45070=CARTESIAN_POINT('Ctrl Pts',(-92.9279145146464,-2.71017867745966,
-3.14266255553868));
#45071=CARTESIAN_POINT('Ctrl Pts',(-92.8616233374139,-1.50455896984186,
-3.64087420552191));
#45072=CARTESIAN_POINT('Ctrl Pts',(-92.7953321601814,-0.29893926222404,
-4.13908585550516));
#45073=CARTESIAN_POINT('Ctrl Pts',(-92.729040982949,1.17874067316951,-3.97894041513037));
#45074=CARTESIAN_POINT('Ctrl Pts',(-92.6627498057165,2.24963315697919,-3.23400886411684));
#45075=CARTESIAN_POINT('Ctrl Pts',(-92.596458628484,3.32052564078884,-2.48907731310333));
#45076=CARTESIAN_POINT('Ctrl Pts',(-92.5301674512514,3.98463067301462,-1.15935965145112));
#45077=CARTESIAN_POINT('Ctrl Pts',(-92.463876274019,3.9368577200577,0.144270461940386));
#45078=CARTESIAN_POINT('Ctrl Pts',(-92.3975850967865,3.88908476710079,1.44790057533193));
#45079=CARTESIAN_POINT('Ctrl Pts',(-92.3312939195541,3.12943382896112,2.72544314046279));
#45080=CARTESIAN_POINT('Ctrl Pts',(-92.2650027423216,2.0068893265053,3.38999379134027));
#45081=CARTESIAN_POINT('Ctrl Pts',(-92.1987115650892,0.88434482404947,4.05454444221775));
#45082=CARTESIAN_POINT('Ctrl Pts',(-92.1324203878566,-0.601093242722498,
4.10610317884187));
#45083=CARTESIAN_POINT('Ctrl Pts',(-92.0661292106241,-1.76701310093099,
3.52098386467543));
#45084=CARTESIAN_POINT('Ctrl Pts',(-91.9998380333916,-2.93293295913946,
2.93586455050899));
#45085=CARTESIAN_POINT('Ctrl Pts',(-91.9335468561591,-3.77933460878443,
1.71406718555199));
#45086=CARTESIAN_POINT('Ctrl Pts',(-91.8672556789267,-3.91738026307234,
0.416886733607205));
#45087=CARTESIAN_POINT('Ctrl Pts',(-91.8602249599626,-3.93202112841853,
0.279310187466734));
#45088=CARTESIAN_POINT('Ctrl Pts',(-91.8531942409986,-3.93869417241828,
0.140885707556243));
#45089=CARTESIAN_POINT('Ctrl Pts',(-91.8461635220346,-3.93771195638885,
0.00236553390519242));
#45090=CARTESIAN_POINT('Origin',(-54.75,0.,0.));
#45091=CARTESIAN_POINT('',(-90.412836477965,-3.92810207392459,0.00247836248652517));
#45092=CARTESIAN_POINT('',(-90.5961635220346,-3.92771739568111,0.00220584221594762));
#45093=CARTESIAN_POINT('',(-54.75,-3.933,-4.81653586104654E-16));
#45094=CARTESIAN_POINT('Ctrl Pts',(-90.412836477965,-3.92810207392459,0.00247836248652517));
#45095=CARTESIAN_POINT('Ctrl Pts',(-90.4377099594238,-3.93093227664902,
0.495612161623221));
#45096=CARTESIAN_POINT('Ctrl Pts',(-90.4625834408826,-3.84493247844779,
0.98779472531452));
#45097=CARTESIAN_POINT('Ctrl Pts',(-90.4874569223414,-3.66561490624659,
1.44323595897181));
#45098=CARTESIAN_POINT('Ctrl Pts',(-90.5537480995739,-3.18770943172068,
2.65704817055711));
#45099=CARTESIAN_POINT('Ctrl Pts',(-90.6200392768065,-2.04697315672674,
3.60988882064005));
#45100=CARTESIAN_POINT('Ctrl Pts',(-90.6863304540389,-0.767461497118248,
3.86402193635174));
#45101=CARTESIAN_POINT('Ctrl Pts',(-90.7526216312714,0.512050162490266,
4.11815505206344));
#45102=CARTESIAN_POINT('Ctrl Pts',(-90.8189128085039,1.93033720671331,3.6735806334039));
#45103=CARTESIAN_POINT('Ctrl Pts',(-90.8852039857364,2.83583711136996,2.73453662472151));
#45104=CARTESIAN_POINT('Ctrl Pts',(-90.9514951629689,3.7413370160266,1.79549261603915));
#45105=CARTESIAN_POINT('Ctrl Pts',(-91.0177863402014,4.1340497811168,0.361979017333895));
#45106=CARTESIAN_POINT('Ctrl Pts',(-91.0840775174339,3.83356275918494,-0.907446552451885));
#45107=CARTESIAN_POINT('Ctrl Pts',(-91.1503686946663,3.53307573725307,-2.17687212223768));
#45108=CARTESIAN_POINT('Ctrl Pts',(-91.2166598718987,2.53938892829914,-3.28220966310406));
#45109=CARTESIAN_POINT('Ctrl Pts',(-91.2829510491312,1.30900307251152,-3.71566597399737));
#45110=CARTESIAN_POINT('Ctrl Pts',(-91.3492422263637,0.0786172167238791,
-4.14912228489069));
#45111=CARTESIAN_POINT('Ctrl Pts',(-91.4155334035962,-1.3884676858974,-3.91069736581095));
#45112=CARTESIAN_POINT('Ctrl Pts',(-91.4818245808287,-2.41827132492559,
-3.10992386935904));
#45113=CARTESIAN_POINT('Ctrl Pts',(-91.5421618798742,-3.3555841427113,-2.3810710726494));
#45114=CARTESIAN_POINT('Ctrl Pts',(-91.6024991789196,-3.930636331294,-1.18634707030812));
#45115=CARTESIAN_POINT('Ctrl Pts',(-91.662836477965,-3.93817602267047,0.00205778069578805));
#45116=CARTESIAN_POINT('Ctrl Pts',(-91.8461635220346,-3.93771195638885,
0.00236553390519242));
#45117=CARTESIAN_POINT('Ctrl Pts',(-91.7869030637662,-3.92943306310346,
-1.16519201063766));
#45118=CARTESIAN_POINT('Ctrl Pts',(-91.7276426054977,-3.37728995814469,
-2.33954807026313));
#45119=CARTESIAN_POINT('Ctrl Pts',(-91.6683821472292,-2.46845039605334,
-3.07024678428145));
#45120=CARTESIAN_POINT('Ctrl Pts',(-91.6020909699967,-1.4517852158156,-3.88763631129265));
#45121=CARTESIAN_POINT('Ctrl Pts',(-91.5357997927642,0.0112348035907324,
-4.14985182638249));
#45122=CARTESIAN_POINT('Ctrl Pts',(-91.4695086155317,1.24849676326094,-3.73643125271875));
#45123=CARTESIAN_POINT('Ctrl Pts',(-91.4032174382992,2.48575872293114,-3.32301067905501));
#45124=CARTESIAN_POINT('Ctrl Pts',(-91.3369262610668,3.49726262286522,-2.23395401663771));
#45125=CARTESIAN_POINT('Ctrl Pts',(-91.2706350838343,3.81832253298691,-0.969575014246389));
#45126=CARTESIAN_POINT('Ctrl Pts',(-91.2043439066018,4.1393824431086,0.294803988144949));
#45127=CARTESIAN_POINT('Ctrl Pts',(-91.1380527293693,3.76999836341785,1.7345053305103));
#45128=CARTESIAN_POINT('Ctrl Pts',(-91.0717615521368,2.87986571934768,2.68812873811737));
#45129=CARTESIAN_POINT('Ctrl Pts',(-91.0054703749043,1.9897330752775,3.64175214572446));
#45130=CARTESIAN_POINT('Ctrl Pts',(-90.9391791976719,0.578851866827931,
4.10929761857325));
#45131=CARTESIAN_POINT('Ctrl Pts',(-90.8728880204394,-0.704617630377498,
3.87597428643788));
#45132=CARTESIAN_POINT('Ctrl Pts',(-90.8065968432069,-1.98808712758291,
3.64265095430252));
#45133=CARTESIAN_POINT('Ctrl Pts',(-90.7403056659744,-3.14414491354417,
2.70845881718298));
#45134=CARTESIAN_POINT('Ctrl Pts',(-90.6740144887419,-3.64169685453977,
1.50256670194756));
#45135=CARTESIAN_POINT('Ctrl Pts',(-90.6480641665061,-3.83646837221226,
1.03050857478256));
#45136=CARTESIAN_POINT('Ctrl Pts',(-90.6221138442704,-3.9303300118642,0.516814960462088));
#45137=CARTESIAN_POINT('Ctrl Pts',(-90.5961635220346,-3.92771739568111,
0.00220584221594762));
#45138=CARTESIAN_POINT('Origin',(-54.75,0.,0.));
#45139=CARTESIAN_POINT('',(-89.162836477965,-3.92910621855356,-0.00299364777908595));
#45140=CARTESIAN_POINT('',(-89.3461635220346,-3.92962428827605,-0.00318291295316376));
#45141=CARTESIAN_POINT('',(-54.75,-3.933,-4.81653586104654E-16));
#45142=CARTESIAN_POINT('Ctrl Pts',(-89.162836477965,-3.92910621855356,-0.00299364777908595));
#45143=CARTESIAN_POINT('Ctrl Pts',(-89.2066295626955,-3.92298954530611,
0.864677208853277));
#45144=CARTESIAN_POINT('Ctrl Pts',(-89.2504226474261,-3.63987888166823,
1.73597420126334));
#45145=CARTESIAN_POINT('Ctrl Pts',(-89.2942157321567,-3.11124652009766,
2.41656942075883));
#45146=CARTESIAN_POINT('Ctrl Pts',(-89.3605069093892,-2.31103658313397,
3.44681103531342));
#45147=CARTESIAN_POINT('Ctrl Pts',(-89.4267980866217,-0.948238901927029,
4.04007913123173));
#45148=CARTESIAN_POINT('Ctrl Pts',(-89.4930892638542,0.351075869679159,
3.92382573617834));
#45149=CARTESIAN_POINT('Ctrl Pts',(-89.5593804410867,1.65039064128533,3.80757234112494));
#45150=CARTESIAN_POINT('Ctrl Pts',(-89.6256716183192,2.88622250329074,2.98179745509986));
#45151=CARTESIAN_POINT('Ctrl Pts',(-89.6919627955516,3.49082902954029,1.82586290851347));
#45152=CARTESIAN_POINT('Ctrl Pts',(-89.7582539727841,4.09543555578984,0.669928361927062));
#45153=CARTESIAN_POINT('Ctrl Pts',(-89.8245451500166,4.06881674628351,-0.816165845220666));
#45154=CARTESIAN_POINT('Ctrl Pts',(-89.8908363272491,3.42320130943634,-1.94970650848781));
#45155=CARTESIAN_POINT('Ctrl Pts',(-89.9571275044816,2.77758587258919,-3.08324717175494));
#45156=CARTESIAN_POINT('Ctrl Pts',(-90.0234186817141,1.5129738084012,-3.8642342911415));
#45157=CARTESIAN_POINT('Ctrl Pts',(-90.0897098589465,0.210329197456982,
-3.93388158221159));
#45158=CARTESIAN_POINT('Ctrl Pts',(-90.156001036179,-1.09231541348726,-4.00352887328168));
#45159=CARTESIAN_POINT('Ctrl Pts',(-90.2222922134115,-2.43299257118775,
-3.36183633603528));
#45160=CARTESIAN_POINT('Ctrl Pts',(-90.288583390644,-3.19579381300906,-2.30359818086824));
#45161=CARTESIAN_POINT('Ctrl Pts',(-90.3300010864176,-3.67238015659939,
-1.64242745202328));
#45162=CARTESIAN_POINT('Ctrl Pts',(-90.3714187821913,-3.92338940530952,
-0.818655812163256));
#45163=CARTESIAN_POINT('Ctrl Pts',(-90.412836477965,-3.92810207392459,0.00247836248652517));
#45164=CARTESIAN_POINT('Ctrl Pts',(-90.5961635220346,-3.92771739568111,
0.00220584221594762));
#45165=CARTESIAN_POINT('Ctrl Pts',(-90.5558226670379,-3.92365597518519,
-0.797775430869884));
#45166=CARTESIAN_POINT('Ctrl Pts',(-90.5154818120412,-3.68645491319269,
-1.599969110314));
#45167=CARTESIAN_POINT('Ctrl Pts',(-90.4751409570445,-3.23277753135463,
-2.25140225347118));
#45168=CARTESIAN_POINT('Ctrl Pts',(-90.408849779812,-2.48726017114393,-3.32188700030313));
#45169=CARTESIAN_POINT('Ctrl Pts',(-90.3425586025795,-1.15717935469258,
-3.98526440061574));
#45170=CARTESIAN_POINT('Ctrl Pts',(-90.276267425347,0.146424425412479,-3.9367781956581));
#45171=CARTESIAN_POINT('Ctrl Pts',(-90.2099762481145,1.45002820551758,-3.88829199070047));
#45172=CARTESIAN_POINT('Ctrl Pts',(-90.1436850708821,2.72715494927636,-3.12794218047255));
#45173=CARTESIAN_POINT('Ctrl Pts',(-90.0773938936496,3.39109131946141,-2.00503424839575));
#45174=CARTESIAN_POINT('Ctrl Pts',(-90.0111027164171,4.05502768964645,-0.88212631631897));
#45175=CARTESIAN_POINT('Ctrl Pts',(-89.9448115391846,4.10577368625775,0.603339737606724));
#45176=CARTESIAN_POINT('Ctrl Pts',(-89.8785203619521,3.52001654635439,1.76893928317445));
#45177=CARTESIAN_POINT('Ctrl Pts',(-89.8122291847196,2.93425940645103,2.93453882874219));
#45178=CARTESIAN_POINT('Ctrl Pts',(-89.7459380074871,1.71199913003302,3.78027186595199));
#45179=CARTESIAN_POINT('Ctrl Pts',(-89.6796468302546,0.414743342903526,
3.91760776924945));
#45180=CARTESIAN_POINT('Ctrl Pts',(-89.6133556530222,-0.882512444225967,
4.05494367254691));
#45181=CARTESIAN_POINT('Ctrl Pts',(-89.5470644757897,-2.25476374206692,
3.48388244193204));
#45182=CARTESIAN_POINT('Ctrl Pts',(-89.4807732985572,-3.07159689558824,
2.46677019302147));
#45183=CARTESIAN_POINT('Ctrl Pts',(-89.4359033730497,-3.62447956083405,
1.77832637973155));
#45184=CARTESIAN_POINT('Ctrl Pts',(-89.3910334475421,-3.92290235831991,
0.885528271771005));
#45185=CARTESIAN_POINT('Ctrl Pts',(-89.3461635220346,-3.92962428827605,
-0.00318291295316376));
#45186=CARTESIAN_POINT('Origin',(-54.75,0.,0.));
#45187=CARTESIAN_POINT('',(-87.912836477965,-3.93898829629484,-0.00129309091083552));
#45188=CARTESIAN_POINT('',(-88.0961635220347,-3.93924257493437,-0.000916068792095346));
#45189=CARTESIAN_POINT('',(-54.75,-3.933,-4.81653586104654E-16));
#45190=CARTESIAN_POINT('Ctrl Pts',(-87.912836477965,-3.93898829629484,-0.00129309091083552));
#45191=CARTESIAN_POINT('Ctrl Pts',(-87.9755491659674,-3.93371149202149,
1.2332226163925));
#45192=CARTESIAN_POINT('Ctrl Pts',(-88.0382618539697,-3.30606438542729,
2.47236114778859));
#45193=CARTESIAN_POINT('Ctrl Pts',(-88.1009745419721,-2.30534636056446,
3.19453295991741));
#45194=CARTESIAN_POINT('Ctrl Pts',(-88.1672657192045,-1.24752571757992,
3.95791308465947));
#45195=CARTESIAN_POINT('Ctrl Pts',(-88.2335568964369,0.227156656004045,
4.14364528590165));
#45196=CARTESIAN_POINT('Ctrl Pts',(-88.2998480736694,1.44123016380054,3.66640399971388));
#45197=CARTESIAN_POINT('Ctrl Pts',(-88.3661392509019,2.65530367159704,3.1891627135261));
#45198=CARTESIAN_POINT('Ctrl Pts',(-88.4324304281344,3.60876831360607,2.04894793990836));
#45199=CARTESIAN_POINT('Ctrl Pts',(-88.4987216053669,3.86360145442727,0.769575516446496));
#45200=CARTESIAN_POINT('Ctrl Pts',(-88.5650127825994,4.11843459524847,-0.509796907015349));
#45201=CARTESIAN_POINT('Ctrl Pts',(-88.6313039598319,3.67463623488187,-1.92832698032131));
#45202=CARTESIAN_POINT('Ctrl Pts',(-88.6975951370643,2.73608779569937,-2.83434053148019));
#45203=CARTESIAN_POINT('Ctrl Pts',(-88.7638863142968,1.79753935651686,-3.74035408263909));
#45204=CARTESIAN_POINT('Ctrl Pts',(-88.8301774915293,0.364240838518444,
-4.13385111165089));
#45205=CARTESIAN_POINT('Ctrl Pts',(-88.8964686687618,-0.905348947651138,
-3.83405867940925));
#45206=CARTESIAN_POINT('Ctrl Pts',(-88.9627598459943,-2.1749387338207,-3.53426624716762));
#45207=CARTESIAN_POINT('Ctrl Pts',(-89.0290510232268,-3.28081978816143,
-2.54118435367256));
#45208=CARTESIAN_POINT('Ctrl Pts',(-89.0953422004593,-3.7149492189716,-1.31103584032961));
#45209=CARTESIAN_POINT('Ctrl Pts',(-89.1178402929612,-3.86228532763525,
-0.89354446063647));
#45210=CARTESIAN_POINT('Ctrl Pts',(-89.1403383854631,-3.93224857496374,
-0.448747567920103));
#45211=CARTESIAN_POINT('Ctrl Pts',(-89.162836477965,-3.92910621855356,-0.00299364777908595));
#45212=CARTESIAN_POINT('Ctrl Pts',(-89.3461635220346,-3.92962428827605,
-0.00318291295316376));
#45213=CARTESIAN_POINT('Ctrl Pts',(-89.3247422703097,-3.93283338996363,
-0.427460550667744));
#45214=CARTESIAN_POINT('Ctrl Pts',(-89.3033210185847,-3.86955855712855,
-0.850806704224785));
#45215=CARTESIAN_POINT('Ctrl Pts',(-89.2818997668597,-3.73574759958786,
-1.25054090150623));
#45216=CARTESIAN_POINT('Ctrl Pts',(-89.2156085896273,-3.32165014086451,
-2.48757647991708));
#45217=CARTESIAN_POINT('Ctrl Pts',(-89.1493174123949,-2.23204021421619,
-3.49848436953255));
#45218=CARTESIAN_POINT('Ctrl Pts',(-89.0830262351624,-0.967485738578175,
-3.81885244802863));
#45219=CARTESIAN_POINT('Ctrl Pts',(-89.0167350579299,0.297068737059861,
-4.13922052652472));
#45220=CARTESIAN_POINT('Ctrl Pts',(-88.9504438806973,1.73656776168761,-3.76904879390135));
#45221=CARTESIAN_POINT('Ctrl Pts',(-88.8841527034648,2.6897040055491,-2.87839452415744));
#45222=CARTESIAN_POINT('Ctrl Pts',(-88.8178615262323,3.6428402494106,-1.98774025441354));
#45223=CARTESIAN_POINT('Ctrl Pts',(-88.7515703489999,4.10961371250589,-0.576603447549069));
#45224=CARTESIAN_POINT('Ctrl Pts',(-88.6852791717675,3.8755881866824,0.706738198638142));
#45225=CARTESIAN_POINT('Ctrl Pts',(-88.618987994535,3.6415626608589,1.99007984482537));
#45226=CARTESIAN_POINT('Ctrl Pts',(-88.5526968173024,2.70673814611665,3.14562633033533));
#45227=CARTESIAN_POINT('Ctrl Pts',(-88.4864056400699,1.50057398425297,3.64251841339884));
#45228=CARTESIAN_POINT('Ctrl Pts',(-88.4201144628374,0.294409822389292,
4.13941049646235));
#45229=CARTESIAN_POINT('Ctrl Pts',(-88.353823285605,-1.18309398659577,3.97764817707937));
#45230=CARTESIAN_POINT('Ctrl Pts',(-88.2875321083725,-2.25317067599549,
3.23154523084553));
#45231=CARTESIAN_POINT('Ctrl Pts',(-88.2237425795933,-3.28286558600009,
2.5135981774363));
#45232=CARTESIAN_POINT('Ctrl Pts',(-88.159953050814,-3.93530353798598,1.25458118357524));
#45233=CARTESIAN_POINT('Ctrl Pts',(-88.0961635220347,-3.93924257493437,
-0.000916068792095346));
#45234=CARTESIAN_POINT('Origin',(-54.75,0.,0.));
#45235=CARTESIAN_POINT('',(-86.662836477965,-3.93304779575148,0.00362946431549549));
#45236=CARTESIAN_POINT('',(-86.8461635220346,-3.93240142136994,0.00363335402696072));
#45237=CARTESIAN_POINT('',(-54.75,-3.933,-4.81653586104654E-16));
#45238=CARTESIAN_POINT('Ctrl Pts',(-86.662836477965,-3.93304779575148,0.00362946431549549));
#45239=CARTESIAN_POINT('Ctrl Pts',(-86.6781775920066,-3.93585383828323,
0.306810777743879));
#45240=CARTESIAN_POINT('Ctrl Pts',(-86.6935187060482,-3.90377069809062,
0.609404500676993));
#45241=CARTESIAN_POINT('Ctrl Pts',(-86.7088598200898,-3.83455345189039,
0.903251071829943));
#45242=CARTESIAN_POINT('Ctrl Pts',(-86.7751509973223,-3.53545569908325,
2.17300469432574));
#45243=CARTESIAN_POINT('Ctrl Pts',(-86.8414421745548,-2.54297901833069,
3.27942893109026));
#45244=CARTESIAN_POINT('Ctrl Pts',(-86.9077333517873,-1.31306821568301,
3.71423135185862));
#45245=CARTESIAN_POINT('Ctrl Pts',(-86.9740245290198,-0.0831574130353308,
4.14903377262697));
#45246=CARTESIAN_POINT('Ctrl Pts',(-87.0403157062523,1.38418751150747,3.91221437739916));
#45247=CARTESIAN_POINT('Ctrl Pts',(-87.1066068834848,2.41486679318088,3.11256823947022));
#45248=CARTESIAN_POINT('Ctrl Pts',(-87.1728980607172,3.44554607485426,2.31292210154131));
#45249=CARTESIAN_POINT('Ctrl Pts',(-87.2391892379497,4.03955971365827,0.950449220911299));
#45250=CARTESIAN_POINT('Ctrl Pts',(-87.3054804151822,3.92401723409042,-0.348928962294304));
#45251=CARTESIAN_POINT('Ctrl Pts',(-87.3717715924147,3.80847475452257,-1.64830714549996));
#45252=CARTESIAN_POINT('Ctrl Pts',(-87.4380627696472,2.98337615658278,-2.88459063128121));
#45253=CARTESIAN_POINT('Ctrl Pts',(-87.5043539468797,1.82777258324076,-3.48982951705665));
#45254=CARTESIAN_POINT('Ctrl Pts',(-87.5706451241122,0.672169009898779,
-4.09506840283207));
#45255=CARTESIAN_POINT('Ctrl Pts',(-87.6369363013446,-0.813939538845411,
-4.06926268860171));
#45256=CARTESIAN_POINT('Ctrl Pts',(-87.7032274785771,-1.94783327000578,
-3.42426754597608));
#45257=CARTESIAN_POINT('Ctrl Pts',(-87.7695186558095,-3.08172700116616,
-2.77927240335044));
#45258=CARTESIAN_POINT('Ctrl Pts',(-87.8358098330421,-3.86340591474271,
-1.51508783232952));
#45259=CARTESIAN_POINT('Ctrl Pts',(-87.9021010102746,-3.93376591533843,
-0.212481522698077));
#45260=CARTESIAN_POINT('Ctrl Pts',(-87.9056794995047,-3.93756404526878,
-0.142165036481684));
#45261=CARTESIAN_POINT('Ctrl Pts',(-87.9092579887349,-3.93928939943462,
-0.0717365897266798));
#45262=CARTESIAN_POINT('Ctrl Pts',(-87.912836477965,-3.93898829629484,-0.00129309091083552));
#45263=CARTESIAN_POINT('Ctrl Pts',(-88.0961635220347,-3.93924257493437,
-0.000916068792095346));
#45264=CARTESIAN_POINT('Ctrl Pts',(-88.0936618735815,-3.93939705304194,
-0.0501531899855988));
#45265=CARTESIAN_POINT('Ctrl Pts',(-88.0911602251283,-3.93855414570549,
-0.0993848978486387));
#45266=CARTESIAN_POINT('Ctrl Pts',(-88.0886585766751,-3.93669749276575,
-0.148578345051743));
#45267=CARTESIAN_POINT('Ctrl Pts',(-88.0223673994425,-3.88749805032196,
-1.45215540163056));
#45268=CARTESIAN_POINT('Ctrl Pts',(-87.95607622221,-3.12644959562002,-2.72886594170351));
#45269=CARTESIAN_POINT('Ctrl Pts',(-87.8897850449775,-2.00317857006993,
-3.39218783244369));
#45270=CARTESIAN_POINT('Ctrl Pts',(-87.8234938677451,-0.879907544519845,
-4.05550972318388));
#45271=CARTESIAN_POINT('Ctrl Pts',(-87.7572026905126,0.605586051878377,
-4.10544296459131));
#45272=CARTESIAN_POINT('Ctrl Pts',(-87.6909115132801,1.77086493587776,-3.51904817430013));
#45273=CARTESIAN_POINT('Ctrl Pts',(-87.6246203360477,2.93614381987714,-2.93265338400896));
#45274=CARTESIAN_POINT('Ctrl Pts',(-87.5583291588152,3.78120799147769,-1.70993056201918));
#45275=CARTESIAN_POINT('Ctrl Pts',(-87.4920379815827,3.91783410267256,-0.412599828044509));
#45276=CARTESIAN_POINT('Ctrl Pts',(-87.4257468043502,4.05446021386743,0.884730905930157));
#45277=CARTESIAN_POINT('Ctrl Pts',(-87.3594556271177,3.48264826465663,2.25666955188971));
#45278=CARTESIAN_POINT('Ctrl Pts',(-87.2931644498852,2.4650892515505,3.07294608739832));
#45279=CARTESIAN_POINT('Ctrl Pts',(-87.2268732726527,1.44753023844436,3.88922262290694));
#45280=CARTESIAN_POINT('Ctrl Pts',(-87.1605820954203,-0.0157758385571052,
4.14983704796462));
#45281=CARTESIAN_POINT('Ctrl Pts',(-87.0942909181878,-1.25258466539632,
3.73506282814365));
#45282=CARTESIAN_POINT('Ctrl Pts',(-87.0279997409553,-2.48939349223549,
3.32028860832269));
#45283=CARTESIAN_POINT('Ctrl Pts',(-86.9617085637227,-3.49970506891242,
2.23012574362311));
#45284=CARTESIAN_POINT('Ctrl Pts',(-86.8954173864903,-3.81938121987922,
0.965396173288631));
#45285=CARTESIAN_POINT('Ctrl Pts',(-86.8789994316717,-3.89855357466691,
0.652167870363411));
#45286=CARTESIAN_POINT('Ctrl Pts',(-86.8625814768532,-3.93536402261767,
0.328232067872365));
#45287=CARTESIAN_POINT('Ctrl Pts',(-86.8461635220346,-3.93240142136994,
0.00363335402696072));
#45288=CARTESIAN_POINT('Origin',(-54.75,0.,0.));
#45289=CARTESIAN_POINT('',(-85.412836477965,-3.92650867564805,-0.000365894358481667));
#45290=CARTESIAN_POINT('',(-85.5961635220347,-3.92659593005969,-0.000715850624292737));
#45291=CARTESIAN_POINT('',(-54.75,-3.933,-4.81653586104654E-16));
#45292=CARTESIAN_POINT('Ctrl Pts',(-85.412836477965,-3.92650867564805,-0.000365894358481667));
#45293=CARTESIAN_POINT('Ctrl Pts',(-85.4470971952784,-3.92594651516599,
0.679565426024714));
#45294=CARTESIAN_POINT('Ctrl Pts',(-85.4813579125918,-3.7583595467037,1.35975629231021));
#45295=CARTESIAN_POINT('Ctrl Pts',(-85.5156186299051,-3.42533275744544,
1.94595944843094));
#45296=CARTESIAN_POINT('Ctrl Pts',(-85.5819098071376,-2.78095810212358,
3.08020590804822));
#45297=CARTESIAN_POINT('Ctrl Pts',(-85.64820098437,-1.51720140270921,3.86257638181553));
#45298=CARTESIAN_POINT('Ctrl Pts',(-85.7144921616025,-0.214633784331787,
3.93364907087425));
#45299=CARTESIAN_POINT('Ctrl Pts',(-85.780783338835,1.0879338340456,4.00472175993298));
#45300=CARTESIAN_POINT('Ctrl Pts',(-85.8470745160675,2.42931237138605,3.36449666428316));
#45301=CARTESIAN_POINT('Ctrl Pts',(-85.9133656933,3.19327115052751,2.30709385014463));
#45302=CARTESIAN_POINT('Ctrl Pts',(-85.9796568705325,3.95722992966898,1.24969103600607));
#45303=CARTESIAN_POINT('Ctrl Pts',(-86.045948047765,4.14376895061143,-0.224889496621225));
#45304=CARTESIAN_POINT('Ctrl Pts',(-86.1122392249975,3.66719199562616,-1.4392239371904));
#45305=CARTESIAN_POINT('Ctrl Pts',(-86.17853040223,3.1906150406409,-2.65355837775957));
#45306=CARTESIAN_POINT('Ctrl Pts',(-86.2448215794625,2.05092210972791,-3.60764672627063));
#45307=CARTESIAN_POINT('Ctrl Pts',(-86.311112756695,0.771689305398751,-3.86317981591585));
#45308=CARTESIAN_POINT('Ctrl Pts',(-86.3774039339274,-0.507543498930407,
-4.11871290556108));
#45309=CARTESIAN_POINT('Ctrl Pts',(-86.4436951111599,-1.92631617667573,
-3.67569073634049));
#45310=CARTESIAN_POINT('Ctrl Pts',(-86.5099862883923,-2.83284310311752,
-2.73763814761665));
#45311=CARTESIAN_POINT('Ctrl Pts',(-86.5609363515832,-3.52958143413936,
-2.01666982774167));
#45312=CARTESIAN_POINT('Ctrl Pts',(-86.6118864147741,-3.92372852181079,
-1.00327961905144));
#45313=CARTESIAN_POINT('Ctrl Pts',(-86.662836477965,-3.93304779575148,0.00362946431549549));
#45314=CARTESIAN_POINT('Ctrl Pts',(-86.8461635220346,-3.93240142136994,
0.00363335402696072));
#45315=CARTESIAN_POINT('Ctrl Pts',(-86.7962902996207,-3.92340185518861,
-0.982408088393583));
#45316=CARTESIAN_POINT('Ctrl Pts',(-86.7464170772068,-3.54738575066246,
-1.97456672412491));
#45317=CARTESIAN_POINT('Ctrl Pts',(-86.6965438547929,-2.87692246730654,
-2.69127846780546));
#45318=CARTESIAN_POINT('Ctrl Pts',(-86.6302526775604,-1.98574683851036,
-3.64392726259569));
#45319=CARTESIAN_POINT('Ctrl Pts',(-86.5639615003279,-0.57435485566134,
-4.10992857620667));
#45320=CARTESIAN_POINT('Ctrl Pts',(-86.4976703230954,0.70885855533344,-3.87520092675168));
#45321=CARTESIAN_POINT('Ctrl Pts',(-86.4313791458629,1.9920719663282,-3.64047327729668));
#45322=CARTESIAN_POINT('Ctrl Pts',(-86.3650879686304,3.14710680546873,-2.70501666477572));
#45323=CARTESIAN_POINT('Ctrl Pts',(-86.298796791398,3.64333888185318,-1.49858081735462));
#45324=CARTESIAN_POINT('Ctrl Pts',(-86.2325056141655,4.13957095823763,-0.29214496993353));
#45325=CARTESIAN_POINT('Ctrl Pts',(-86.166214436933,3.97700027186602,1.18527011238769));
#45326=CARTESIAN_POINT('Ctrl Pts',(-86.0999232597005,3.23031196295841,2.25493842402275));
#45327=CARTESIAN_POINT('Ctrl Pts',(-86.033632082468,2.48362365405083,3.32460673565777));
#45328=CARTESIAN_POINT('Ctrl Pts',(-85.9673409052355,1.1528177226073,3.98652827660665));
#45329=CARTESIAN_POINT('Ctrl Pts',(-85.901049728003,-0.150732220213392,
3.9366156114048));
#45330=CARTESIAN_POINT('Ctrl Pts',(-85.8347585507705,-1.45428216303412,
3.88670294620295));
#45331=CARTESIAN_POINT('Ctrl Pts',(-85.768467373538,-2.73057611723201,3.12495607485035));
#45332=CARTESIAN_POINT('Ctrl Pts',(-85.7021761963055,-3.39328332995887,
2.00132229208334));
#45333=CARTESIAN_POINT('Ctrl Pts',(-85.6668386382152,-3.74654986714039,
1.40235157337791));
#45334=CARTESIAN_POINT('Ctrl Pts',(-85.6315010801249,-3.92546013234001,
0.700547386331901));
#45335=CARTESIAN_POINT('Ctrl Pts',(-85.5961635220347,-3.92659593005969,
-0.000715850624292737));
#45336=CARTESIAN_POINT('Origin',(-54.75,0.,0.));
#45337=CARTESIAN_POINT('',(-84.162836477965,-3.93439518658889,-0.00350198815590452));
#45338=CARTESIAN_POINT('',(-84.3461635220346,-3.93503686469963,-0.00338281421578225));
#45339=CARTESIAN_POINT('',(-54.75,-3.933,-4.81653586104654E-16));
#45340=CARTESIAN_POINT('Ctrl Pts',(-84.162836477965,-3.93439518658889,-0.00350198815590452));
#45341=CARTESIAN_POINT('Ctrl Pts',(-84.2160167985501,-3.92468364801176,
1.04656012953353));
#45342=CARTESIAN_POINT('Ctrl Pts',(-84.2691971191353,-3.49131722508058,
2.10369626757898));
#45343=CARTESIAN_POINT('Ctrl Pts',(-84.3223774397204,-2.73918768000938,
2.83134482673009));
#45344=CARTESIAN_POINT('Ctrl Pts',(-84.3886686169529,-1.80163122255463,
3.73838485708176));
#45345=CARTESIAN_POINT('Ctrl Pts',(-84.4549597941853,-0.368764153098906,
4.13345006031658));
#45346=CARTESIAN_POINT('Ctrl Pts',(-84.5212509714178,0.901152925616475,
3.8350470764802));
#45347=CARTESIAN_POINT('Ctrl Pts',(-84.5875421486503,2.17107000433186,3.53664409264381));
#45348=CARTESIAN_POINT('Ctrl Pts',(-84.6538333258829,3.27803709230692,2.54477292173622));
#45349=CARTESIAN_POINT('Ctrl Pts',(-84.7201245031154,3.71351237287333,1.31510019796331));
#45350=CARTESIAN_POINT('Ctrl Pts',(-84.7864156803478,4.14898765343973,0.0854274741904251));
#45351=CARTESIAN_POINT('Ctrl Pts',(-84.8527068575802,3.91297112659752,-1.38204680244773));
#45352=CARTESIAN_POINT('Ctrl Pts',(-84.9189980348127,3.11388902708113,-2.41316344270134));
#45353=CARTESIAN_POINT('Ctrl Pts',(-84.9852892120452,2.31480692756472,-3.44428008295497));
#45354=CARTESIAN_POINT('Ctrl Pts',(-85.0515803892777,0.9526592553741,-4.03903908682399));
#45355=CARTESIAN_POINT('Ctrl Pts',(-85.1178715665102,-0.346781950456118,
-3.9242075573298));
#45356=CARTESIAN_POINT('Ctrl Pts',(-85.1841627437427,-1.64622315628634,
-3.80937602783561));
#45357=CARTESIAN_POINT('Ctrl Pts',(-85.2504539209751,-2.88295789575617,
-2.98495396497819));
#45358=CARTESIAN_POINT('Ctrl Pts',(-85.3167450982076,-3.48882895987641,
-1.82968171081588));
#45359=CARTESIAN_POINT('Ctrl Pts',(-85.3487755581267,-3.78157272527062,
-1.27147919914778));
#45360=CARTESIAN_POINT('Ctrl Pts',(-85.3808060180458,-3.92703424137465,
-0.636035974061732));
#45361=CARTESIAN_POINT('Ctrl Pts',(-85.412836477965,-3.92650867564805,-0.000365894358481667));
#45362=CARTESIAN_POINT('Ctrl Pts',(-85.5961635220347,-3.92659593005969,
-0.000715850624292737));
#45363=CARTESIAN_POINT('Ctrl Pts',(-85.5652099028925,-3.92759082195199,
-0.614981134594069));
#45364=CARTESIAN_POINT('Ctrl Pts',(-85.5342562837504,-3.79218420171298,
-1.22883136227772));
#45365=CARTESIAN_POINT('Ctrl Pts',(-85.5033026646082,-3.51807874880253,
-1.77279005846446));
#45366=CARTESIAN_POINT('Ctrl Pts',(-85.4370114873757,-2.93104648366353,
-2.93774793206387));
#45367=CARTESIAN_POINT('Ctrl Pts',(-85.3707203101432,-1.7078614821297,-3.78214298508129));
#45368=CARTESIAN_POINT('Ctrl Pts',(-85.3044291329107,-0.410456189671825,
-3.91805926327392));
#45369=CARTESIAN_POINT('Ctrl Pts',(-85.2381379556782,0.886949102786071,
-4.05397554146654));
#45370=CARTESIAN_POINT('Ctrl Pts',(-85.1718467784457,2.25857468616802,-3.48141304483438));
#45371=CARTESIAN_POINT('Ctrl Pts',(-85.1055556012133,3.07429435930779,-2.46340757214366));
#45372=CARTESIAN_POINT('Ctrl Pts',(-85.0392644239808,3.89001403244753,-1.44540209945299));
#45373=CARTESIAN_POINT('Ctrl Pts',(-84.9729732467483,4.14982779534511,0.0180463492962202));
#45374=CARTESIAN_POINT('Ctrl Pts',(-84.9066820695158,3.73437693859115,1.25462805431929));
#45375=CARTESIAN_POINT('Ctrl Pts',(-84.8403908922833,3.31892608183717,2.49120975934241));
#45376=CARTESIAN_POINT('Ctrl Pts',(-84.7740997150508,2.22821060543163,3.50092472063938));
#45377=CARTESIAN_POINT('Ctrl Pts',(-84.7078085378183,0.963306319003282,
3.81990884838039));
#45378=CARTESIAN_POINT('Ctrl Pts',(-84.6415173605858,-0.301597967425049,
4.13889297612139));
#45379=CARTESIAN_POINT('Ctrl Pts',(-84.5752261833534,-1.74069106387619,
3.76714627030641));
#45380=CARTESIAN_POINT('Ctrl Pts',(-84.5089350061209,-2.69285212441525,
2.87544954923551));
#45381=CARTESIAN_POINT('Ctrl Pts',(-84.4546778447588,-3.47216482425126,
2.14562493454348));
#45382=CARTESIAN_POINT('Ctrl Pts',(-84.4004206833967,-3.92528723901599,
1.06749166239896));
#45383=CARTESIAN_POINT('Ctrl Pts',(-84.3461635220346,-3.93503686469963,
-0.00338281421578225));
#45384=CARTESIAN_POINT('Origin',(-54.75,0.,0.));
#45385=CARTESIAN_POINT('',(-82.912836477965,-3.93823441574634,0.00201426645151499));
#45386=CARTESIAN_POINT('',(-83.0961635220346,-3.93777751392323,0.00232566860396301));
#45387=CARTESIAN_POINT('',(-54.75,-3.933,-4.81653586104654E-16));
#45388=CARTESIAN_POINT('Ctrl Pts',(-82.912836477965,-3.93823441574634,0.00201426645151499));
#45389=CARTESIAN_POINT('Ctrl Pts',(-82.9186452245895,-3.93894770498266,
0.11641899894547));
#45390=CARTESIAN_POINT('Ctrl Pts',(-82.9244539712139,-3.93439648798973,
0.230766159426596));
#45391=CARTESIAN_POINT('Ctrl Pts',(-82.9302627178383,-3.92439670583951,
0.34463483480704));
#45392=CARTESIAN_POINT('Ctrl Pts',(-82.9965538950707,-3.81027616079436,
1.64413867426808));
#45393=CARTESIAN_POINT('Ctrl Pts',(-83.0628450723031,-2.98653087981396,
2.88132429720423));
#45394=CARTESIAN_POINT('Ctrl Pts',(-83.1291362495356,-1.83159029066747,
3.48782735829902));
#45395=CARTESIAN_POINT('Ctrl Pts',(-83.195427426768,-0.676649701520935,
4.09433041939382));
#45396=CARTESIAN_POINT('Ctrl Pts',(-83.2617186040007,0.809486195791681,
4.0701509186472));
#45397=CARTESIAN_POINT('Ctrl Pts',(-83.3280097812332,1.94408504432396,3.42639694352571));
#45398=CARTESIAN_POINT('Ctrl Pts',(-83.3943009584657,3.07868389285625,2.78264296840423));
#45399=CARTESIAN_POINT('Ctrl Pts',(-83.4605921356981,3.86174569260815,1.51931451890789));
#45400=CARTESIAN_POINT('Ctrl Pts',(-83.5268833129305,3.93353104885403,0.216785981714108));
#45401=CARTESIAN_POINT('Ctrl Pts',(-83.593174490163,4.00531640509991,-1.08574255547963));
#45402=CARTESIAN_POINT('Ctrl Pts',(-83.6594656673956,3.36582531783971,-2.42747118037085));
#45403=CARTESIAN_POINT('Ctrl Pts',(-83.7257568446281,2.30884064908559,-3.19200838521713));
#45404=CARTESIAN_POINT('Ctrl Pts',(-83.7920480218606,1.25185598033144,-3.95654559006343));
#45405=CARTESIAN_POINT('Ctrl Pts',(-83.858339199093,-0.222622269916648,
-4.14389137486483));
#45406=CARTESIAN_POINT('Ctrl Pts',(-83.9246303763255,-1.43721727974187,
-3.66797889374759));
#45407=CARTESIAN_POINT('Ctrl Pts',(-83.990921553558,-2.6518122895671,-3.19206641263036));
#45408=CARTESIAN_POINT('Ctrl Pts',(-84.0572127307905,-3.60652405896942,
-2.0528956655945));
#45409=CARTESIAN_POINT('Ctrl Pts',(-84.1235039080229,-3.86275702094368,
-0.773802863342302));
#45410=CARTESIAN_POINT('Ctrl Pts',(-84.1366147646703,-3.91343395523601,
-0.520827986909221));
#45411=CARTESIAN_POINT('Ctrl Pts',(-84.1497256213176,-3.93678942920926,
-0.26237996678345));
#45412=CARTESIAN_POINT('Ctrl Pts',(-84.162836477965,-3.93439518658889,-0.00350198815590452));
#45413=CARTESIAN_POINT('Ctrl Pts',(-84.3461635220346,-3.93503686469963,
-0.00338281421578225));
#45414=CARTESIAN_POINT('Ctrl Pts',(-84.3341295061642,-3.93719929169106,
-0.240898381253968));
#45415=CARTESIAN_POINT('Ctrl Pts',(-84.3220954902938,-3.91755069453226,
-0.478056863309719));
#45416=CARTESIAN_POINT('Ctrl Pts',(-84.3100614744233,-3.87481250676164,
-0.710978699828652));
#45417=CARTESIAN_POINT('Ctrl Pts',(-84.2437702971909,-3.63938280394195,
-1.99406349149509));
#45418=CARTESIAN_POINT('Ctrl Pts',(-84.1774791199585,-2.70329437367554,
-3.14858633850115));
#45419=CARTESIAN_POINT('Ctrl Pts',(-84.111187942726,-1.49658720184918,-3.64415825965719));
#45420=CARTESIAN_POINT('Ctrl Pts',(-84.0448967654935,-0.289880030022867,
-4.1397301808132));
#45421=CARTESIAN_POINT('Ctrl Pts',(-83.978605588261,1.18744588336335,-3.97635117611928));
#45422=CARTESIAN_POINT('Ctrl Pts',(-83.9123144110285,2.25670549702358,-3.22907772806261));
#45423=CARTESIAN_POINT('Ctrl Pts',(-83.846023233796,3.32596511068386,-2.48180428000591));
#45424=CARTESIAN_POINT('Ctrl Pts',(-83.7797320565636,3.98715842461806,-1.15063638858639));
#45425=CARTESIAN_POINT('Ctrl Pts',(-83.7134408793311,3.93653255159977,0.152886050252543));
#45426=CARTESIAN_POINT('Ctrl Pts',(-83.6471497020986,3.88590667858149,1.45640848909151));
#45427=CARTESIAN_POINT('Ctrl Pts',(-83.580858524866,3.12346161861065,2.73228547534992));
#45428=CARTESIAN_POINT('Ctrl Pts',(-83.5145673476336,1.99946541499167,3.39437781167899));
#45429=CARTESIAN_POINT('Ctrl Pts',(-83.4482761704011,0.875469211372724,
4.05647014800804));
#45430=CARTESIAN_POINT('Ctrl Pts',(-83.3819849931687,-0.610078135894369,
4.1047778344078));
#45431=CARTESIAN_POINT('Ctrl Pts',(-83.3156938159362,-1.77471465035827,
3.5171082701518));
#45432=CARTESIAN_POINT('Ctrl Pts',(-83.2494026387037,-2.93935116482217,
2.9294387058958));
#45433=CARTESIAN_POINT('Ctrl Pts',(-83.1831114614712,-3.7830768464829,1.70579189098402));
#45434=CARTESIAN_POINT('Ctrl Pts',(-83.1168202842387,-3.91828325098612,
0.408312428427184));
#45435=CARTESIAN_POINT('Ctrl Pts',(-83.1099346968373,-3.93232698281131,
0.273544747208272));
#45436=CARTESIAN_POINT('Ctrl Pts',(-83.1030491094359,-3.93872668788066,
0.137980505116214));
#45437=CARTESIAN_POINT('Ctrl Pts',(-83.0961635220346,-3.93777751392323,
0.00232566860396301));
#45438=CARTESIAN_POINT('Origin',(-54.75,0.,0.));
#45439=CARTESIAN_POINT('',(-81.662836477965,-3.92815744923983,0.00251336901012894));
#45440=CARTESIAN_POINT('',(-81.8461635220347,-3.92776649390124,0.00224383255729018));
#45441=CARTESIAN_POINT('',(-54.75,-3.933,-4.81653586104654E-16));
#45442=CARTESIAN_POINT('Ctrl Pts',(-81.662836477965,-3.92815744923983,0.00251336901012894));
#45443=CARTESIAN_POINT('Ctrl Pts',(-81.6875648278611,-3.93101333610238,
0.492752512294545));
#45444=CARTESIAN_POINT('Ctrl Pts',(-81.7122931777573,-3.84604462728733,
0.982037294908663));
#45445=CARTESIAN_POINT('Ctrl Pts',(-81.7370215276534,-3.66876469384258,
1.43521019205571));
#45446=CARTESIAN_POINT('Ctrl Pts',(-81.8033127048859,-3.19351682905999,
2.65006540754234));
#45447=CARTESIAN_POINT('Ctrl Pts',(-81.8696038821185,-2.05486860691728,
3.60540031203857));
#45448=CARTESIAN_POINT('Ctrl Pts',(-81.935895059351,-0.775916189644389,
3.86233306963734));
#45449=CARTESIAN_POINT('Ctrl Pts',(-82.0021862365835,0.503036227628501,
4.11926582723611));
#45450=CARTESIAN_POINT('Ctrl Pts',(-82.0684774138159,1.92229284003157,3.67779643793744));
#45451=CARTESIAN_POINT('Ctrl Pts',(-82.1347685910484,2.8298457027665,2.74073639241362));
#45452=CARTESIAN_POINT('Ctrl Pts',(-82.2010597682809,3.73739856550144,1.8036763468898));
#45453=CARTESIAN_POINT('Ctrl Pts',(-82.2673509455133,4.13324767856824,0.371025645140833));
#45454=CARTESIAN_POINT('Ctrl Pts',(-82.3336421227458,3.83553955303096,-0.899054509638602));
#45455=CARTESIAN_POINT('Ctrl Pts',(-82.3999332999783,3.53783142749368,-2.16913466441804));
#45456=CARTESIAN_POINT('Ctrl Pts',(-82.4662244772108,2.54656606335231,-3.27664427222795));
#45457=CARTESIAN_POINT('Ctrl Pts',(-82.5325156544433,1.3171317865624,-3.71279228223091));
#45458=CARTESIAN_POINT('Ctrl Pts',(-82.5988068316758,0.0876975097725195,
-4.14894029223385));
#45459=CARTESIAN_POINT('Ctrl Pts',(-82.6650980089082,-1.37990567966589,
-3.91372670442989));
#45460=CARTESIAN_POINT('Ctrl Pts',(-82.7313891861407,-2.41145936983018,
-3.11520888253495));
#45461=CARTESIAN_POINT('Ctrl Pts',(-82.7918716167488,-3.35262344457671,
-2.38666097060545));
#45462=CARTESIAN_POINT('Ctrl Pts',(-82.852354047357,-3.93080743200468,-1.18920248678531));
#45463=CARTESIAN_POINT('Ctrl Pts',(-82.912836477965,-3.93823441574634,0.00201426645151499));
#45464=CARTESIAN_POINT('Ctrl Pts',(-83.0961635220346,-3.93777751392323,
0.00232566860396301));
#45465=CARTESIAN_POINT('Ctrl Pts',(-83.0367579322034,-3.92958849016864,
-1.16804006880197));
#45466=CARTESIAN_POINT('Ctrl Pts',(-82.9773523423723,-3.37439139798938,
-2.34514913109041));
#45467=CARTESIAN_POINT('Ctrl Pts',(-82.9179467525412,-2.46172515530447,
-3.07564171091296));
#45468=CARTESIAN_POINT('Ctrl Pts',(-82.8516555753088,-1.44327352777386,
-3.89080427749445));
#45469=CARTESIAN_POINT('Ctrl Pts',(-82.7853643980763,0.0203168546331192,
-4.14981730045549));
#45470=CARTESIAN_POINT('Ctrl Pts',(-82.7190732208438,1.25667106766366,-3.73368993113562));
#45471=CARTESIAN_POINT('Ctrl Pts',(-82.6527820436113,2.49302528069421,-3.31756256181575));
#45472=CARTESIAN_POINT('Ctrl Pts',(-82.5864908663788,3.50214332434836,-2.22629480021494));
#45473=CARTESIAN_POINT('Ctrl Pts',(-82.5201996891463,3.82043533337418,-0.961216176347729));
#45474=CARTESIAN_POINT('Ctrl Pts',(-82.4539085119138,4.13872734240001,0.303862447519519));
#45475=CARTESIAN_POINT('Ctrl Pts',(-82.3876173346814,3.76619331679752,1.74275193365313));
#45476=CARTESIAN_POINT('Ctrl Pts',(-82.321326157449,2.87397577038541,2.69442497490727));
#45477=CARTESIAN_POINT('Ctrl Pts',(-82.2550349802165,1.98175822397333,3.64609801616138));
#45478=CARTESIAN_POINT('Ctrl Pts',(-82.1887438029839,0.569857156751641,
4.11055461253598));
#45479=CARTESIAN_POINT('Ctrl Pts',(-82.1224526257514,-0.713098631489105,
3.87442292682856));
#45480=CARTESIAN_POINT('Ctrl Pts',(-82.0561614485189,-1.99605441972978,
3.63829124112116));
#45481=CARTESIAN_POINT('Ctrl Pts',(-81.9898702712864,-3.15006492898956,
2.70157127333181));
#45482=CARTESIAN_POINT('Ctrl Pts',(-81.923579094054,-3.64497654656548,1.49459313833364));
#45483=CARTESIAN_POINT('Ctrl Pts',(-81.8977739033809,-3.83763097195148,
1.02475232071357));
#45484=CARTESIAN_POINT('Ctrl Pts',(-81.8719687127078,-3.93041120894692,
0.513958900310409));
#45485=CARTESIAN_POINT('Ctrl Pts',(-81.8461635220347,-3.92776649390124,
0.00224383255729018));
#45486=CARTESIAN_POINT('Origin',(-54.75,0.,0.));
#45487=CARTESIAN_POINT('',(-80.412836477965,-3.92903919912688,-0.0029659054929293));
#45488=CARTESIAN_POINT('',(-80.5961635220346,-3.92955240483563,-0.0031591487905448));
#45489=CARTESIAN_POINT('',(-54.75,-3.933,-4.81653586104654E-16));
#45490=CARTESIAN_POINT('Ctrl Pts',(-80.412836477965,-3.92903919912688,-0.0029659054929293));
#45491=CARTESIAN_POINT('Ctrl Pts',(-80.4564844311329,-3.92300599112755,
0.861866566955545));
#45492=CARTESIAN_POINT('Ctrl Pts',(-80.5001323843009,-3.64192243487377,
1.73026339850602));
#45493=CARTESIAN_POINT('Ctrl Pts',(-80.5437803374688,-3.11652780543653,
2.40975457507759));
#45494=CARTESIAN_POINT('Ctrl Pts',(-80.6100715147012,-2.31857450020302,
3.44174500635217));
#45495=CARTESIAN_POINT('Ctrl Pts',(-80.6763626919337,-0.957078468089482,
4.0379942059965));
#45496=CARTESIAN_POINT('Ctrl Pts',(-80.7426538691662,0.342487615989928,
3.92458467956292));
#45497=CARTESIAN_POINT('Ctrl Pts',(-80.8089450463987,1.64205370006938,3.81117515312933));
#45498=CARTESIAN_POINT('Ctrl Pts',(-80.8752362236312,2.87968983611469,2.98810690061779));
#45499=CARTESIAN_POINT('Ctrl Pts',(-80.9415274008637,3.48682471262449,1.83349832222383));
#45500=CARTESIAN_POINT('Ctrl Pts',(-81.0078185780962,4.0939595891343,0.678889743829845));
#45501=CARTESIAN_POINT('Ctrl Pts',(-81.0741097553286,4.07059320610855,-0.807259160446579));
#45502=CARTESIAN_POINT('Ctrl Pts',(-81.1404009325611,3.42746010389805,-1.94221005824642));
#45503=CARTESIAN_POINT('Ctrl Pts',(-81.2066921097936,2.78432700168757,-3.07716095604624));
#45504=CARTESIAN_POINT('Ctrl Pts',(-81.2729832870261,1.52142718029238,-3.8609138473695));
#45505=CARTESIAN_POINT('Ctrl Pts',(-81.3392744642586,0.218938114200209,
-3.93341184931313));
#45506=CARTESIAN_POINT('Ctrl Pts',(-81.4055656414911,-1.08355095189193,
-4.00590985125675));
#45507=CARTESIAN_POINT('Ctrl Pts',(-81.4718568187236,-2.42562926268104,
-3.36715296382081));
#45508=CARTESIAN_POINT('Ctrl Pts',(-81.5381479959561,-3.19074466436435,
-2.31058675686434));
#45509=CARTESIAN_POINT('Ctrl Pts',(-81.5797108232923,-3.67045192949554,
-1.64814749024648));
#45510=CARTESIAN_POINT('Ctrl Pts',(-81.6212736506287,-3.9233573419517,-0.821469021703119));
#45511=CARTESIAN_POINT('Ctrl Pts',(-81.662836477965,-3.92815744923983,0.00251336901012894));
#45512=CARTESIAN_POINT('Ctrl Pts',(-81.8461635220347,-3.92776649390124,
0.00224383255729018));
#45513=CARTESIAN_POINT('Ctrl Pts',(-81.8056775354753,-3.9236171776203,-0.800590357575939));
#45514=CARTESIAN_POINT('Ctrl Pts',(-81.7651915489159,-3.68458179285588,
-1.60569315898882));
#45515=CARTESIAN_POINT('Ctrl Pts',(-81.7247055623565,-3.22784252652727,
-2.25847189446946));
#45516=CARTESIAN_POINT('Ctrl Pts',(-81.658414385124,-2.47998416302114,-3.32732249006709));
#45517=CARTESIAN_POINT('Ctrl Pts',(-81.5921232078915,-1.14845471011691,
-3.98778737905524));
#45518=CARTESIAN_POINT('Ctrl Pts',(-81.525832030659,0.155039834524771,-3.93644831337552));
#45519=CARTESIAN_POINT('Ctrl Pts',(-81.4595408534265,1.45853437916645,-3.88510924769581));
#45520=CARTESIAN_POINT('Ctrl Pts',(-81.393249676194,2.73399401554557,-3.12196622734823));
#45521=CARTESIAN_POINT('Ctrl Pts',(-81.3269584989616,3.39547127727642,-1.99760793935079));
#45522=CARTESIAN_POINT('Ctrl Pts',(-81.2606673217291,4.05694853900726,-0.873249651353348));
#45523=CARTESIAN_POINT('Ctrl Pts',(-81.1943761444967,4.10444342608984,0.612323904293962));
#45524=CARTESIAN_POINT('Ctrl Pts',(-81.1280849672642,3.51613673863844,1.77663871098304));
#45525=CARTESIAN_POINT('Ctrl Pts',(-81.0617937900317,2.92783005118702,2.94095351767216));
#45526=CARTESIAN_POINT('Ctrl Pts',(-80.9955026127992,1.70372178920158,3.78400957540303));
#45527=CARTESIAN_POINT('Ctrl Pts',(-80.9292114355667,0.406168544952221,
3.91850606574213));
#45528=CARTESIAN_POINT('Ctrl Pts',(-80.8629202583342,-0.89138469929703,
4.05300255608121));
#45529=CARTESIAN_POINT('Ctrl Pts',(-80.7966290811017,-2.26238292581019,
3.47893947902867));
#45530=CARTESIAN_POINT('Ctrl Pts',(-80.7303379038692,-3.07698814181064,
2.46004200153638));
#45531=CARTESIAN_POINT('Ctrl Pts',(-80.6856131099244,-3.62657938385882,
1.77262051297274));
#45532=CARTESIAN_POINT('Ctrl Pts',(-80.6408883159795,-3.92291045278412,
0.882718340543989));
#45533=CARTESIAN_POINT('Ctrl Pts',(-80.5961635220346,-3.92955240483563,
-0.0031591487905448));
#45534=CARTESIAN_POINT('Origin',(-54.75,0.,0.));
#45535=CARTESIAN_POINT('',(-79.1628364779651,-3.9389481592111,-0.0013426765242408));
#45536=CARTESIAN_POINT('',(-79.3461635220346,-3.93921293753935,-0.000967729229624012));
#45537=CARTESIAN_POINT('',(-54.75,-3.933,-4.81653586104654E-16));
#45538=CARTESIAN_POINT('Ctrl Pts',(-79.1628364779651,-3.9389481592111,-0.0013426765242408));
#45539=CARTESIAN_POINT('Ctrl Pts',(-79.2254040344047,-3.93350653257731,
1.23034949682626));
#45540=CARTESIAN_POINT('Ctrl Pts',(-79.2879715908444,-3.30915507795444,
2.46679613944863));
#45541=CARTESIAN_POINT('Ctrl Pts',(-79.350539147284,-2.31233217295835,3.18947998834734));
#45542=CARTESIAN_POINT('Ctrl Pts',(-79.4168303245165,-1.25618474408748,
3.95517335782692));
#45543=CARTESIAN_POINT('Ctrl Pts',(-79.483121501749,0.218087617257299,4.14413250185621));
#45544=CARTESIAN_POINT('Ctrl Pts',(-79.5494126789815,1.43320267473284,3.66954939567586));
#45545=CARTESIAN_POINT('Ctrl Pts',(-79.615703856214,2.64831773220827,3.19496628949555));
#45546=CARTESIAN_POINT('Ctrl Pts',(-79.6819950334464,3.60427548581447,2.05684093310556));
#45547=CARTESIAN_POINT('Ctrl Pts',(-79.7482862106789,3.86190796212373,0.778029283672377));
#45548=CARTESIAN_POINT('Ctrl Pts',(-79.8145773879114,4.11954043843302,-0.500782365760914));
#45549=CARTESIAN_POINT('Ctrl Pts',(-79.8808685651439,3.67884763744538,-1.92028030823745));
#45550=CARTESIAN_POINT('Ctrl Pts',(-79.9471597423764,2.74228428436574,-2.82834573167552));
#45551=CARTESIAN_POINT('Ctrl Pts',(-80.0134509196089,1.80572093128612,-3.73641115511357));
#45552=CARTESIAN_POINT('Ctrl Pts',(-80.0797420968414,0.373287026114508,
-4.1330440595131));
#45553=CARTESIAN_POINT('Ctrl Pts',(-80.1460332740738,-0.896955824524606,
-3.83603088139523));
#45554=CARTESIAN_POINT('Ctrl Pts',(-80.2123244513063,-2.16719867516372,
-3.53901770327735));
#45555=CARTESIAN_POINT('Ctrl Pts',(-80.2786156285388,-3.27525047127037,
-2.54835844264207));
#45556=CARTESIAN_POINT('Ctrl Pts',(-80.3449068057713,-3.71207108014695,
-1.319162980872));
#45557=CARTESIAN_POINT('Ctrl Pts',(-80.3675500298359,-3.86127686190769,
-0.899303967622076));
#45558=CARTESIAN_POINT('Ctrl Pts',(-80.3901932539004,-3.93216904304033,
-0.45161455979811));
#45559=CARTESIAN_POINT('Ctrl Pts',(-80.412836477965,-3.92903919912688,-0.0029659054929293));
#45560=CARTESIAN_POINT('Ctrl Pts',(-80.5961635220346,-3.92955240483563,
-0.0031591487905448));
#45561=CARTESIAN_POINT('Ctrl Pts',(-80.574597138747,-3.93275516713114,-0.430331010206185));
#45562=CARTESIAN_POINT('Ctrl Pts',(-80.5530307554594,-3.86859978389275,
-0.856567057420322));
#45563=CARTESIAN_POINT('Ctrl Pts',(-80.5314643721718,-3.73300180598275,
-1.25871370481774));
#45564=CARTESIAN_POINT('Ctrl Pts',(-80.4651731949393,-3.31619804866662,
-2.4948400557474));
#45565=CARTESIAN_POINT('Ctrl Pts',(-80.3988820177068,-2.22437832854666,
-3.50336087967453));
#45566=CARTESIAN_POINT('Ctrl Pts',(-80.3325908404744,-0.959125745947673,
-3.82096067470299));
#45567=CARTESIAN_POINT('Ctrl Pts',(-80.2662996632419,0.306126836651311,
-4.13856046973145));
#45568=CARTESIAN_POINT('Ctrl Pts',(-80.2000084860094,1.74481228172936,-3.76523923586116));
#45569=CARTESIAN_POINT('Ctrl Pts',(-80.1337173087769,2.69599701881079,-2.8725011311973));
#45570=CARTESIAN_POINT('Ctrl Pts',(-80.0674261315444,3.6471817558922,-1.97976302653346));
#45571=CARTESIAN_POINT('Ctrl Pts',(-80.0011349543119,4.1108657849771,-0.567608051076111));
#45572=CARTESIAN_POINT('Ctrl Pts',(-79.9348437770794,3.87403218706907,0.715218349680184));
#45573=CARTESIAN_POINT('Ctrl Pts',(-79.868552599847,3.63719858916104,1.99804475043648));
#45574=CARTESIAN_POINT('Ctrl Pts',(-79.8022614226145,2.69984736426009,3.15154257649167));
#45575=CARTESIAN_POINT('Ctrl Pts',(-79.735970245382,1.49259862740443,3.64579374233333));
#45576=CARTESIAN_POINT('Ctrl Pts',(-79.6696790681495,0.285349890548748,
4.140044908175));
#45577=CARTESIAN_POINT('Ctrl Pts',(-79.603387890917,-1.19179635826171,3.97504941380306));
#45578=CARTESIAN_POINT('Ctrl Pts',(-79.5370967136845,-2.26023761583134,
3.22660635872235));
#45579=CARTESIAN_POINT('Ctrl Pts',(-79.4734523164678,-3.28601966765575,
2.50804607543565));
#45580=CARTESIAN_POINT('Ctrl Pts',(-79.4098079192513,-3.93508158397175,
1.25169827097145));
#45581=CARTESIAN_POINT('Ctrl Pts',(-79.3461635220346,-3.93921293753935,
-0.000967729229624012));
#45582=CARTESIAN_POINT('Origin',(-54.75,0.,0.));
#45583=CARTESIAN_POINT('',(-77.912836477965,-3.93313541941523,0.00362608069297291));
#45584=CARTESIAN_POINT('',(-78.0961635220346,-3.93248803517055,0.00363500034747385));
#45585=CARTESIAN_POINT('',(-54.75,-3.933,-4.81653586104654E-16));
#45586=CARTESIAN_POINT('Ctrl Pts',(-77.912836477965,-3.93313541941523,0.00362608069297291));
#45587=CARTESIAN_POINT('Ctrl Pts',(-77.9280324604439,-3.93591805124307,
0.303922101060753));
#45588=CARTESIAN_POINT('Ctrl Pts',(-77.9432284429229,-3.90444631903579,
0.603640822955118));
#45589=CARTESIAN_POINT('Ctrl Pts',(-77.9584244254018,-3.83652106142591,
0.894856870902738));
#45590=CARTESIAN_POINT('Ctrl Pts',(-78.0247156026343,-3.54020291963971,
2.16526203714848));
#45591=CARTESIAN_POINT('Ctrl Pts',(-78.0910067798669,-2.55015005906897,
3.27385568985141));
#45592=CARTESIAN_POINT('Ctrl Pts',(-78.1572979570994,-1.32119378028406,
3.71134876683736));
#45593=CARTESIAN_POINT('Ctrl Pts',(-78.2235891343319,-0.092237501499141,
4.1488418438233));
#45594=CARTESIAN_POINT('Ctrl Pts',(-78.2898803115643,1.37562219549991,3.91523434509225));
#45595=CARTESIAN_POINT('Ctrl Pts',(-78.3561714887968,2.40804905895374,3.11784579539117));
#45596=CARTESIAN_POINT('Ctrl Pts',(-78.4224626660292,3.44047592240755,2.32045724569012));
#45597=CARTESIAN_POINT('Ctrl Pts',(-78.4887538432617,4.03746995231615,0.959287645018993));
#45598=CARTESIAN_POINT('Ctrl Pts',(-78.5550450204942,3.92477147844376,-0.340340294647681));
#45599=CARTESIAN_POINT('Ctrl Pts',(-78.6213361977267,3.81207300457136,-1.63996823431439));
#45600=CARTESIAN_POINT('Ctrl Pts',(-78.6876273749592,2.98968202691799,-2.87805451297669));
#45601=CARTESIAN_POINT('Ctrl Pts',(-78.7539185521917,1.835405804914,-3.48582102315285));
#45602=CARTESIAN_POINT('Ctrl Pts',(-78.8202097294241,0.681129582910052,
-4.093587533329));
#45603=CARTESIAN_POINT('Ctrl Pts',(-78.8865009066566,-0.805031883444454,
-4.07103427501903));
#45604=CARTESIAN_POINT('Ctrl Pts',(-78.9527920838891,-1.94033449075904,
-3.42852223824453));
#45605=CARTESIAN_POINT('Ctrl Pts',(-79.0190832611216,-3.07563709807365,
-2.78601020147002));
#45606=CARTESIAN_POINT('Ctrl Pts',(-79.0853744383542,-3.86008084634829,
-1.52353938623096));
#45607=CARTESIAN_POINT('Ctrl Pts',(-79.1516656155866,-3.93329147228718,
-0.221090181146506));
#45608=CARTESIAN_POINT('Ctrl Pts',(-79.1553892363794,-3.93740376324929,
-0.147930717940411));
#45609=CARTESIAN_POINT('Ctrl Pts',(-79.1591128571723,-3.93927201002505,
-0.0746451170862052));
#45610=CARTESIAN_POINT('Ctrl Pts',(-79.1628364779651,-3.9389481592111,-0.0013426765242408));
#45611=CARTESIAN_POINT('Ctrl Pts',(-79.3461635220346,-3.93921293753935,
-0.000967729229624012));
#45612=CARTESIAN_POINT('Ctrl Pts',(-79.3435167420188,-3.9393847481706,-0.0530623594071839));
#45613=CARTESIAN_POINT('Ctrl Pts',(-79.3408699620029,-3.93844116481995,
-0.105150621980919));
#45614=CARTESIAN_POINT('Ctrl Pts',(-79.3382231819871,-3.93636289675727,
-0.157193572384996));
#45615=CARTESIAN_POINT('Ctrl Pts',(-79.2719320047546,-3.88431065378475,
-1.46065983262229));
#45616=CARTESIAN_POINT('Ctrl Pts',(-79.2056408275221,-3.12046990151082,
-2.73570173730745));
#45617=CARTESIAN_POINT('Ctrl Pts',(-79.1393496502896,-1.99574986571674,
-3.39656372642382));
#45618=CARTESIAN_POINT('Ctrl Pts',(-79.0730584730571,-0.871029829922625,
-4.05742571554021));
#45619=CARTESIAN_POINT('Ctrl Pts',(-79.0067672958246,0.614569489391649,
-4.10410778908778));
#45620=CARTESIAN_POINT('Ctrl Pts',(-78.9404761185922,1.7785622397629,-3.51516415455325));
#45621=CARTESIAN_POINT('Ctrl Pts',(-78.8741849413597,2.94255499013405,-2.92622052001877));
#45622=CARTESIAN_POINT('Ctrl Pts',(-78.8078937641272,3.78494117156225,-1.70165117740231));
#45623=CARTESIAN_POINT('Ctrl Pts',(-78.7416025868947,3.91872770747519,-0.404024539889156));
#45624=CARTESIAN_POINT('Ctrl Pts',(-78.6753114096622,4.05251424338815,0.893602097624076));
#45625=CARTESIAN_POINT('Ctrl Pts',(-78.6090202324297,3.47770113378575,2.26428603003402));
#45626=CARTESIAN_POINT('Ctrl Pts',(-78.5427290551972,2.45835811134335,3.07833365159769));
#45627=CARTESIAN_POINT('Ctrl Pts',(-78.4764378779647,1.43901508890095,3.89238127316137));
#45628=CARTESIAN_POINT('Ctrl Pts',(-78.4101467007323,-0.0248578463814547,
4.14979258387876));
#45629=CARTESIAN_POINT('Ctrl Pts',(-78.3438555234998,-1.26075596517005,
3.73231256333852));
#45630=CARTESIAN_POINT('Ctrl Pts',(-78.2775643462673,-2.49665408395865,
3.31483254279828));
#45631=CARTESIAN_POINT('Ctrl Pts',(-78.2112731690348,-3.50457738625344,
2.2224611910004));
#45632=CARTESIAN_POINT('Ctrl Pts',(-78.1449819918023,-3.82148487220956,
0.95703502842889));
#45633=CARTESIAN_POINT('Ctrl Pts',(-78.1287091685464,-3.8992777207111,0.646404607510269));
#45634=CARTESIAN_POINT('Ctrl Pts',(-78.1124363452905,-3.93543137278026,
0.325346258476264));
#45635=CARTESIAN_POINT('Ctrl Pts',(-78.0961635220346,-3.93248803517055,
0.00363500034747385));
#45636=CARTESIAN_POINT('Origin',(-54.75,0.,0.));
#45637=CARTESIAN_POINT('',(-76.662836477965,-3.92650124665457,-0.000318401066521645));
#45638=CARTESIAN_POINT('',(-76.8461635220347,-3.92658087967646,-0.000668997711400442));
#45639=CARTESIAN_POINT('',(-54.75,-3.933,-4.81653586104654E-16));
#45640=CARTESIAN_POINT('Ctrl Pts',(-76.662836477965,-3.92650124665457,-0.000318401066521645));
#45641=CARTESIAN_POINT('Ctrl Pts',(-76.6969520637157,-3.92601417802138,
0.676735860399884));
#45642=CARTESIAN_POINT('Ctrl Pts',(-76.7310676494664,-3.75992112010715,
1.35401404301683));
#45643=CARTESIAN_POINT('Ctrl Pts',(-76.7651832352171,-3.42958334624692,
1.93845834242374));
#45644=CARTESIAN_POINT('Ctrl Pts',(-76.8314744124496,-2.78769256724728,
3.074112319395));
#45645=CARTESIAN_POINT('Ctrl Pts',(-76.8977655896821,-1.52565113609083,
3.85924668979409));
#45646=CARTESIAN_POINT('Ctrl Pts',(-76.9640567669146,-0.223242181908324,
3.93316991781225));
#45647=CARTESIAN_POINT('Ctrl Pts',(-77.0303479441471,1.07916677227421,4.00709314583042));
#45648=CARTESIAN_POINT('Ctrl Pts',(-77.0966391213795,2.4219432494828,3.36980523146763));
#45649=CARTESIAN_POINT('Ctrl Pts',(-77.162930298612,3.18821435754475,2.31407689684504));
#45650=CARTESIAN_POINT('Ctrl Pts',(-77.2292214758445,3.95448546560672,1.25834856222242));
#45651=CARTESIAN_POINT('Ctrl Pts',(-77.2955126530771,4.14425120452202,-0.215820192660025));
#45652=CARTESIAN_POINT('Ctrl Pts',(-77.3618038303095,3.67033299901256,-1.43119472837413));
#45653=CARTESIAN_POINT('Ctrl Pts',(-77.428095007542,3.19641479350313,-2.64656926408816));
#45654=CARTESIAN_POINT('Ctrl Pts',(-77.4943861847744,2.05881264356902,-3.60314958063389));
#45655=CARTESIAN_POINT('Ctrl Pts',(-77.5606773620069,0.780142144793593,
-3.86148169853015));
#45656=CARTESIAN_POINT('Ctrl Pts',(-77.6269685392394,-0.498528353981874,
-4.11981381642642));
#45657=CARTESIAN_POINT('Ctrl Pts',(-77.693259716472,-1.91826720159868,-3.67989773567319));
#45658=CARTESIAN_POINT('Ctrl Pts',(-77.7595508937044,-2.82684491390624,
-2.74383135540231));
#45659=CARTESIAN_POINT('Ctrl Pts',(-77.810646088458,-3.52714859076301,-2.02234026112835));
#45660=CARTESIAN_POINT('Ctrl Pts',(-77.8617412832115,-3.92377905727359,
-1.00609367027775));
#45661=CARTESIAN_POINT('Ctrl Pts',(-77.912836477965,-3.93313541941523,0.00362608069297291));
#45662=CARTESIAN_POINT('Ctrl Pts',(-78.0961635220346,-3.93248803517055,
0.00363500034747385));
#45663=CARTESIAN_POINT('Ctrl Pts',(-78.0461451680581,-3.92344099397065,
-0.985220303633294));
#45664=CARTESIAN_POINT('Ctrl Pts',(-77.9961268140815,-3.54501146993409,
-1.98024419461987));
#45665=CARTESIAN_POINT('Ctrl Pts',(-77.946108460105,-2.87102563211285,-2.69756825565498));
#45666=CARTESIAN_POINT('Ctrl Pts',(-77.8798172828725,-1.97776723644254,
-3.64826440382224));
#45667=CARTESIAN_POINT('Ctrl Pts',(-77.8135261056399,-0.565358775484557,
-4.11117572681156));
#45668=CARTESIAN_POINT('Ctrl Pts',(-77.7472349284074,0.717337853767346,
-3.87364028760014));
#45669=CARTESIAN_POINT('Ctrl Pts',(-77.6809437511749,2.00003448301918,-3.63610484838873));
#45670=CARTESIAN_POINT('Ctrl Pts',(-77.6146525739425,3.15301928056487,-2.69812264697659));
#45671=CARTESIAN_POINT('Ctrl Pts',(-77.54836139671,3.64660984671592,-1.49060366965903));
#45672=CARTESIAN_POINT('Ctrl Pts',(-77.4820702194775,4.14020041286697,-0.283084692341431));
#45673=CARTESIAN_POINT('Ctrl Pts',(-77.415779042245,3.97439674762335,1.19397106088165));
#45674=CARTESIAN_POINT('Ctrl Pts',(-77.3494878650125,3.22536922501803,2.26200266058046));
#45675=CARTESIAN_POINT('Ctrl Pts',(-77.28319668778,2.47634170241269,3.33003426027929));
#45676=CARTESIAN_POINT('Ctrl Pts',(-77.2169055105476,1.14409032244569,3.98904170645383));
#45677=CARTESIAN_POINT('Ctrl Pts',(-77.1506143333151,-0.159347263188599,
3.93627630177059));
#45678=CARTESIAN_POINT('Ctrl Pts',(-77.0843231560826,-1.46278484882285,
3.88351089708735));
#45679=CARTESIAN_POINT('Ctrl Pts',(-77.0180319788501,-2.73740864012438,
3.1189726415463));
#45680=CARTESIAN_POINT('Ctrl Pts',(-76.9517408016176,-3.39765515879417,
1.99389119464573));
#45681=CARTESIAN_POINT('Ctrl Pts',(-76.9165483750899,-3.74816450360395,
1.39661192143539));
#45682=CARTESIAN_POINT('Ctrl Pts',(-76.8813559485623,-3.92552400471929,
0.697720821079181));
#45683=CARTESIAN_POINT('Ctrl Pts',(-76.8461635220347,-3.92658087967646,
-0.000668997711400442));
#45684=CARTESIAN_POINT('Origin',(-54.75,0.,0.));
#45685=CARTESIAN_POINT('',(-75.412836477965,-3.93430794215879,-0.00351519416923518));
#45686=CARTESIAN_POINT('',(-75.5961635220347,-3.93495109289722,-0.00340104241912089));
#45687=CARTESIAN_POINT('',(-54.75,-3.933,-4.81653586104654E-16));
#45688=CARTESIAN_POINT('Ctrl Pts',(-75.412836477965,-3.93430794215879,-0.00351519416923518));
#45689=CARTESIAN_POINT('Ctrl Pts',(-75.4658716669875,-3.92460957776598,
1.04374099397056));
#45690=CARTESIAN_POINT('Ctrl Pts',(-75.51890685601,-3.49386462216488,2.09804064888604));
#45691=CARTESIAN_POINT('Ctrl Pts',(-75.5719420450325,-2.74537760506035,
2.82534324990779));
#45692=CARTESIAN_POINT('Ctrl Pts',(-75.638233222265,-1.80980847781403,3.73443297909794));
#45693=CARTESIAN_POINT('Ctrl Pts',(-75.7045243994974,-0.37780945214924,
4.1326331097266));
#45694=CARTESIAN_POINT('Ctrl Pts',(-75.7708155767298,0.892757649401435,
3.83701009297626));
#45695=CARTESIAN_POINT('Ctrl Pts',(-75.8371067539623,2.16332475095207,3.54138707622592));
#45696=CARTESIAN_POINT('Ctrl Pts',(-75.9033979311948,3.27245992838864,2.5519409120966));
#45697=CARTESIAN_POINT('Ctrl Pts',(-75.9696891084273,3.71062534251835,1.32322418419065));
#45698=CARTESIAN_POINT('Ctrl Pts',(-76.0359802856598,4.14879075664809,0.094507456284634));
#45699=CARTESIAN_POINT('Ctrl Pts',(-76.1022714628923,3.91598640747094,-1.37347983539797));
#45700=CARTESIAN_POINT('Ctrl Pts',(-76.1685626401248,3.11916285200426,-2.40634282196928));
#45701=CARTESIAN_POINT('Ctrl Pts',(-76.2348538173573,2.32233929653761,-3.43920580854055));
#45702=CARTESIAN_POINT('Ctrl Pts',(-76.3011449945897,0.961496534781437,
-4.03694449000047));
#45703=CARTESIAN_POINT('Ctrl Pts',(-76.3674361718222,-0.33819287142288,
-3.92495710242611));
#45704=CARTESIAN_POINT('Ctrl Pts',(-76.4337273490547,-1.6378822776272,-3.81296971485175));
#45705=CARTESIAN_POINT('Ctrl Pts',(-76.5000185262872,-2.8764183282797,-2.99125625824311));
#45706=CARTESIAN_POINT('Ctrl Pts',(-76.5663097035197,-3.48481629018454,
-1.83731273816706));
#45707=CARTESIAN_POINT('Ctrl Pts',(-76.5984852950015,-3.78011296611989,
-1.27722590844014));
#45708=CARTESIAN_POINT('Ctrl Pts',(-76.6306608864832,-3.92696061796596,
-0.638871744020152));
#45709=CARTESIAN_POINT('Ctrl Pts',(-76.662836477965,-3.92650124665457,-0.000318401066521645));
#45710=CARTESIAN_POINT('Ctrl Pts',(-76.8461635220347,-3.92658087967646,
-0.000668997711400442));
#45711=CARTESIAN_POINT('Ctrl Pts',(-76.8150647713298,-3.92751481615262,
-0.617820271787113));
#45712=CARTESIAN_POINT('Ctrl Pts',(-76.783966020625,-3.79077655588946,-1.2345801022648));
#45713=CARTESIAN_POINT('Ctrl Pts',(-76.7528672699202,-3.51419051818756,
-1.78048523612163));
#45714=CARTESIAN_POINT('Ctrl Pts',(-76.6865760926877,-2.92461011287302,
-2.94415558172847));
#45715=CARTESIAN_POINT('Ctrl Pts',(-76.6202849154552,-1.69958005620581,
-3.78587163468196));
#45716=CARTESIAN_POINT('Ctrl Pts',(-76.5539937382227,-0.401880413879147,
-3.91894817611904));
#45717=CARTESIAN_POINT('Ctrl Pts',(-76.4877025609902,0.89581922844744,-4.05202471755611));
#45718=CARTESIAN_POINT('Ctrl Pts',(-76.4214113837578,2.26618845643342,-3.47646174747684));
#45719=CARTESIAN_POINT('Ctrl Pts',(-76.3551202065253,3.07967823987134,-2.45667348522945));
#45720=CARTESIAN_POINT('Ctrl Pts',(-76.2888290292928,3.89316802330925,-1.43688522298207));
#45721=CARTESIAN_POINT('Ctrl Pts',(-76.2225378520603,4.14977836219906,0.0271283314335248));
#45722=CARTESIAN_POINT('Ctrl Pts',(-76.1562466748278,3.73162220340928,1.26279784810924));
#45723=CARTESIAN_POINT('Ctrl Pts',(-76.0899554975953,3.31346604461948,2.49846736478502));
#45724=CARTESIAN_POINT('Ctrl Pts',(-76.0236643203629,2.22054338815007,3.50579284372096));
#45725=CARTESIAN_POINT('Ctrl Pts',(-75.9573731431304,0.954944024417141,
3.822007925737));
#45726=CARTESIAN_POINT('Ctrl Pts',(-75.8910819658979,-0.31065533931575,
4.13822300775303));
#45727=CARTESIAN_POINT('Ctrl Pts',(-75.8247907886653,-1.7489314103121,3.7633276928492));
#45728=CARTESIAN_POINT('Ctrl Pts',(-75.7584996114329,-2.69913868496981,
2.86954927357345));
#45729=CARTESIAN_POINT('Ctrl Pts',(-75.7043875816335,-3.47477198201586,
2.13997760993702));
#45730=CARTESIAN_POINT('Ctrl Pts',(-75.6502755518341,-3.92520026725676,
1.06466905972103));
#45731=CARTESIAN_POINT('Ctrl Pts',(-75.5961635220347,-3.93495109289722,
-0.0034010424191209));
#45732=CARTESIAN_POINT('Origin',(-54.75,0.,0.));
#45733=CARTESIAN_POINT('',(-74.162836477965,-3.93829176197897,0.00197029291977097));
#45734=CARTESIAN_POINT('',(-74.3461635220347,-3.93784216741542,0.00228528798276027));
#45735=CARTESIAN_POINT('',(-54.75,-3.933,-4.81653586104654E-16));
#45736=CARTESIAN_POINT('Ctrl Pts',(-74.162836477965,-3.93829176197897,0.00197029291977097));
#45737=CARTESIAN_POINT('Ctrl Pts',(-74.1685000930268,-3.9389747377774,0.113512333841672));
#45738=CARTESIAN_POINT('Ctrl Pts',(-74.1741637080885,-3.93464848695273,
0.225000608832605));
#45739=CARTESIAN_POINT('Ctrl Pts',(-74.1798273231502,-3.92514155145442,
0.336045346958482));
#45740=CARTESIAN_POINT('Ctrl Pts',(-74.2461185003827,-3.81386528370203,
1.6357958306324));
#45741=CARTESIAN_POINT('Ctrl Pts',(-74.3124096776152,-2.99282959412186,
2.87478128251356));
#45742=CARTESIAN_POINT('Ctrl Pts',(-74.3787008548477,-1.83921912141205,
3.48381051402035));
#45743=CARTESIAN_POINT('Ctrl Pts',(-74.4449920320802,-0.685608648702251,
4.09283974552713));
#45744=CARTESIAN_POINT('Ctrl Pts',(-74.5112832093127,0.800576607137177,
4.07191275665953));
#45745=CARTESIAN_POINT('Ctrl Pts',(-74.5775743865452,1.93658161380189,3.43064342758774));
#45746=CARTESIAN_POINT('Ctrl Pts',(-74.6438655637776,3.07258662046659,2.78937409851594));
#45747=CARTESIAN_POINT('Ctrl Pts',(-74.7101567410101,3.85841137795658,1.52776242923994));
#45748=CARTESIAN_POINT('Ctrl Pts',(-74.7764479182426,3.93304718592474,0.22539411584145));
#45749=CARTESIAN_POINT('Ctrl Pts',(-74.8427390954751,4.00768299389289,-1.076974197557));
#45750=CARTESIAN_POINT('Ctrl Pts',(-74.9090302727075,3.37112985233926,-2.42009915507794));
#45751=CARTESIAN_POINT('Ctrl Pts',(-74.9753214499401,2.31582092800211,-3.18694777233545));
#45752=CARTESIAN_POINT('Ctrl Pts',(-75.0416126271726,1.26051200366493,-3.95379638959298));
#45753=CARTESIAN_POINT('Ctrl Pts',(-75.1079038044051,-0.213552703455776,
-4.14436866658707));
#45754=CARTESIAN_POINT('Ctrl Pts',(-75.1741949816376,-1.42918635358045,
-3.67111550361819));
#45755=CARTESIAN_POINT('Ctrl Pts',(-75.24048615887,-2.64482000370512,-3.19786234064932));
#45756=CARTESIAN_POINT('Ctrl Pts',(-75.3067773361024,-3.60202259683376,
-2.0607837377175));
#45757=CARTESIAN_POINT('Ctrl Pts',(-75.3730685133349,-3.86105427898415,
-0.78225477237576));
#45758=CARTESIAN_POINT('Ctrl Pts',(-75.3863245015449,-3.91285183437474,
-0.526592320775261));
#45759=CARTESIAN_POINT('Ctrl Pts',(-75.399580489755,-3.93673201957639,-0.265273772553341));
#45760=CARTESIAN_POINT('Ctrl Pts',(-75.412836477965,-3.93430794215879,-0.00351519416923518));
#45761=CARTESIAN_POINT('Ctrl Pts',(-75.5961635220347,-3.93495109289722,
-0.0034010424191209));
#45762=CARTESIAN_POINT('Ctrl Pts',(-75.5839843746017,-3.93714573877374,
-0.243794597993349));
#45763=CARTESIAN_POINT('Ctrl Pts',(-75.5718052271686,-3.9170166442977,-0.483821469881175));
#45764=CARTESIAN_POINT('Ctrl Pts',(-75.5596260797355,-3.87324722853908,
-0.719457143116103));
#45765=CARTESIAN_POINT('Ctrl Pts',(-75.493334902503,-3.63501001913161,-2.00202361688233));
#45766=CARTESIAN_POINT('Ctrl Pts',(-75.4270437252704,-2.69639712199763,
-3.15449504076718));
#45767=CARTESIAN_POINT('Ctrl Pts',(-75.3607525480379,-1.48860826569452,
-3.64742485946899));
#45768=CARTESIAN_POINT('Ctrl Pts',(-75.2944613708054,-0.280819409391409,
-4.1403546781708));
#45769=CARTESIAN_POINT('Ctrl Pts',(-75.228170193573,1.19614540608083,-3.97374289168959));
#45770=CARTESIAN_POINT('Ctrl Pts',(-75.1618790163406,2.26376702818862,-3.22413112578451));
#45771=CARTESIAN_POINT('Ctrl Pts',(-75.0955878391081,3.3313886502965,-2.47451935987938));
#45772=CARTESIAN_POINT('Ctrl Pts',(-75.0292966618756,3.98966707903983,-1.14190761455027));
#45773=CARTESIAN_POINT('Ctrl Pts',(-74.9630054846431,3.93618852844139,0.161500906290973));
#45774=CARTESIAN_POINT('Ctrl Pts',(-74.8967143074106,3.88270997784296,1.46490942713211));
#45775=CARTESIAN_POINT('Ctrl Pts',(-74.8304231301781,3.11747444790289,2.73911472348538));
#45776=CARTESIAN_POINT('Ctrl Pts',(-74.7641319529456,1.99203192669418,3.39874557406075));
#45777=CARTESIAN_POINT('Ctrl Pts',(-74.6978407757132,0.866589405485442,
4.05837642463612));
#45778=CARTESIAN_POINT('Ctrl Pts',(-74.6315495984807,-0.619060106991951,
4.10343282943355));
#45779=CARTESIAN_POINT('Ctrl Pts',(-74.5652584212482,-1.78240769948418,
3.51321582983254));
#45780=CARTESIAN_POINT('Ctrl Pts',(-74.4989672440157,-2.9457552919764,2.92299883023154));
#45781=CARTESIAN_POINT('Ctrl Pts',(-74.4326760667832,-3.78680096448347,
1.6975084262321));
#45782=CARTESIAN_POINT('Ctrl Pts',(-74.3663848895507,-3.91916747160762,
0.399736167564488));
#45783=CARTESIAN_POINT('Ctrl Pts',(-74.359644433712,-3.93262643602852,0.267779292405271));
#45784=CARTESIAN_POINT('Ctrl Pts',(-74.3529039778734,-3.93875855994925,
0.135075114875559));
#45785=CARTESIAN_POINT('Ctrl Pts',(-74.3461635220347,-3.93784216741542,
0.00228528798276027));
#45786=CARTESIAN_POINT('Origin',(-54.75,0.,0.));
#45787=CARTESIAN_POINT('',(-72.912836477965,-3.92821364041606,0.00254794616387777));
#45788=CARTESIAN_POINT('',(-73.0961635220347,-3.92781646010829,0.00228144192526316));
#45789=CARTESIAN_POINT('',(-54.75,-3.933,-4.81653586104654E-16));
#45790=CARTESIAN_POINT('Ctrl Pts',(-72.912836477965,-3.92821364041606,0.00254794616387777));
#45791=CARTESIAN_POINT('Ctrl Pts',(-72.9374196962985,-3.93109434647776,
0.48989238060394));
#45792=CARTESIAN_POINT('Ctrl Pts',(-72.962002914632,-3.84714999645044,0.976279715033341));
#45793=CARTESIAN_POINT('Ctrl Pts',(-72.9865861329655,-3.67189690925834,
1.42717755095344));
#45794=CARTESIAN_POINT('Ctrl Pts',(-73.052877310198,-3.1993089305005,2.64306995158314));
#45795=CARTESIAN_POINT('Ctrl Pts',(-73.1191684874305,-2.06275421496071,
3.60089453475158));
#45796=CARTESIAN_POINT('Ctrl Pts',(-73.185459664663,-0.784367165786236,
3.86062570361371));
#45797=CARTESIAN_POINT('Ctrl Pts',(-73.2517508418955,0.494019883388161,
4.12035687247583));
#45798=CARTESIAN_POINT('Ctrl Pts',(-73.3180420191279,1.91423926619718,3.68199462703174));
#45799=CARTESIAN_POINT('Ctrl Pts',(-73.3843331963604,2.8238407401297,2.746923032877));
#45800=CARTESIAN_POINT('Ctrl Pts',(-73.4506243735929,3.73344221406231,1.81185143872218));
#45801=CARTESIAN_POINT('Ctrl Pts',(-73.5169155508254,4.13242577911829,0.380070495856531));
#45802=CARTESIAN_POINT('Ctrl Pts',(-73.5832067280579,3.83749797589989,-0.890658160649008));
#45803=CARTESIAN_POINT('Ctrl Pts',(-73.6494979052904,3.54257017268151,-2.16138681715447));
#45804=CARTESIAN_POINT('Ctrl Pts',(-73.7157890825228,2.55373100118889,-3.27106318729991));
#45805=CARTESIAN_POINT('Ctrl Pts',(-73.7820802597553,1.32525419198386,-3.70990080740653));
#45806=CARTESIAN_POINT('Ctrl Pts',(-73.8483714369878,0.0967773827788009,
-4.14873842751317));
#45807=CARTESIAN_POINT('Ctrl Pts',(-73.9146626142203,-1.37133706413864,
-3.91673729758093));
#45808=CARTESIAN_POINT('Ctrl Pts',(-73.9809537914528,-2.40463586463505,
-3.12047897488147));
#45809=CARTESIAN_POINT('Ctrl Pts',(-74.0415813536236,-3.34965434044744,
-2.39224932232706));
#45810=CARTESIAN_POINT('Ctrl Pts',(-74.1022089157943,-3.93098067935254,
-1.19205895287587));
#45811=CARTESIAN_POINT('Ctrl Pts',(-74.162836477965,-3.93829176197897,0.00197029291977097));
#45812=CARTESIAN_POINT('Ctrl Pts',(-74.3461635220347,-3.93784216741542,
0.00228528798276027));
#45813=CARTESIAN_POINT('Ctrl Pts',(-74.2866128006409,-3.92974600333162,
-1.17088907506766));
#45814=CARTESIAN_POINT('Ctrl Pts',(-74.227062079247,-3.37148448707964,-2.35074871895834));
#45815=CARTESIAN_POINT('Ctrl Pts',(-74.1675113578533,-2.45498812369899,
-3.08102190622906));
#45816=CARTESIAN_POINT('Ctrl Pts',(-74.1012201806208,-1.4347549269249,-3.89395360801932));
#45817=CARTESIAN_POINT('Ctrl Pts',(-74.0349290033883,0.0293988083645495,
-4.14976289826403));
#45818=CARTESIAN_POINT('Ctrl Pts',(-73.9686378261559,1.26483935302405,-3.73093072640168));
#45819=CARTESIAN_POINT('Ctrl Pts',(-73.9023466489234,2.50027989768352,-3.31209855453934));
#45820=CARTESIAN_POINT('Ctrl Pts',(-73.8360554716908,3.50700725171301,-2.21862492056999));
#45821=CARTESIAN_POINT('Ctrl Pts',(-73.7697642944583,3.82252983512861,-0.952852734538805));
#45822=CARTESIAN_POINT('Ctrl Pts',(-73.7034731172259,4.13805241854422,0.312919451492413));
#45823=CARTESIAN_POINT('Ctrl Pts',(-73.6371819399934,3.76237023134582,1.75099018958553));
#45824=CARTESIAN_POINT('Ctrl Pts',(-73.5708907627609,2.86807205602136,2.70070830628483));
#45825=CARTESIAN_POINT('Ctrl Pts',(-73.5045995855285,1.97377388069691,3.65042642298412));
#45826=CARTESIAN_POINT('Ctrl Pts',(-73.4383084082959,0.560859717246415,
4.11179191828967));
#45827=CARTESIAN_POINT('Ctrl Pts',(-73.3720172310634,-0.721576217092039,
3.87285301000355));
#45828=CARTESIAN_POINT('Ctrl Pts',(-73.3057260538309,-2.00401215143046,
3.63391410171745));
#45829=CARTESIAN_POINT('Ctrl Pts',(-73.2394348765985,-3.15596985665681,
2.69467078983973));
#45830=CARTESIAN_POINT('Ctrl Pts',(-73.173143699366,-3.64823878034857,1.48661241610825));
#45831=CARTESIAN_POINT('Ctrl Pts',(-73.1474836402556,-3.83878675682919,
1.01899590101592));
#45832=CARTESIAN_POINT('Ctrl Pts',(-73.1218235811451,-3.93049241100765,
0.511102355713064));
#45833=CARTESIAN_POINT('Ctrl Pts',(-73.0961635220347,-3.92781646010829,
0.00228144192526316));
#45834=CARTESIAN_POINT('Origin',(-54.75,0.,0.));
#45835=CARTESIAN_POINT('',(-71.662836477965,-3.92897287541266,-0.00293764914132633));
#45836=CARTESIAN_POINT('',(-71.8461635220347,-3.92948114538815,-0.00313483220630379));
#45837=CARTESIAN_POINT('',(-54.75,-3.933,-4.81653586104654E-16));
#45838=CARTESIAN_POINT('Ctrl Pts',(-71.662836477965,-3.92897287541266,-0.00293764914132633));
#45839=CARTESIAN_POINT('Ctrl Pts',(-71.7063392995703,-3.92302352206136,
0.859055801694659));
#45840=CARTESIAN_POINT('Ctrl Pts',(-71.7498421211755,-3.64395843373945,
1.72455195491687));
#45841=CARTESIAN_POINT('Ctrl Pts',(-71.7933449427808,-3.12179416362893,
2.40292818746188));
#45842=CARTESIAN_POINT('Ctrl Pts',(-71.8596361200133,-2.3261013120603,3.43666249256066));
#45843=CARTESIAN_POINT('Ctrl Pts',(-71.9259272972458,-0.965913450159726,
4.03588994009282));
#45844=CARTESIAN_POINT('Ctrl Pts',(-71.9922184744783,0.333897721897463,
3.92532482547344));
#45845=CARTESIAN_POINT('Ctrl Pts',(-72.0585096517108,1.63370889395462,3.81475971085407));
#45846=CARTESIAN_POINT('Ctrl Pts',(-72.1248008289432,2.87314337616838,2.9944020340832));
#45847=CARTESIAN_POINT('Ctrl Pts',(-72.1910920061757,3.48280369496138,1.8411249540783));
#45848=CARTESIAN_POINT('Ctrl Pts',(-72.2573831834082,4.09246401375438,0.687847874073377));
#45849=CARTESIAN_POINT('Ctrl Pts',(-72.3236743606407,4.07235016912658,-0.798348609165588));
#45850=CARTESIAN_POINT('Ctrl Pts',(-72.3899655378732,3.43170248194958,-1.93470430545537));
#45851=CARTESIAN_POINT('Ctrl Pts',(-72.4562567151057,2.79105479477258,-3.07106000174515));
#45852=CARTESIAN_POINT('Ctrl Pts',(-72.5225478923381,1.52987326504638,-3.85757491108575));
#45853=CARTESIAN_POINT('Ctrl Pts',(-72.5888390695706,0.22754598230192,-3.93292327666135));
#45854=CARTESIAN_POINT('Ctrl Pts',(-72.6551302468031,-1.07478130044254,
-4.00827164223696));
#45855=CARTESIAN_POINT('Ctrl Pts',(-72.7214214240356,-2.41825433620526,
-3.37245346404756));
#45856=CARTESIAN_POINT('Ctrl Pts',(-72.7877126012681,-3.18568023309867,
-2.31756426590739));
#45857=CARTESIAN_POINT('Ctrl Pts',(-72.8294205601671,-3.6685162469078,-1.65386696626954));
#45858=CARTESIAN_POINT('Ctrl Pts',(-72.871128519066,-3.92332622623003,-0.824282022375144));
#45859=CARTESIAN_POINT('Ctrl Pts',(-72.912836477965,-3.92821364041606,0.00254794616387777));
#45860=CARTESIAN_POINT('Ctrl Pts',(-73.0961635220347,-3.92781646010829,
0.00228144192526316));
#45861=CARTESIAN_POINT('Ctrl Pts',(-73.0555324039126,-3.92357925720035,
-0.803405036117873));
#45862=CARTESIAN_POINT('Ctrl Pts',(-73.0149012857906,-3.6827012670755,-1.61141668343669));
#45863=CARTESIAN_POINT('Ctrl Pts',(-72.9742701676685,-3.22289206139225,
-2.26553071812793));
#45864=CARTESIAN_POINT('Ctrl Pts',(-72.907978990436,-2.47269627658706,-3.33274204304717));
#45865=CARTESIAN_POINT('Ctrl Pts',(-72.8416878132035,-1.13972456481958,
-3.99029125730048));
#45866=CARTESIAN_POINT('Ctrl Pts',(-72.7753966359711,0.163654501047081,
-3.93609957679598));
#45867=CARTESIAN_POINT('Ctrl Pts',(-72.7091054587386,1.46703356691378,-3.88190789629148));
#45868=CARTESIAN_POINT('Ctrl Pts',(-72.6428142815062,2.74081998687971,-3.11597532102913));
#45869=CARTESIAN_POINT('Ctrl Pts',(-72.5765231042737,3.39983497189712,-1.99017206241866));
#45870=CARTESIAN_POINT('Ctrl Pts',(-72.5102319270412,4.05884995691455,-0.86436880380816));
#45871=CARTESIAN_POINT('Ctrl Pts',(-72.4439407498086,4.10309350698347,0.621305138150414));
#45872=CARTESIAN_POINT('Ctrl Pts',(-72.3776495725761,3.51224008978018,1.78432962927463));
#45873=CARTESIAN_POINT('Ctrl Pts',(-72.3113583953437,2.92138667257693,2.94735412039879));
#45874=CARTESIAN_POINT('Ctrl Pts',(-72.2450672181112,1.6954362881015,3.78772916068855));
#45875=CARTESIAN_POINT('Ctrl Pts',(-72.1787760408787,0.397591801587071,
3.91938559387529));
#45876=CARTESIAN_POINT('Ctrl Pts',(-72.1124848636463,-0.900252684927396,
4.05104202706204));
#45877=CARTESIAN_POINT('Ctrl Pts',(-72.0461936864137,-2.26999127348092,
3.47397985314572));
#45878=CARTESIAN_POINT('Ctrl Pts',(-71.9799025091813,-3.08236465026863,
2.45330202725648));
#45879=CARTESIAN_POINT('Ctrl Pts',(-71.9353228467991,-3.62867160056579,
1.76691396207597));
#45880=CARTESIAN_POINT('Ctrl Pts',(-71.8907431844169,-3.92291970365932,
0.879908335057426));
#45881=CARTESIAN_POINT('Ctrl Pts',(-71.8461635220347,-3.92948114538815,
-0.00313483220630379));
#45882=CARTESIAN_POINT('Origin',(-54.75,0.,0.));
#45883=CARTESIAN_POINT('',(-70.412836477965,-3.93890669167694,-0.00139193648397762));
#45884=CARTESIAN_POINT('',(-70.5961635220346,-3.93918182025515,-0.0010191464650001));
#45885=CARTESIAN_POINT('',(-54.75,-3.933,-4.81653586104654E-16));
#45886=CARTESIAN_POINT('Ctrl Pts',(-70.412836477965,-3.93890669167694,-0.00139193648397762));
#45887=CARTESIAN_POINT('Ctrl Pts',(-70.475258902842,-3.93330383208432,1.22747763377414));
#45888=CARTESIAN_POINT('Ctrl Pts',(-70.5376813277191,-3.31223725813826,
2.46122943672829));
#45889=CARTESIAN_POINT('Ctrl Pts',(-70.6001037525961,-2.31930691003918,
3.18441174021372));
#45890=CARTESIAN_POINT('Ctrl Pts',(-70.6663949298286,-1.26483775388198,
3.95241468701055));
#45891=CARTESIAN_POINT('Ctrl Pts',(-70.7326861070611,0.209017533942394,
4.14459986877461));
#45892=CARTESIAN_POINT('Ctrl Pts',(-70.7989772842936,1.42516832109412,3.67267721569922));
#45893=CARTESIAN_POINT('Ctrl Pts',(-70.865268461526,2.64131910824584,3.20075456262383));
#45894=CARTESIAN_POINT('Ctrl Pts',(-70.9315596387585,3.59976539472492,2.06472407470899));
#45895=CARTESIAN_POINT('Ctrl Pts',(-70.997850815991,3.86019597254711,0.786479324392882));
#45896=CARTESIAN_POINT('Ctrl Pts',(-71.0641419932234,4.1206265503693,-0.491765425923184));
#45897=CARTESIAN_POINT('Ctrl Pts',(-71.130433170456,3.68304141953466,-1.9122244386405));
#45898=CARTESIAN_POINT('Ctrl Pts',(-71.1967243476885,2.74846763838938,-2.82233738502199));
#45899=CARTESIAN_POINT('Ctrl Pts',(-71.263015524921,1.8138938572441,-3.73245033140348));
#45900=CARTESIAN_POINT('Ctrl Pts',(-71.3293067021534,0.382331425788183,
-4.13221721144915));
#45901=CARTESIAN_POINT('Ctrl Pts',(-71.3955978793859,-0.888558405273612,
-3.83798471005084));
#45902=CARTESIAN_POINT('Ctrl Pts',(-71.4618890566184,-2.15944823633548,
-3.54375220865252));
#45903=CARTESIAN_POINT('Ctrl Pts',(-71.5281802338509,-3.2696654670032,-2.55552032581013));
#45904=CARTESIAN_POINT('Ctrl Pts',(-71.5944714110833,-3.70917516171872,
-1.32728380305621));
#45905=CARTESIAN_POINT('Ctrl Pts',(-71.6172597667106,-3.86026168096495,
-0.905063353165785));
#45906=CARTESIAN_POINT('Ctrl Pts',(-71.6400481223378,-3.93208936245692,
-0.454481079685571));
#45907=CARTESIAN_POINT('Ctrl Pts',(-71.662836477965,-3.92897287541266,-0.00293764914132633));
#45908=CARTESIAN_POINT('Ctrl Pts',(-71.8461635220347,-3.92948114538815,
-0.00313483220630379));
#45909=CARTESIAN_POINT('Ctrl Pts',(-71.8244520071844,-3.93267674696794,
-0.433201006218865));
#45910=CARTESIAN_POINT('Ctrl Pts',(-71.8027404923342,-3.86763432678414,
-0.862327302053894));
#45911=CARTESIAN_POINT('Ctrl Pts',(-71.7810289774839,-3.73023813252271,
-1.26688047930335));
#45912=CARTESIAN_POINT('Ctrl Pts',(-71.7147378002514,-3.31073007296715,
-2.50209168211176));
#45913=CARTESIAN_POINT('Ctrl Pts',(-71.6484466230188,-2.21670578883407,
-3.50822060986641));
#45914=CARTESIAN_POINT('Ctrl Pts',(-71.5821554457863,-0.950761159419275,
-3.82305060022833));
#45915=CARTESIAN_POINT('Ctrl Pts',(-71.5158642685538,0.315183469995524,
-4.13788059059025));
#45916=CARTESIAN_POINT('Ctrl Pts',(-71.4495730913214,1.75304844469209,-3.76141164355944));
#45917=CARTESIAN_POINT('Ctrl Pts',(-71.3832819140889,2.70227711913041,-2.86659397989856));
#45918=CARTESIAN_POINT('Ctrl Pts',(-71.3169907368564,3.65150579356876,-1.97177631623766));
#45919=CARTESIAN_POINT('Ctrl Pts',(-71.2506995596239,4.11209816774887,-0.558609935946732));
#45920=CARTESIAN_POINT('Ctrl Pts',(-71.1844083823915,3.87245763211158,0.723695075060797));
#45921=CARTESIAN_POINT('Ctrl Pts',(-71.118117205159,3.6328170964743,2.00600008606825));
#45922=CARTESIAN_POINT('Ctrl Pts',(-71.0518260279265,2.69294365101965,3.15744372779227));
#45923=CARTESIAN_POINT('Ctrl Pts',(-70.985534850694,1.48461612149768,3.64905160911101));
#45924=CARTESIAN_POINT('Ctrl Pts',(-70.9192436734615,0.276288591975673,
4.14065949042975));
#45925=CARTESIAN_POINT('Ctrl Pts',(-70.8529524962291,-1.2004930216137,3.97243161134319));
#45926=CARTESIAN_POINT('Ctrl Pts',(-70.7866613189966,-2.26729372986987,
3.22165203221254));
#45927=CARTESIAN_POINT('Ctrl Pts',(-70.7231620533426,-3.28916518247389,
2.50249219928951));
#45928=CARTESIAN_POINT('Ctrl Pts',(-70.6596627876886,-3.93486194413388,
1.24881672704683));
#45929=CARTESIAN_POINT('Ctrl Pts',(-70.5961635220346,-3.93918182025515,
-0.0010191464650001));
#45930=CARTESIAN_POINT('Origin',(-54.75,0.,0.));
#45931=CARTESIAN_POINT('',(-69.162836477965,-3.93322311813782,0.00362201478885243));
#45932=CARTESIAN_POINT('',(-69.3461635220347,-3.93257483085417,0.00363597296250955));
#45933=CARTESIAN_POINT('',(-54.75,-3.933,-4.81653586104654E-16));
#45934=CARTESIAN_POINT('Ctrl Pts',(-69.162836477965,-3.93322311813782,0.00362201478885243));
#45935=CARTESIAN_POINT('Ctrl Pts',(-69.1778873288813,-3.93598182100683,
0.301033048827567));
#45936=CARTESIAN_POINT('Ctrl Pts',(-69.1929381797976,-3.90511541289923,
0.597877093525298));
#45937=CARTESIAN_POINT('Ctrl Pts',(-69.2079890307139,-3.83847029528325,
0.886458383904474));
#45938=CARTESIAN_POINT('Ctrl Pts',(-69.2742802079464,-3.54493318378476,
2.15750900907587));
#45939=CARTESIAN_POINT('Ctrl Pts',(-69.3405713851789,-2.55730888542445,
3.26826676791706));
#45940=CARTESIAN_POINT('Ctrl Pts',(-69.4068625624114,-1.32931301680002,
3.70844840567217));
#45941=CARTESIAN_POINT('Ctrl Pts',(-69.4731537396439,-0.101317148175545,
4.1486300434273));
#45942=CARTESIAN_POINT('Ctrl Pts',(-69.5394449168763,1.36705029071311,3.91823556009631));
#45943=CARTESIAN_POINT('Ctrl Pts',(-69.6057360941088,2.40121979096113,3.1231084178528));
#45944=CARTESIAN_POINT('Ctrl Pts',(-69.6720272713413,3.43538929120911,2.32798127560932));
#45945=CARTESIAN_POINT('Ctrl Pts',(-69.7383184485738,4.0353608528165,0.96812147445346));
#45946=CARTESIAN_POINT('Ctrl Pts',(-69.8046096258063,3.92550692442834,-0.331749996882508));
#45947=CARTESIAN_POINT('Ctrl Pts',(-69.8709008030388,3.81565299604018,-1.63162146821851));
#45948=CARTESIAN_POINT('Ctrl Pts',(-69.9371919802712,2.99597357765637,-2.87150460973458));
#45949=CARTESIAN_POINT('Ctrl Pts',(-70.0034831575037,1.84303023559508,-3.48179583330912));
#45950=CARTESIAN_POINT('Ctrl Pts',(-70.0697743347362,0.690086893533902,
-4.09208705688362));
#45951=CARTESIAN_POINT('Ctrl Pts',(-70.1360655119687,-0.796120372204718,
-4.07278636251674));
#45952=CARTESIAN_POINT('Ctrl Pts',(-70.2023566892012,-1.93282641794617,
-3.43276050901542));
#45953=CARTESIAN_POINT('Ctrl Pts',(-70.2686478664337,-3.06953246368769,
-2.79273465551406));
#45954=CARTESIAN_POINT('Ctrl Pts',(-70.3349390436661,-3.85673728943204,
-1.53198364287817));
#45955=CARTESIAN_POINT('Ctrl Pts',(-70.4012302208986,-3.93279819005921,
-0.229697780645444));
#45956=CARTESIAN_POINT('Ctrl Pts',(-70.4050989732541,-3.93723710336179,
-0.153696392416323));
#45957=CARTESIAN_POINT('Ctrl Pts',(-70.4089677256096,-3.93925393990206,
-0.0775535411296101));
#45958=CARTESIAN_POINT('Ctrl Pts',(-70.412836477965,-3.93890669167694,-0.00139193648397762));
#45959=CARTESIAN_POINT('Ctrl Pts',(-70.5961635220346,-3.93918182025515,
-0.0010191464650001));
#45960=CARTESIAN_POINT('Ctrl Pts',(-70.5933716104561,-3.93937175492662,
-0.055971455134686));
#45961=CARTESIAN_POINT('Ctrl Pts',(-70.5905796988776,-3.93832181084376,
-0.110916341277931));
#45962=CARTESIAN_POINT('Ctrl Pts',(-70.587787787299,-3.93600944686095,-0.165808046812569));
#45963=CARTESIAN_POINT('Ctrl Pts',(-70.5214966100666,-3.88110465267288,
-1.4691572675323));
#45964=CARTESIAN_POINT('Ctrl Pts',(-70.4552054328341,-3.1144752613737,-2.74252442979698));
#45965=CARTESIAN_POINT('Ctrl Pts',(-70.3889142556016,-1.98831160237584,
-3.40092335197723));
#45966=CARTESIAN_POINT('Ctrl Pts',(-70.3226230783692,-0.862147943378008,
-4.05932227415747));
#45967=CARTESIAN_POINT('Ctrl Pts',(-70.2563319011367,0.623549983318482,
-4.10275295625333));
#45968=CARTESIAN_POINT('Ctrl Pts',(-70.1900407239042,1.78625102491787,-3.51126329832246));
#45969=CARTESIAN_POINT('Ctrl Pts',(-70.1237495466717,2.94895206651719,-2.91977364039161));
#45970=CARTESIAN_POINT('Ctrl Pts',(-70.0574583694392,3.78865622301945,-1.69336364243412));
#45971=CARTESIAN_POINT('Ctrl Pts',(-69.9911671922067,3.91960254285678,-0.395447316588599));
#45972=CARTESIAN_POINT('Ctrl Pts',(-69.9248760149742,4.05054886269412,0.902469009256999));
#45973=CARTESIAN_POINT('Ctrl Pts',(-69.8585848377417,3.47273734586645,2.27189166299064));
#45974=CARTESIAN_POINT('Ctrl Pts',(-69.7922936605093,2.45161519640667,3.0837064715881));
#45975=CARTESIAN_POINT('Ctrl Pts',(-69.7260024832768,1.43049304694693,3.89552128018553));
#45976=CARTESIAN_POINT('Ctrl Pts',(-69.6597113060443,-0.0339397351450109,
4.14972824364682));
#45977=CARTESIAN_POINT('Ctrl Pts',(-69.5934201288118,-1.26892122633613,
3.72954442197972));
#45978=CARTESIAN_POINT('Ctrl Pts',(-69.5271289515793,-2.50390271752731,
3.3093606003126));
#45979=CARTESIAN_POINT('Ctrl Pts',(-69.4608377743468,-3.50943291781767,
2.21478599351716));
#45980=CARTESIAN_POINT('Ctrl Pts',(-69.3945465971143,-3.82357022088014,
0.948669299685104));
#45981=CARTESIAN_POINT('Ctrl Pts',(-69.3784189054211,-3.89999531671704,
0.640641285426741));
#45982=CARTESIAN_POINT('Ctrl Pts',(-69.3622912137279,-3.93549831598826,
0.322460054554594));
#45983=CARTESIAN_POINT('Ctrl Pts',(-69.3461635220347,-3.93257483085417,
0.00363597296250955));
#45984=CARTESIAN_POINT('Origin',(-54.75,0.,0.));
#45985=CARTESIAN_POINT('',(-67.912836477965,-3.92649485000913,-0.000270854727073278));
#45986=CARTESIAN_POINT('',(-68.0961635220347,-3.92656685147973,-0.000622033211550006));
#45987=CARTESIAN_POINT('',(-54.75,-3.933,-4.81653586104654E-16));
#45988=CARTESIAN_POINT('Ctrl Pts',(-67.912836477965,-3.92649485000913,-0.000270854727073278));
#45989=CARTESIAN_POINT('Ctrl Pts',(-67.9468069321531,-3.92608231427559,
0.673905878798062));
#45990=CARTESIAN_POINT('Ctrl Pts',(-67.9807773863412,-3.76147556737439,
1.3482714594993));
#45991=CARTESIAN_POINT('Ctrl Pts',(-68.0147478405292,-3.43381750846848,
1.93094795183655));
#45992=CARTESIAN_POINT('Ctrl Pts',(-68.0810390177617,-2.79441368023744,
3.06800400675157));
#45993=CARTESIAN_POINT('Ctrl Pts',(-68.1473301949941,-1.53409356210357,
3.8558985132462));
#45994=CARTESIAN_POINT('Ctrl Pts',(-68.2136213722266,-0.231849510227881,
3.93267192615574));
#45995=CARTESIAN_POINT('Ctrl Pts',(-68.279912549459,1.07039454164785,4.0094453390653));
#45996=CARTESIAN_POINT('Ctrl Pts',(-68.3462037266916,2.41456252726537,3.37509765838973));
#45997=CARTESIAN_POINT('Ctrl Pts',(-68.4124949039241,3.18314229406039,2.32104885987572));
#45998=CARTESIAN_POINT('Ctrl Pts',(-68.4787860811566,3.95172206085539,1.26700006136175));
#45999=CARTESIAN_POINT('Ctrl Pts',(-68.545077258389,4.1447136088279,-0.206749854990709));
#46000=CARTESIAN_POINT('Ctrl Pts',(-68.6113684356215,3.6734564227072,-1.42315866460408));
#46001=CARTESIAN_POINT('Ctrl Pts',(-68.677659612854,3.20219923658649,-2.63956747421748));
#46002=CARTESIAN_POINT('Ctrl Pts',(-68.7439507900865,2.06669331637259,-3.59863517709184));
#46003=CARTESIAN_POINT('Ctrl Pts',(-68.810241967319,0.78859124756331,-3.859765085913));
#46004=CARTESIAN_POINT('Ctrl Pts',(-68.8765331445515,-0.489510821245967,
-4.12089499473416));
#46005=CARTESIAN_POINT('Ctrl Pts',(-68.942824321784,-1.91020903865058,-3.6840871095021));
#46006=CARTESIAN_POINT('Ctrl Pts',(-69.0091154990165,-2.82083318503453,
-2.75001142113526));
#46007=CARTESIAN_POINT('Ctrl Pts',(-69.0603558253326,-3.52470782356272,
-2.02800971481332));
#46008=CARTESIAN_POINT('Ctrl Pts',(-69.1115961516488,-3.9238311684066,-1.00890800885872));
#46009=CARTESIAN_POINT('Ctrl Pts',(-69.162836477965,-3.93322311813782,0.00362201478885243));
#46010=CARTESIAN_POINT('Ctrl Pts',(-69.3461635220347,-3.93257483085417,
0.00363597296250955));
#46011=CARTESIAN_POINT('Ctrl Pts',(-69.2960000364954,-3.92348163840994,
-0.988032736405674));
#46012=CARTESIAN_POINT('Ctrl Pts',(-69.2458365509562,-3.54262932001757,
-1.98592074023852));
#46013=CARTESIAN_POINT('Ctrl Pts',(-69.195673065417,-2.86511504564769,-2.70384512303677));
#46014=CARTESIAN_POINT('Ctrl Pts',(-69.1293818881845,-1.96977816151819,
-3.65258407105819));
#46015=CARTESIAN_POINT('Ctrl Pts',(-69.063090710952,-0.556359987424546,
-4.11240318623246));
#46016=CARTESIAN_POINT('Ctrl Pts',(-68.9967995337195,0.725813716388092,
-3.8720610949815));
#46017=CARTESIAN_POINT('Ctrl Pts',(-68.930508356487,2.00798742020073,-3.63171900373054));
#46018=CARTESIAN_POINT('Ctrl Pts',(-68.8642171792545,3.15891665373242,-2.69121570605441));
#46019=CARTESIAN_POINT('Ctrl Pts',(-68.797926002022,3.64986334551302,-1.4826193824603));
#46020=CARTESIAN_POINT('Ctrl Pts',(-68.7316348247895,4.14081003729361,-0.274023058866195));
#46021=CARTESIAN_POINT('Ctrl Pts',(-68.6653436475571,3.97177418732311,1.20266629064584));
#46022=CARTESIAN_POINT('Ctrl Pts',(-68.5990524703246,3.22041103861628,2.26905606288714));
#46023=CARTESIAN_POINT('Ctrl Pts',(-68.5327612930921,2.46904788990946,3.33544583512841));
#46024=CARTESIAN_POINT('Ctrl Pts',(-68.4664701158596,1.13535744246639,3.99153603009894));
#46025=CARTESIAN_POINT('Ctrl Pts',(-68.4001789386271,-0.167961542942652,
3.9359181386633));
#46026=CARTESIAN_POINT('Ctrl Pts',(-68.3338877613946,-1.47128052835169,
3.88030024722765));
#46027=CARTESIAN_POINT('Ctrl Pts',(-68.2675965841621,-2.74422805172676,
3.11297426938576));
#46028=CARTESIAN_POINT('Ctrl Pts',(-68.2013054069296,-3.40201071397511,
1.98645054712294));
#46029=CARTESIAN_POINT('Ctrl Pts',(-68.1662581119647,-3.74977196892805,
1.39087190713674));
#46030=CARTESIAN_POINT('Ctrl Pts',(-68.1312108169997,-3.9255884166725,0.694893860719782));
#46031=CARTESIAN_POINT('Ctrl Pts',(-68.0961635220347,-3.92656685147973,
-0.000622033211550006));
#46032=CARTESIAN_POINT('Origin',(-54.75,0.,0.));
#46033=CARTESIAN_POINT('',(-66.6628364779651,-3.93422056738883,-0.0035277183879312));
#46034=CARTESIAN_POINT('',(-66.8461635220347,-3.93486507000708,-0.00341859851677232));
#46035=CARTESIAN_POINT('',(-54.75,-3.933,-4.81653586104654E-16));
#46036=CARTESIAN_POINT('Ctrl Pts',(-66.6628364779651,-3.93422056738883,
-0.0035277183879312));
#46037=CARTESIAN_POINT('Ctrl Pts',(-66.7157265354249,-3.92453720768234,
1.04092228063237));
#46038=CARTESIAN_POINT('Ctrl Pts',(-66.7686165928847,-3.49640399633483,
2.09238394656257));
#46039=CARTESIAN_POINT('Ctrl Pts',(-66.8215066503445,-2.75155438065251,
2.81932814061762));
#46040=CARTESIAN_POINT('Ctrl Pts',(-66.8877978275769,-1.81797706468404,
3.73046321440442));
#46041=CARTESIAN_POINT('Ctrl Pts',(-66.9540890048094,-0.386852941616121,
4.13179636517881));
#46042=CARTESIAN_POINT('Ctrl Pts',(-67.0203801820419,0.884358097169925,
3.83895473145184));
#46043=CARTESIAN_POINT('Ctrl Pts',(-67.0866713592744,2.15556913595601,3.54611309772486));
#46044=CARTESIAN_POINT('Ctrl Pts',(-67.1529625365069,3.26686709046021,2.55909667949649));
#46045=CARTESIAN_POINT('Ctrl Pts',(-67.2192537137394,3.70772053948449,1.33134183260772));
#46046=CARTESIAN_POINT('Ctrl Pts',(-67.2855448909718,4.14857398850876,0.103586985718978));
#46047=CARTESIAN_POINT('Ctrl Pts',(-67.3518360682043,3.91898293205315,-1.36490628983015));
#46048=CARTESIAN_POINT('Ctrl Pts',(-67.4181272454368,3.12442173715988,-2.39951067564395));
#46049=CARTESIAN_POINT('Ctrl Pts',(-67.4844184226693,2.32986054226658,-3.43411506145778));
#46050=CARTESIAN_POINT('Ctrl Pts',(-67.5507095999018,0.970329208935581,
-4.03483055753626));
#46051=CARTESIAN_POINT('Ctrl Pts',(-67.6170007771343,-0.329602172556657,
-3.92568784826461));
#46052=CARTESIAN_POINT('Ctrl Pts',(-67.6832919543668,-1.6295335540489,-3.81654513899295));
#46053=CARTESIAN_POINT('Ctrl Pts',(-67.7495831315992,-2.86986498370238,
-2.99754422437115));
#46054=CARTESIAN_POINT('Ctrl Pts',(-67.8158743088317,-3.48078692936503,
-1.84493496539254));
#46055=CARTESIAN_POINT('Ctrl Pts',(-67.8481950318761,-3.77864615938421,
-1.28297233034601));
#46056=CARTESIAN_POINT('Ctrl Pts',(-67.8805157549206,-3.92688735147866,
-0.641707067697644));
#46057=CARTESIAN_POINT('Ctrl Pts',(-67.912836477965,-3.92649485000913,-0.000270854727073278));
#46058=CARTESIAN_POINT('Ctrl Pts',(-68.0961635220347,-3.92656685147973,
-0.000622033211550006));
#46059=CARTESIAN_POINT('Ctrl Pts',(-68.0649196397672,-3.92743910430135,
-0.620658949808565));
#46060=CARTESIAN_POINT('Ctrl Pts',(-68.0336757574997,-3.78936190461529,
-1.24032857880161));
#46061=CARTESIAN_POINT('Ctrl Pts',(-68.0024318752322,-3.51028545575193,
-1.7881718858384));
#46062=CARTESIAN_POINT('Ctrl Pts',(-67.9361406979997,-2.91815973415871,
-2.95054912985305));
#46063=CARTESIAN_POINT('Ctrl Pts',(-67.8698495207672,-1.69129048985058,
-3.78958215119858));
#46064=CARTESIAN_POINT('Ctrl Pts',(-67.8035583435347,-0.393302713211145,
-3.91981831848712));
#46065=CARTESIAN_POINT('Ctrl Pts',(-67.7372671663022,0.904685063428323,
-4.05005448577567));
#46066=CARTESIAN_POINT('Ctrl Pts',(-67.6709759890698,2.27379137239909,-3.47149379900719));
#46067=CARTESIAN_POINT('Ctrl Pts',(-67.6046848118373,3.08504736978577,-2.44992763165452));
#46068=CARTESIAN_POINT('Ctrl Pts',(-67.5383936346048,3.89630336717245,-1.42836146430185));
#46069=CARTESIAN_POINT('Ctrl Pts',(-67.4721024573723,4.14970905297504,0.0362101836350086));
#46070=CARTESIAN_POINT('Ctrl Pts',(-67.4058112801398,3.72884959498036,1.27096159351147));
#46071=CARTESIAN_POINT('Ctrl Pts',(-67.3395201029073,3.30799013698569,2.50571300338793));
#46072=CARTESIAN_POINT('Ctrl Pts',(-67.2732289256748,2.21286553519374,3.51064417520398));
#46073=CARTESIAN_POINT('Ctrl Pts',(-67.2069377484424,0.946577155962392,
3.82408869692854));
#46074=CARTESIAN_POINT('Ctrl Pts',(-67.1406465712099,-0.319711223268989,
4.1375332186531));
#46075=CARTESIAN_POINT('Ctrl Pts',(-67.0743553939774,-1.75716337993967,
3.75949109028616));
#46076=CARTESIAN_POINT('Ctrl Pts',(-67.008064216745,-2.70541231753474,2.86363525371122));
#46077=CARTESIAN_POINT('Ctrl Pts',(-66.9540973185082,-3.47737106158938,
2.13432914110926));
#46078=CARTESIAN_POINT('Ctrl Pts',(-66.9001304202714,-3.92511506363844,
1.06184695920244));
#46079=CARTESIAN_POINT('Ctrl Pts',(-66.8461635220347,-3.93486507000708,
-0.00341859851677232));
#46080=CARTESIAN_POINT('Origin',(-54.75,0.,0.));
#46081=CARTESIAN_POINT('',(-65.412836477965,-3.93834804191526,0.00192586831589278));
#46082=CARTESIAN_POINT('',(-65.5961635220347,-3.93790589778391,0.0022443990911959));
#46083=CARTESIAN_POINT('',(-54.75,-3.933,-4.81653586104654E-16));
#46084=CARTESIAN_POINT('Ctrl Pts',(-65.412836477965,-3.93834804191526,0.00192586831589278));
#46085=CARTESIAN_POINT('Ctrl Pts',(-65.4183549614641,-3.93900111014635,
0.110605513045279));
#46086=CARTESIAN_POINT('Ctrl Pts',(-65.4238734449632,-3.93489409538351,
0.21923504688863));
#46087=CARTESIAN_POINT('Ctrl Pts',(-65.4293919284623,-3.92586759692805,
0.327454249562873));
#46088=CARTESIAN_POINT('Ctrl Pts',(-65.4956831056947,-3.81743613944527,
1.62744515207093));
#46089=CARTESIAN_POINT('Ctrl Pts',(-65.5619742829273,-2.99911397375712,
2.86822449856297));
#46090=CARTESIAN_POINT('Ctrl Pts',(-65.6282654601598,-1.84683914289999,
3.47977698343139));
#46091=CARTESIAN_POINT('Ctrl Pts',(-65.6945566373923,-0.694564312042931,
4.09132946829977));
#46092=CARTESIAN_POINT('Ctrl Pts',(-65.7608478146247,0.791663183983091,
4.07365509154464));
#46093=CARTESIAN_POINT('Ctrl Pts',(-65.8271389918572,1.92906890768864,3.43487347999244));
#46094=CARTESIAN_POINT('Ctrl Pts',(-65.8934301690896,3.06647463139425,2.79609186844021));
#46095=CARTESIAN_POINT('Ctrl Pts',(-65.9597213463221,3.85505858277934,1.53620302209095));
#46096=CARTESIAN_POINT('Ctrl Pts',(-66.0260125235546,3.93254448498876,0.234001170404978));
#46097=CARTESIAN_POINT('Ctrl Pts',(-66.0923037007871,4.01003038719819,-1.06820068128095));
#46098=CARTESIAN_POINT('Ctrl Pts',(-66.1585948780196,3.37641824023196,-2.41271553830341));
#46099=CARTESIAN_POINT('Ctrl Pts',(-66.2248860552521,2.32279011489556,-3.1818718950187));
#46100=CARTESIAN_POINT('Ctrl Pts',(-66.2911772324846,1.26916198955922,-3.95102825173394));
#46101=CARTESIAN_POINT('Ctrl Pts',(-66.3574684097171,-0.20448211414741,
-4.14482610814199));
#46102=CARTESIAN_POINT('Ctrl Pts',(-66.4237595869495,-1.42114858208481,
-3.67423453004905));
#46103=CARTESIAN_POINT('Ctrl Pts',(-66.490050764182,-2.63781505002231,-3.20364295195607));
#46104=CARTESIAN_POINT('Ctrl Pts',(-66.5563419414145,-3.59750388219069,
-2.068661939362));
#46105=CARTESIAN_POINT('Ctrl Pts',(-66.622633118647,-3.85933304384037,-0.790702934665299));
#46106=CARTESIAN_POINT('Ctrl Pts',(-66.6360342384197,-3.91226322402019,
-0.532356614664742));
#46107=CARTESIAN_POINT('Ctrl Pts',(-66.6494353581924,-3.93667410723093,
-0.268167240553048));
#46108=CARTESIAN_POINT('Ctrl Pts',(-66.6628364779651,-3.93422056738883,
-0.0035277183879312));
#46109=CARTESIAN_POINT('Ctrl Pts',(-66.8461635220347,-3.93486507000708,
-0.00341859851677232));
#46110=CARTESIAN_POINT('Ctrl Pts',(-66.8338392430389,-3.93709165338732,
-0.246690499753148));
#46111=CARTESIAN_POINT('Ctrl Pts',(-66.8215149640432,-3.91647612331212,
-0.489586042066614));
#46112=CARTESIAN_POINT('Ctrl Pts',(-66.8091906850475,-3.87166339873204,
-0.727932140439692));
#46113=CARTESIAN_POINT('Ctrl Pts',(-66.742899507815,-3.63061982381493,-2.00997415323278));
#46114=CARTESIAN_POINT('Ctrl Pts',(-66.6766083305825,-2.68948695546139,
-3.16038863403615));
#46115=CARTESIAN_POINT('Ctrl Pts',(-66.6103171533501,-1.48062219959417,
-3.65067398931148));
#46116=CARTESIAN_POINT('Ctrl Pts',(-66.5440259761176,-0.271757443726919,
-4.14095934458682));
#46117=CARTESIAN_POINT('Ctrl Pts',(-66.4777347988851,1.20483919965406,-3.9711155743341));
#46118=CARTESIAN_POINT('Ctrl Pts',(-66.4114436216526,2.2708177166518,-3.2191690809752));
#46119=CARTESIAN_POINT('Ctrl Pts',(-66.3451524444201,3.33679623364958,-2.46722258761628));
#46120=CARTESIAN_POINT('Ctrl Pts',(-66.2788612671875,3.9921566242641,-1.13317337115124));
#46121=CARTESIAN_POINT('Ctrl Pts',(-66.2125700899551,3.93582565223036,0.170114988792669));
#46122=CARTESIAN_POINT('Ctrl Pts',(-66.1462789127226,3.87949468019661,1.47340334873654));
#46123=CARTESIAN_POINT('Ctrl Pts',(-66.0799877354902,3.11147234551458,2.74593085215923));
#46124=CARTESIAN_POINT('Ctrl Pts',(-66.0136965582577,1.98458889721679,3.4030970575654));
#46125=CARTESIAN_POINT('Ctrl Pts',(-65.9474053810252,0.857705448919006,
4.06026326297157));
#46126=CARTESIAN_POINT('Ctrl Pts',(-65.8811142037926,-0.628039112994567,
4.10206817036125));
#46127=CARTESIAN_POINT('Ctrl Pts',(-65.8148230265601,-1.79009221146151,
3.50930656236118));
#46128=CARTESIAN_POINT('Ctrl Pts',(-65.7485318493276,-2.95214530992843,
2.91654495436113));
#46129=CARTESIAN_POINT('Ctrl Pts',(-65.6822406720953,-3.79050694494877,
1.68921683097136));
#46130=CARTESIAN_POINT('Ctrl Pts',(-65.6159494948628,-3.92003292070173,
0.391157992096705));
#46131=CARTESIAN_POINT('Ctrl Pts',(-65.6093541705868,-3.93291948944168,
0.262013823458523));
#46132=CARTESIAN_POINT('Ctrl Pts',(-65.6027588463107,-3.93878978643022,
0.132169540605536));
#46133=CARTESIAN_POINT('Ctrl Pts',(-65.5961635220347,-3.93790589778391,
0.0022443990911959));
#46134=CARTESIAN_POINT('Origin',(-54.75,0.,0.));
#46135=CARTESIAN_POINT('',(-64.1628364779651,-3.92827063990554,0.00258208764951584));
#46136=CARTESIAN_POINT('',(-64.3461635220347,-3.92786728767746,0.00231866363322961));
#46137=CARTESIAN_POINT('',(-54.75,-3.933,-4.81653586104654E-16));
#46138=CARTESIAN_POINT('Ctrl Pts',(-64.1628364779651,-3.92827063990554,
0.00258208764951584));
#46139=CARTESIAN_POINT('Ctrl Pts',(-64.1872745647359,-3.93117530062354,
0.487031767005991));
#46140=CARTESIAN_POINT('Ctrl Pts',(-64.2117126515067,-3.84824859058194,
0.970521987776141));
#46141=CARTESIAN_POINT('Ctrl Pts',(-64.2361507382776,-3.67501153749169,
1.41913807413845));
#46142=CARTESIAN_POINT('Ctrl Pts',(-64.3024419155101,-3.20508570830013,
2.6360618361852));
#46143=CARTESIAN_POINT('Ctrl Pts',(-64.3687330927425,-2.07062994308782,
3.59637151036013));
#46144=CARTESIAN_POINT('Ctrl Pts',(-64.435024269975,-0.792814385066712,
3.85889984645854));
#46145=CARTESIAN_POINT('Ctrl Pts',(-64.5013154472075,0.485001172954427,
4.12142818255696));
#46146=CARTESIAN_POINT('Ctrl Pts',(-64.56760662444,1.90617652378437,3.68617518057882));
#46147=CARTESIAN_POINT('Ctrl Pts',(-64.6338978016725,2.81782225222164,2.7530965164794));
#46148=CARTESIAN_POINT('Ctrl Pts',(-64.7001889789049,3.72946798065891,1.82001785237999));
#46149=CARTESIAN_POINT('Ctrl Pts',(-64.7664801561375,4.13158408670352,0.389113526159296));
#46150=CARTESIAN_POINT('Ctrl Pts',(-64.8327713333699,3.83943801841159,-0.882257545698581));
#46151=CARTESIAN_POINT('Ctrl Pts',(-64.8990625106024,3.54729195011966,-2.15362861755646));
#46152=CARTESIAN_POINT('Ctrl Pts',(-64.9653536878349,2.56088370749119,-3.26546643505152));
#46153=CARTESIAN_POINT('Ctrl Pts',(-65.0316448650673,1.3333702498722,-3.70699156337349));
#46154=CARTESIAN_POINT('Ctrl Pts',(-65.0979360422998,0.105856792253199,
-4.14851669169545));
#46155=CARTESIAN_POINT('Ctrl Pts',(-65.1642272195323,-1.36276188035633,
-3.91972913084432));
#46156=CARTESIAN_POINT('Ctrl Pts',(-65.2305183967648,-2.39780084202234,
-3.12573412115672));
#46157=CARTESIAN_POINT('Ctrl Pts',(-65.2912910904982,-3.34667682289195,
-2.39783611777122));
#46158=CARTESIAN_POINT('Ctrl Pts',(-65.3520637842316,-3.93115608137005,
-1.19491648254071));
#46159=CARTESIAN_POINT('Ctrl Pts',(-65.412836477965,-3.93834804191526,0.00192586831589278));
#46160=CARTESIAN_POINT('Ctrl Pts',(-65.5961635220347,-3.93790589778391,
0.0022443990911959));
#46161=CARTESIAN_POINT('Ctrl Pts',(-65.5364676690782,-3.92990561084547,
-1.17373904290349));
#46162=CARTESIAN_POINT('Ctrl Pts',(-65.4767718161217,-3.36856921796084,
-2.356346824119));
#46163=CARTESIAN_POINT('Ctrl Pts',(-65.4170759631653,-2.44823933350512,
-3.08638734446033));
#46164=CARTESIAN_POINT('Ctrl Pts',(-65.3507847859328,-1.4262294540701,-3.89708428778295));
#46165=CARTESIAN_POINT('Ctrl Pts',(-65.2844936087003,0.0384806212853624,
-4.14968862006866));
#46166=CARTESIAN_POINT('Ctrl Pts',(-65.2182024314679,1.27300158021858,-3.72815365173264));
#46167=CARTESIAN_POINT('Ctrl Pts',(-65.1519112542354,2.50752253915183,-3.30661868339661));
#46168=CARTESIAN_POINT('Ctrl Pts',(-65.0856200770029,3.51185438166279,-2.21094441443874));
#46169=CARTESIAN_POINT('Ctrl Pts',(-65.0193288997704,3.82460602821833,-0.944484728877324));
#46170=CARTESIAN_POINT('Ctrl Pts',(-64.9530377225379,4.13735767477386,0.321974956684055));
#46171=CARTESIAN_POINT('Ctrl Pts',(-64.8867465453054,3.75852912537409,1.75922005884896));
#46172=CARTESIAN_POINT('Ctrl Pts',(-64.8204553680729,2.86215460453238,2.70697870215496));
#46173=CARTESIAN_POINT('Ctrl Pts',(-64.7541641908405,1.96578008369065,3.65473734546098));
#46174=CARTESIAN_POINT('Ctrl Pts',(-64.687873013608,0.551859591406997,4.113009529908));
#46175=CARTESIAN_POINT('Ctrl Pts',(-64.6215818363755,-0.730050346581443,
3.87126454348224));
#46176=CARTESIAN_POINT('Ctrl Pts',(-64.555290659143,-2.01196028456981,3.62951955705649));
#46177=CARTESIAN_POINT('Ctrl Pts',(-64.4889994819105,-3.16185966826298,
2.68775739975796));
#46178=CARTESIAN_POINT('Ctrl Pts',(-64.422708304678,-3.65148354026384,1.47862457349683));
#46179=CARTESIAN_POINT('Ctrl Pts',(-64.3971933771303,-3.83993573166107,
1.01323931793717));
#46180=CARTESIAN_POINT('Ctrl Pts',(-64.3716784495825,-3.93057361066039,
0.508245326816594));
#46181=CARTESIAN_POINT('Ctrl Pts',(-64.3461635220347,-3.92786728767746,
0.00231866363322961));
#46182=CARTESIAN_POINT('Origin',(-54.75,0.,0.));
#46183=CARTESIAN_POINT('',(-62.9128364779651,-3.92890725657977,-0.00290888419126417));
#46184=CARTESIAN_POINT('',(-63.0961635220347,-3.92941051997575,-0.00310996813596078));
#46185=CARTESIAN_POINT('',(-54.75,-3.933,-4.81653586104654E-16));
#46186=CARTESIAN_POINT('Ctrl Pts',(-62.9128364779651,-3.92890725657977,
-0.00290888419126417));
#46187=CARTESIAN_POINT('Ctrl Pts',(-62.9561941680077,-3.92304212850891,
0.85624490671229));
#46188=CARTESIAN_POINT('Ctrl Pts',(-62.9995518580503,-3.64598688522449,
1.71883987619063));
#46189=CARTESIAN_POINT('Ctrl Pts',(-63.0429095480929,-3.12704556945061,
2.39609029060797));
#46190=CARTESIAN_POINT('Ctrl Pts',(-63.1092007253254,-2.33361698265479,
3.43156351828243));
#46191=CARTESIAN_POINT('Ctrl Pts',(-63.1754919025578,-0.974743805821233,
4.03376634359936));
#46192=CARTESIAN_POINT('Ctrl Pts',(-63.2417830797903,0.325306228544258,
3.92604617036488));
#46193=CARTESIAN_POINT('Ctrl Pts',(-63.3080742570227,1.62535626290979,3.8183259971304));
#46194=CARTESIAN_POINT('Ctrl Pts',(-63.3743654342553,2.86658315480724,3.00068282534447));
#46195=CARTESIAN_POINT('Ctrl Pts',(-63.4406566114877,3.47876599581036,1.8487427675477));
#46196=CARTESIAN_POINT('Ctrl Pts',(-63.5069477887202,4.09094883681349,0.696802709750933));
#46197=CARTESIAN_POINT('Ctrl Pts',(-63.5732389659527,4.07408762692229,-0.789434234056675));
#46198=CARTESIAN_POINT('Ctrl Pts',(-63.6395301431852,3.4359284232711,-1.92718928606513));
#46199=CARTESIAN_POINT('Ctrl Pts',(-63.7058213204177,2.79776921961993,-3.06494433807355));
#46200=CARTESIAN_POINT('Ctrl Pts',(-63.7721124976502,1.53831202220882,-3.85421749828284));
#46201=CARTESIAN_POINT('Ctrl Pts',(-63.8384036748827,0.236152760532859,
-3.9324158665964));
#46202=CARTESIAN_POINT('Ctrl Pts',(-63.9046948521151,-1.06600650114314,
-4.01061423490997));
#46203=CARTESIAN_POINT('Ctrl Pts',(-63.9709860293476,-2.41086782708398,
-3.37773781132776));
#46204=CARTESIAN_POINT('Ctrl Pts',(-64.0372772065801,-3.18060054346902,
-2.32453067457735));
#46205=CARTESIAN_POINT('Ctrl Pts',(-64.0791302970417,-3.66657310203702,
-1.65958587483903));
#46206=CARTESIAN_POINT('Ctrl Pts',(-64.1209833875034,-3.9232960676761,-0.827094819727051));
#46207=CARTESIAN_POINT('Ctrl Pts',(-64.1628364779651,-3.92827063990554,
0.00258208764951584));
#46208=CARTESIAN_POINT('Ctrl Pts',(-64.3461635220347,-3.92786728767746,
0.00231866363322961));
#46209=CARTESIAN_POINT('Ctrl Pts',(-64.30538727235,-3.92354222339997,-0.806219471601042));
#46210=CARTESIAN_POINT('Ctrl Pts',(-64.2646110226653,-3.68081332915015,
-1.6171396786422));
#46211=CARTESIAN_POINT('Ctrl Pts',(-64.2238347729806,-3.21792615966099,
-2.27257869063668));
#46212=CARTESIAN_POINT('Ctrl Pts',(-64.1575435957481,-2.46539654674866,
-3.33814563328531));
#46213=CARTESIAN_POINT('Ctrl Pts',(-64.0912524185156,-1.13098896061534,
-3.99277602335871));
#46214=CARTESIAN_POINT('Ctrl Pts',(-64.0249612412831,0.172268383717981,
-3.93573198758981));
#46215=CARTESIAN_POINT('Ctrl Pts',(-63.9586700640506,1.47552572805126,-3.87868795182091));
#46216=CARTESIAN_POINT('Ctrl Pts',(-63.8923788868182,2.74763283058462,-3.10996949020974));
#46217=CARTESIAN_POINT('Ctrl Pts',(-63.8260877095857,3.40418238242286,-1.98272665321478));
#46218=CARTESIAN_POINT('Ctrl Pts',(-63.7597965323532,4.06073193426111,-0.855483816219792));
#46219=CARTESIAN_POINT('Ctrl Pts',(-63.6935053551207,4.10172393540427,0.630283396158968));
#46220=CARTESIAN_POINT('Ctrl Pts',(-63.6272141778882,3.50832661844329,1.79201200121225));
#46221=CARTESIAN_POINT('Ctrl Pts',(-63.5609230006557,2.91492930148232,2.9537406062655));
#46222=CARTESIAN_POINT('Ctrl Pts',(-63.4946318234233,1.6871426664172,3.79143060399324));
#46223=CARTESIAN_POINT('Ctrl Pts',(-63.4283406461908,0.3890131538872,3.92024634943637));
#46224=CARTESIAN_POINT('Ctrl Pts',(-63.3620494689583,-0.909116358642765,
4.04906209487949));
#46225=CARTESIAN_POINT('Ctrl Pts',(-63.2957582917257,-2.27758874863767,
3.46900358803805));
#46226=CARTESIAN_POINT('Ctrl Pts',(-63.2294671144933,-3.08772639521042,
2.44655030246413));
#46227=CARTESIAN_POINT('Ctrl Pts',(-63.1850325836737,-3.63075621799453,
1.76120673298667));
#46228=CARTESIAN_POINT('Ctrl Pts',(-63.1405980528542,-3.92293010133024,
0.877098248494651));
#46229=CARTESIAN_POINT('Ctrl Pts',(-63.0961635220347,-3.92941051997575,
-0.00310996813596078));
#46230=CARTESIAN_POINT('Origin',(-54.75,0.,0.));
#46231=CARTESIAN_POINT('',(-61.6628364779651,-3.93886391369501,-0.00144086038807723));
#46232=CARTESIAN_POINT('',(-61.8461635220346,-3.93914924332037,-0.00107030884100855));
#46233=CARTESIAN_POINT('',(-54.75,-3.933,-4.81653586104654E-16));
#46234=CARTESIAN_POINT('Ctrl Pts',(-61.6628364779651,-3.93886391369501,
-0.00144086038807723));
#46235=CARTESIAN_POINT('Ctrl Pts',(-61.7251137712794,-3.93310338294905,
1.22460701239503));
#46236=CARTESIAN_POINT('Ctrl Pts',(-61.7873910645938,-3.31531093334815,
2.45566105020782));
#46237=CARTESIAN_POINT('Ctrl Pts',(-61.8496683579081,-2.32627053840023,
3.17932823979179));
#46238=CARTESIAN_POINT('Ctrl Pts',(-61.9159595351406,-1.2734847055183,3.94963708542352));
#46239=CARTESIAN_POINT('Ctrl Pts',(-61.9822507123731,0.199946449501902,
4.14504738441835));
#46240=CARTESIAN_POINT('Ctrl Pts',(-62.0485418896056,1.41712714136624,3.67578744480276));
#46241=CARTESIAN_POINT('Ctrl Pts',(-62.1148330668381,2.63430783323069,3.20652750518713));
#46242=CARTESIAN_POINT('Ctrl Pts',(-62.1811242440705,3.59523806193922,2.07259732696095));
#46243=CARTESIAN_POINT('Ctrl Pts',(-62.247415421303,3.85846549389725,0.794925598135253));
#46244=CARTESIAN_POINT('Ctrl Pts',(-62.3137065985355,4.12169292585525,-0.482746130690301));
#46245=CARTESIAN_POINT('Ctrl Pts',(-62.379997775768,3.68721756106294,-1.90415941011534));
#46246=CARTESIAN_POINT('Ctrl Pts',(-62.4462889530005,2.75463782815404,-2.81631552029761));
#46247=CARTESIAN_POINT('Ctrl Pts',(-62.512580130233,1.82205809524509,-3.72847163047994));
#46248=CARTESIAN_POINT('Ctrl Pts',(-62.5788713074655,0.391373994219499,
-4.13137057141944));
#46249=CARTESIAN_POINT('Ctrl Pts',(-62.6451624846979,-0.880156730119362,
-3.83992015601784));
#46250=CARTESIAN_POINT('Ctrl Pts',(-62.7114536619304,-2.15168745445822,
-3.54846974061623));
#46251=CARTESIAN_POINT('Ctrl Pts',(-62.7777448391629,-3.26406480211035,
-2.56266996887352));
#46252=CARTESIAN_POINT('Ctrl Pts',(-62.8440360163953,-3.70626147755742,
-1.33539826798612));
#46253=CARTESIAN_POINT('Ctrl Pts',(-62.8669695035852,-3.8592397804802,-0.910822615450734));
#46254=CARTESIAN_POINT('Ctrl Pts',(-62.8899029907751,-3.93200953991977,
-0.457347126599487));
#46255=CARTESIAN_POINT('Ctrl Pts',(-62.9128364779651,-3.92890725657977,
-0.00290888419126417));
#46256=CARTESIAN_POINT('Ctrl Pts',(-63.0961635220347,-3.92941051997575,
-0.00310996813596078));
#46257=CARTESIAN_POINT('Ctrl Pts',(-63.0743068756218,-3.93259813592061,
-0.436070537446338));
#46258=CARTESIAN_POINT('Ctrl Pts',(-63.0524502292088,-3.86666218165736,
-0.86808743645036));
#46259=CARTESIAN_POINT('Ctrl Pts',(-63.0305935827959,-3.72745659244489,
-1.27504118584678));
#46260=CARTESIAN_POINT('Ctrl Pts',(-62.9643024055634,-3.30524623995596,
-2.50933132427722));
#46261=CARTESIAN_POINT('Ctrl Pts',(-62.8980112283309,-2.20902263182746,
-3.51306353683163));
#46262=CARTESIAN_POINT('Ctrl Pts',(-62.8317200510984,-0.942392019056605,
-3.82512221459457));
#46263=CARTESIAN_POINT('Ctrl Pts',(-62.7654288738659,0.324238593714291,
-4.13718089235752));
#46264=CARTESIAN_POINT('Ctrl Pts',(-62.6991376966334,1.76127621112752,-3.75756603532902));
#46265=CARTESIAN_POINT('Ctrl Pts',(-62.632846519401,2.70854427642858,-2.86067309855433));
#46266=CARTESIAN_POINT('Ctrl Pts',(-62.5665553421685,3.65581234172959,-1.96378016177969));
#46267=CARTESIAN_POINT('Ctrl Pts',(-62.500264164936,4.11331085491841,-0.54960914525888));
#46268=CARTESIAN_POINT('Ctrl Pts',(-62.4339729877035,3.87086452935152,0.732168334179135));
#46269=CARTESIAN_POINT('Ctrl Pts',(-62.367681810471,3.62841820378463,2.01394581361719));
#46270=CARTESIAN_POINT('Ctrl Pts',(-62.3013906332385,2.68602703946198,3.1633297559725));
#46271=CARTESIAN_POINT('Ctrl Pts',(-62.235099456006,1.47662650476639,3.65229199812773));
#46272=CARTESIAN_POINT('Ctrl Pts',(-62.1688082787735,0.267225970070802,
4.14125424028296));
#46273=CARTESIAN_POINT('Ctrl Pts',(-62.1025171015411,-1.20918393499766,
3.96979478223817));
#46274=CARTESIAN_POINT('Ctrl Pts',(-62.0362259243086,-2.27433898431471,
3.21668227504563));
#46275=CARTESIAN_POINT('Ctrl Pts',(-61.9728717902173,-3.2923021377792,2.49693655987786));
#46276=CARTESIAN_POINT('Ctrl Pts',(-61.9095176561259,-3.93464461114698,
1.24593653647341));
#46277=CARTESIAN_POINT('Ctrl Pts',(-61.8461635220346,-3.93914924332037,
-0.00107030884100855));
#46278=CARTESIAN_POINT('Origin',(-54.75,0.,0.));
#46279=CARTESIAN_POINT('',(-60.412836477965,-3.93331087711921,0.00361726591575254));
#46280=CARTESIAN_POINT('',(-60.5961635220347,-3.93266179433523,0.00363627036369697));
#46281=CARTESIAN_POINT('',(-54.75,-3.933,-4.81653586104654E-16));
#46282=CARTESIAN_POINT('Ctrl Pts',(-60.412836477965,-3.93331087711921,0.00361726591575254));
#46283=CARTESIAN_POINT('Ctrl Pts',(-60.4277421973187,-3.93604514286324,
0.298143623714554));
#46284=CARTESIAN_POINT('Ctrl Pts',(-60.4426479166723,-3.9057779826615,0.59211331334404));
#46285=CARTESIAN_POINT('Ctrl Pts',(-60.4575536360259,-3.84040114412618,
0.878055651061374));
#46286=CARTESIAN_POINT('Ctrl Pts',(-60.5238448132584,-3.54964646886187,
2.14974564724254));
#46287=CARTESIAN_POINT('Ctrl Pts',(-60.5901359904909,-2.56445546310868,
3.26266219205633));
#46288=CARTESIAN_POINT('Ctrl Pts',(-60.6564271677234,-1.3374258863424,3.70553028225484));
#46289=CARTESIAN_POINT('Ctrl Pts',(-60.7227183449559,-0.110396309576058,
4.14839837245339));
#46290=CARTESIAN_POINT('Ctrl Pts',(-60.7890095221883,1.35847183820337,3.92121800803657));
#46291=CARTESIAN_POINT('Ctrl Pts',(-60.8553006994208,2.39437902191271,3.12835608164908));
#46292=CARTESIAN_POINT('Ctrl Pts',(-60.9215918766533,3.43028620562202,2.33549415526161));
#46293=CARTESIAN_POINT('Ctrl Pts',(-60.9878830538858,4.03323242526126,0.976950666903413));
#46294=CARTESIAN_POINT('Ctrl Pts',(-61.0541742311183,3.92622356852165,-0.323158110143606));
#46295=CARTESIAN_POINT('Ctrl Pts',(-61.1204654083508,3.81921471178203,-1.62326688719066));
#46296=CARTESIAN_POINT('Ctrl Pts',(-61.1867565855833,3.00225077866358,-2.86494095292658));
#46297=CARTESIAN_POINT('Ctrl Pts',(-61.2530477628157,1.85064583876572,-3.47775396680466));
#46298=CARTESIAN_POINT('Ctrl Pts',(-61.3193389400482,0.699040898867858,
-4.09056698068275));
#46299=CARTESIAN_POINT('Ctrl Pts',(-61.3856301172807,-0.787205047809493,
-4.07451894270296));
#46300=CARTESIAN_POINT('Ctrl Pts',(-61.4519212945132,-1.92530908752859,
-3.4369823379887));
#46301=CARTESIAN_POINT('Ctrl Pts',(-61.5182124717457,-3.06341312724766,
-2.79944573327446));
#46302=CARTESIAN_POINT('Ctrl Pts',(-61.5845036489782,-3.85337526000851,
-1.54042056182595));
#46303=CARTESIAN_POINT('Ctrl Pts',(-61.6507948262107,-3.93228607101718,
-0.238304279967317));
#46304=CARTESIAN_POINT('Ctrl Pts',(-61.6548087101288,-3.93706406483925,
-0.159462059607168));
#46305=CARTESIAN_POINT('Ctrl Pts',(-61.6588225940469,-3.93923519029504,
-0.0804618578901768));
#46306=CARTESIAN_POINT('Ctrl Pts',(-61.6628364779651,-3.93886391369501,
-0.00144086038807723));
#46307=CARTESIAN_POINT('Ctrl Pts',(-61.8461635220346,-3.93914924332037,
-0.00107030884100855));
#46308=CARTESIAN_POINT('Ctrl Pts',(-61.8432264788935,-3.93935807419176,
-0.0588804731591042));
#46309=CARTESIAN_POINT('Ctrl Pts',(-61.8402894357523,-3.93819608322699,
-0.116682055459375));
#46310=CARTESIAN_POINT('Ctrl Pts',(-61.8373523926111,-3.9356371447697,-0.174421727073953));
#46311=CARTESIAN_POINT('Ctrl Pts',(-61.7710612153786,-3.87788006234203,
-1.47764766566053));
#46312=CARTESIAN_POINT('Ctrl Pts',(-61.7047700381462,-3.10846570392124,
-2.74933398649333));
#46313=CARTESIAN_POINT('Ctrl Pts',(-61.6384788609137,-1.98086381567448,
-3.40526668822253));
#46314=CARTESIAN_POINT('Ctrl Pts',(-61.5721876836812,-0.853261927427686,
-4.06119938995174));
#46315=CARTESIAN_POINT('Ctrl Pts',(-61.5058965064487,0.632527490645155,
-4.10137847257725));
#46316=CARTESIAN_POINT('Ctrl Pts',(-61.4396053292162,1.7939312545159,-3.5073456242916));
#46317=CARTESIAN_POINT('Ctrl Pts',(-61.3733141519837,2.95533501838662,-2.91331277600597));
#46318=CARTESIAN_POINT('Ctrl Pts',(-61.3070229747513,3.79235312805534,-1.68506799680926));
#46319=CARTESIAN_POINT('Ctrl Pts',(-61.2407317975188,3.92045860462712,-0.386868199225031));
#46320=CARTESIAN_POINT('Ctrl Pts',(-61.1744406202863,4.04856408119891,0.911331598359233));
#46321=CARTESIAN_POINT('Ctrl Pts',(-61.1081494430538,3.46775692467366,2.27948641433106));
#46322=CARTESIAN_POINT('Ctrl Pts',(-61.0418582658213,2.44486053903682,3.08906452163548));
#46323=CARTESIAN_POINT('Ctrl Pts',(-60.9755670885888,1.4219641534,3.89864262893988));
#46324=CARTESIAN_POINT('Ctrl Pts',(-60.9092759113564,-0.0430214613483292,
4.14964402757698));
#46325=CARTESIAN_POINT('Ctrl Pts',(-60.8429847341239,-1.27708040978551,
3.72675841732577));
#46326=CARTESIAN_POINT('Ctrl Pts',(-60.7766935568914,-2.51113935822273,
3.30387280707455));
#46327=CARTESIAN_POINT('Ctrl Pts',(-60.7104023796589,-3.51427164034871,
2.20710018793501));
#46328=CARTESIAN_POINT('Ctrl Pts',(-60.6441112024264,-3.82563725590282,
0.940299027126366));
#46329=CARTESIAN_POINT('Ctrl Pts',(-60.6281286422958,-3.90070636586495,
0.634877905170875));
#46330=CARTESIAN_POINT('Ctrl Pts',(-60.6121460821653,-3.93556484722619,
0.319573458575761));
#46331=CARTESIAN_POINT('Ctrl Pts',(-60.5961635220347,-3.93266179433523,
0.00363627036369697));
#46332=CARTESIAN_POINT('Origin',(-54.75,0.,0.));
#46333=CARTESIAN_POINT('',(-59.1628364779651,-3.92648948652695,-0.00022326326588662));
#46334=CARTESIAN_POINT('',(-59.3461635220347,-3.92655384726127,-0.000574964978985582));
#46335=CARTESIAN_POINT('',(-54.75,-3.933,-4.81653586104654E-16));
#46336=CARTESIAN_POINT('Ctrl Pts',(-59.1628364779651,-3.92648948652695,
-0.00022326326588662));
#46337=CARTESIAN_POINT('Ctrl Pts',(-59.1966618005905,-3.92615091508906,
0.671075478630216));
#46338=CARTESIAN_POINT('Ctrl Pts',(-59.2304871232159,-3.76302289449586,
1.34252854543093));
#46339=CARTESIAN_POINT('Ctrl Pts',(-59.2643124458412,-3.43803522382986,
1.92342831264168));
#46340=CARTESIAN_POINT('Ctrl Pts',(-59.3306036230737,-2.80112140890214,
3.06188099937473));
#46341=CARTESIAN_POINT('Ctrl Pts',(-59.3968948003062,-1.54252864031098,
3.85253186820853));
#46342=CARTESIAN_POINT('Ctrl Pts',(-59.4631859775387,-0.240455728064175,
3.93215509828994));
#46343=CARTESIAN_POINT('Ctrl Pts',(-59.5294771547712,1.06161718418263,4.01177832837136));
#46344=CARTESIAN_POINT('Ctrl Pts',(-59.5957683320036,2.40717024008509,3.3803739197004));
#46345=CARTESIAN_POINT('Ctrl Pts',(-59.6620595092361,3.17805498436802,2.32800970584318));
#46346=CARTESIAN_POINT('Ctrl Pts',(-59.7283506864686,3.94893972865099,1.2756454919859));
#46347=CARTESIAN_POINT('Ctrl Pts',(-59.7946418637011,4.14515616131437,-0.197678527057687));
#46348=CARTESIAN_POINT('Ctrl Pts',(-59.8609330409336,3.67656225174966,-1.41511578437099));
#46349=CARTESIAN_POINT('Ctrl Pts',(-59.9272242181661,3.207968342185,-2.63255304168415));
#46350=CARTESIAN_POINT('Ctrl Pts',(-59.9935153953985,2.07456409039245,-3.5941035372671));
#46351=CARTESIAN_POINT('Ctrl Pts',(-60.059806572631,0.797036573239359,-3.85802998628644));
#46352=CARTESIAN_POINT('Ctrl Pts',(-60.1260977498635,-0.480490943913802,
-4.12195643530578));
#46353=CARTESIAN_POINT('Ctrl Pts',(-60.1923889270961,-1.90214172642751,
-3.68825883776143));
#46354=CARTESIAN_POINT('Ctrl Pts',(-60.2586801043285,-2.81480794529668,
-2.75617831521495));
#46355=CARTESIAN_POINT('Ctrl Pts',(-60.3100655622074,-3.52225912515261,
-2.03367818125222));
#46356=CARTESIAN_POINT('Ctrl Pts',(-60.3614510200862,-3.92388486460105,
-1.01172264447929));
#46357=CARTESIAN_POINT('Ctrl Pts',(-60.412836477965,-3.93331087711921,0.00361726591575254));
#46358=CARTESIAN_POINT('Ctrl Pts',(-60.5961635220347,-3.93266179433523,
0.00363627036369697));
#46359=CARTESIAN_POINT('Ctrl Pts',(-60.5458549049328,-3.9235237979739,-0.990845395913261));
#46360=CARTESIAN_POINT('Ctrl Pts',(-60.4955462878309,-3.5402392935668,-1.99159635371037));
#46361=CARTESIAN_POINT('Ctrl Pts',(-60.445237670729,-2.85919073622048,-2.71010903988703));
#46362=CARTESIAN_POINT('Ctrl Pts',(-60.3789464934965,-1.96177965200193,
-3.65688624361394));
#46363=CARTESIAN_POINT('Ctrl Pts',(-60.312655316264,-0.547358534582749,
-4.11361094859019));
#46364=CARTESIAN_POINT('Ctrl Pts',(-60.2463641390315,0.734286102598856,
-3.87046335645961));
#46365=CARTESIAN_POINT('Ctrl Pts',(-60.180072961799,2.01593073978061,-3.62731576432901));
#46366=CARTESIAN_POINT('Ctrl Pts',(-60.1137817845665,3.16479889672468,-2.68429587509133));
#46367=CARTESIAN_POINT('Ctrl Pts',(-60.0474906073341,3.65309936266116,-1.47462799400088));
#46368=CARTESIAN_POINT('Ctrl Pts',(-59.9811994301016,4.14139982859761,-0.264960112910496));
#46369=CARTESIAN_POINT('Ctrl Pts',(-59.9149082528691,3.96913260352656,1.21135576003267));
#46370=CARTESIAN_POINT('Ctrl Pts',(-59.8486170756366,3.21543742750144,2.27609859715904));
#46371=CARTESIAN_POINT('Ctrl Pts',(-59.7823258984041,2.4617422514763,3.34084143428544));
#46372=CARTESIAN_POINT('Ctrl Pts',(-59.7160347211716,1.12661912449713,3.99401123559503));
#46373=CARTESIAN_POINT('Ctrl Pts',(-59.6497435439392,-0.176575018216088,
3.93554112379841));
#46374=CARTESIAN_POINT('Ctrl Pts',(-59.5834523667067,-1.47976916092926,
3.87707101200179));
#46375=CARTESIAN_POINT('Ctrl Pts',(-59.5171611894742,-2.75103431937646,
3.10696098709893));
#46376=CARTESIAN_POINT('Ctrl Pts',(-59.4508700122417,-3.40634997464003,
1.97900038515314));
#46377=CARTESIAN_POINT('Ctrl Pts',(-59.4159678488394,-3.75137226923431,
1.38513153436435));
#46378=CARTESIAN_POINT('Ctrl Pts',(-59.381065685437,-3.92565335922222,0.692066502269124));
#46379=CARTESIAN_POINT('Ctrl Pts',(-59.3461635220347,-3.92655384726127,
-0.000574964978985582));
#46380=CARTESIAN_POINT('Origin',(-54.75,0.,0.));
#46381=CARTESIAN_POINT('',(-57.9128364779651,-3.93413307819626,-0.00353956003321609));
#46382=CARTESIAN_POINT('',(-58.0961635220347,-3.93477881256964,-0.00343548079462405));
#46383=CARTESIAN_POINT('',(-54.75,-3.933,-4.81653586104654E-16));
#46384=CARTESIAN_POINT('Ctrl Pts',(-57.9128364779651,-3.93413307819626,
-0.00353956003321609));
#46385=CARTESIAN_POINT('Ctrl Pts',(-57.9655814038622,-3.92446652853235,
1.03810397902358));
#46386=CARTESIAN_POINT('Ctrl Pts',(-58.0183263297594,-3.49893535502753,
2.08672616861535));
#46387=CARTESIAN_POINT('Ctrl Pts',(-58.0710712556565,-2.7577179772013,2.81329952766982));
#46388=CARTESIAN_POINT('Ctrl Pts',(-58.137362432889,-1.82613694403996,3.72647558201504));
#46389=CARTESIAN_POINT('Ctrl Pts',(-58.2036536101215,-0.395894578184176,
4.13093983068094));
#46390=CARTESIAN_POINT('Ctrl Pts',(-58.269944787354,0.875954309153151,3.84088098259272));
#46391=CARTESIAN_POINT('Ctrl Pts',(-58.3362359645864,2.14780319649048,3.55082213450451));
#46392=CARTESIAN_POINT('Ctrl Pts',(-58.4025271418189,3.26125860530939,2.56624018966217));
#46393=CARTESIAN_POINT('Ctrl Pts',(-58.4688183190514,3.70479797768473,1.33945310433386));
#46394=CARTESIAN_POINT('Ctrl Pts',(-58.5351094962839,4.14833735006006,0.11266601900554));
#46395=CARTESIAN_POINT('Ctrl Pts',(-58.6014006735164,3.92196068599184,-1.35632620680879));
#46396=CARTESIAN_POINT('Ctrl Pts',(-58.6676918507489,3.12966565735949,-2.39266703644929));
#46397=CARTESIAN_POINT('Ctrl Pts',(-58.7339830279814,2.33737062872715,-3.42900786608978));
#46398=CARTESIAN_POINT('Ctrl Pts',(-58.8002742052139,0.979157235530679,
-4.03269729955644));
#46399=CARTESIAN_POINT('Ctrl Pts',(-58.8665653824463,-0.321009895004302,
-3.92639979134522));
#46400=CARTESIAN_POINT('Ctrl Pts',(-58.9328565596788,-1.62117702553925,
-3.82010228313399));
#46401=CARTESIAN_POINT('Ctrl Pts',(-58.9991477369113,-2.86329789341262,
-3.00381783324499));
#46402=CARTESIAN_POINT('Ctrl Pts',(-59.0654389141437,-3.47674089671723,
-1.85254835598435));
#46403=CARTESIAN_POINT('Ctrl Pts',(-59.0979047687509,-3.77717229930323,
-1.28871846152857));
#46404=CARTESIAN_POINT('Ctrl Pts',(-59.130370623358,-3.92681445049547,-0.644541947043256));
#46405=CARTESIAN_POINT('Ctrl Pts',(-59.1628364779651,-3.92648948652695,
-0.00022326326588662));
#46406=CARTESIAN_POINT('Ctrl Pts',(-59.3461635220347,-3.92655384726127,
-0.000574964978985582));
#46407=CARTESIAN_POINT('Ctrl Pts',(-59.3147745082045,-3.927363694811,-0.623497170235501));
#46408=CARTESIAN_POINT('Ctrl Pts',(-59.2833854943744,-3.78794024227485,
-1.24607678874562));
#46409=CARTESIAN_POINT('Ctrl Pts',(-59.2519964805442,-3.50636358019973,
-1.79584997079805));
#46410=CARTESIAN_POINT('Ctrl Pts',(-59.1857053033117,-2.9116953784159,-2.9569285458146));
#46411=CARTESIAN_POINT('Ctrl Pts',(-59.1194141260793,-1.68299282276828,
-3.79327451685904));
#46412=CARTESIAN_POINT('Ctrl Pts',(-59.0531229488468,-0.384723128751967,
-3.92066968621047));
#46413=CARTESIAN_POINT('Ctrl Pts',(-58.9868317716143,0.913546565264345,
-4.0480648555619));
#46414=CARTESIAN_POINT('Ctrl Pts',(-58.9205405943818,2.28138339764935,-3.46650922322033));
#46415=CARTESIAN_POINT('Ctrl Pts',(-58.8542494171493,3.09040172333452,-2.44317004372955));
#46416=CARTESIAN_POINT('Ctrl Pts',(-58.7879582399168,3.89942004901979,-1.41983086423867));
#46417=CARTESIAN_POINT('Ctrl Pts',(-58.7216670626844,4.14961986800506,0.0452918624015372));
#46418=CARTESIAN_POINT('Ctrl Pts',(-58.6553758854519,3.7260591265843,1.27911925142432));
#46419=CARTESIAN_POINT('Ctrl Pts',(-58.5890847082194,3.30249838516356,2.51294664044703));
#46420=CARTESIAN_POINT('Ctrl Pts',(-58.5227935309869,2.20517708333687,3.51547869185234));
#46421=CARTESIAN_POINT('Ctrl Pts',(-58.4565023537544,0.938205753713269,
3.82615115198887));
#46422=CARTESIAN_POINT('Ctrl Pts',(-58.3902111765219,-0.328765575910331,
4.1368236121254));
#46423=CARTESIAN_POINT('Ctrl Pts',(-58.3239199992895,-1.76538693333084,
3.75563648099315));
#46424=CARTESIAN_POINT('Ctrl Pts',(-58.257628822057,-2.71167299206166,2.85770751797482));
#46425=CARTESIAN_POINT('Ctrl Pts',(-58.2038070553829,-3.47996207043064,
2.12867953634796));
#46426=CARTESIAN_POINT('Ctrl Pts',(-58.1499852887088,-3.92503161905221,
1.05902534985808));
#46427=CARTESIAN_POINT('Ctrl Pts',(-58.0961635220347,-3.93477881256964,
-0.00343548079462405));
#46428=CARTESIAN_POINT('Origin',(-54.75,0.,0.));
#46429=CARTESIAN_POINT('',(-56.6628364779651,-3.93840323605561,0.00188100101654563));
#46430=CARTESIAN_POINT('',(-56.8461635220347,-3.93796868589441,0.00220300913379331));
#46431=CARTESIAN_POINT('',(-54.75,-3.933,-4.81653586104654E-16));
#46432=CARTESIAN_POINT('Ctrl Pts',(-56.6628364779651,-3.93840323605561,
0.00188100101654563));
#46433=CARTESIAN_POINT('Ctrl Pts',(-56.6682098299015,-3.93902682028425,
0.107698540420122));
#46434=CARTESIAN_POINT('Ctrl Pts',(-56.6735831818379,-3.93513331440954,
0.213469473948844));
#46435=CARTESIAN_POINT('Ctrl Pts',(-56.6789565337743,-3.9265748387829,0.318861583768759));
#46436=CARTESIAN_POINT('Ctrl Pts',(-56.7452477110068,-3.82098871092086,
1.61908667858072));
#46437=CARTESIAN_POINT('Ctrl Pts',(-56.8115388882393,-3.00538398861963,
2.86165397675729));
#46438=CARTESIAN_POINT('Ctrl Pts',(-56.8778300654718,-1.85445031863387,
3.47572678585144));
#46439=CARTESIAN_POINT('Ctrl Pts',(-56.9441212427042,-0.703516648648172,
4.08979959494555));
#46440=CARTESIAN_POINT('Ctrl Pts',(-57.0104124199367,0.782745969022029,
4.0753779149573));
#46441=CARTESIAN_POINT('Ctrl Pts',(-57.0767035971692,1.92154696196791,3.43908708047911));
#46442=CARTESIAN_POINT('Ctrl Pts',(-57.1429947744017,3.06034795491373,2.80279624600096));
#46443=CARTESIAN_POINT('Ctrl Pts',(-57.2092859516342,3.85168732313528,1.54463625703294));
#46444=CARTESIAN_POINT('Ctrl Pts',(-57.2755771288667,3.93202294845389,0.242607104179611));
#46445=CARTESIAN_POINT('Ctrl Pts',(-57.3418683060992,4.01235857377251,-1.05942204867379));
#46446=CARTESIAN_POINT('Ctrl Pts',(-57.4081594833316,3.38169045618811,-2.40532036541251));
#46447=CARTESIAN_POINT('Ctrl Pts',(-57.4744506605641,2.32974817638575,-3.17678077757873));
#46448=CARTESIAN_POINT('Ctrl Pts',(-57.5407418377966,1.27780589658338,-3.94824118974495));
#46449=CARTESIAN_POINT('Ctrl Pts',(-57.6070330150291,-0.195410545436957,
-4.14526369733868));
#46450=CARTESIAN_POINT('Ctrl Pts',(-57.6733241922616,-1.41310400375366,
-3.6773359581009));
#46451=CARTESIAN_POINT('Ctrl Pts',(-57.7396153694941,-2.63079746207036,
-3.20940821886311));
#46452=CARTESIAN_POINT('Ctrl Pts',(-57.8059065467266,-3.59296793668343,
-2.07653023279381));
#46453=CARTESIAN_POINT('Ctrl Pts',(-57.872197723959,-3.85759332375651,-0.799147309746884));
#46454=CARTESIAN_POINT('Ctrl Pts',(-57.8857439752944,-3.91166812152987,
-0.53812086777579));
#46455=CARTESIAN_POINT('Ctrl Pts',(-57.8992902266297,-3.93661569636409,
-0.271060367805669));
#46456=CARTESIAN_POINT('Ctrl Pts',(-57.9128364779651,-3.93413307819626,
-0.00353956003321609));
#46457=CARTESIAN_POINT('Ctrl Pts',(-58.0961635220347,-3.93477881256964,
-0.00343548079462405));
#46458=CARTESIAN_POINT('Ctrl Pts',(-58.0836941114763,-3.93703703940372,
-0.249586083391217));
#46459=CARTESIAN_POINT('Ctrl Pts',(-58.0712247009179,-3.91592912913868,
-0.495350579148307));
#46460=CARTESIAN_POINT('Ctrl Pts',(-58.0587552903595,-3.87006102492655,
-0.736403651206962));
#46461=CARTESIAN_POINT('Ctrl Pts',(-57.992464113127,-3.62621223901949,-2.017915062466));
#46462=CARTESIAN_POINT('Ctrl Pts',(-57.9261729358945,-2.68256390716426,
-3.16626709007967));
#46463=CARTESIAN_POINT('Ctrl Pts',(-57.8598817586621,-1.47262904179876,
-3.65390563362237));
#46464=CARTESIAN_POINT('Ctrl Pts',(-57.7935905814296,-0.262694176433262,
-4.14154417716508));
#46465=CARTESIAN_POINT('Ctrl Pts',(-57.7272994041971,1.2135272224425,-3.96846923663683));
#46466=CARTESIAN_POINT('Ctrl Pts',(-57.6610082269646,2.27785752864255,-3.21419161740132));
#46467=CARTESIAN_POINT('Ctrl Pts',(-57.5947170497321,3.3421878348426,-2.45991399816581));
#46468=CARTESIAN_POINT('Ctrl Pts',(-57.5284258724996,3.99462704836693,-1.12443370022303));
#46469=CARTESIAN_POINT('Ctrl Pts',(-57.4621346952671,3.93544392470469,0.178728256499565));
#46470=CARTESIAN_POINT('Ctrl Pts',(-57.3958435180347,3.87626080104246,1.48189021322216));
#46471=CARTESIAN_POINT('Ctrl Pts',(-57.3295523408022,3.10545534019366,2.75273382872457));
#46472=CARTESIAN_POINT('Ctrl Pts',(-57.2632611635697,1.97713636220909,3.40743224135082));
#46473=CARTESIAN_POINT('Ctrl Pts',(-57.1969699863372,0.848817384224515,
4.06213065397707));
#46474=CARTESIAN_POINT('Ctrl Pts',(-57.1306788091047,-0.637015110895826,
4.10068386372716));
#46475=CARTESIAN_POINT('Ctrl Pts',(-57.0643876318722,-1.7977681494841,3.50538048646177));
#46476=CARTESIAN_POINT('Ctrl Pts',(-56.9980964546397,-2.95852118807237,
2.91007710919639));
#46477=CARTESIAN_POINT('Ctrl Pts',(-56.9318052774073,-3.79419477012857,
1.68091714491552));
#46478=CARTESIAN_POINT('Ctrl Pts',(-56.8655141001748,-3.92087959412325,
0.382577943110031));
#46479=CARTESIAN_POINT('Ctrl Pts',(-56.8590639074614,-3.93320614439339,
0.256248340762304));
#46480=CARTESIAN_POINT('Ctrl Pts',(-56.8526137147481,-3.93882036517576,
0.12926378608889));
#46481=CARTESIAN_POINT('Ctrl Pts',(-56.8461635220347,-3.93796868589441,
0.00220300913379331));
#46482=CARTESIAN_POINT('Origin',(-54.75,0.,0.));
#46483=CARTESIAN_POINT('',(-55.4128364779651,-3.92832844003735,0.00261578722564659));
#46484=CARTESIAN_POINT('',(-55.5961635220347,-3.92791896985871,0.00235549104295047));
#46485=CARTESIAN_POINT('',(-54.75,-3.933,-4.81653586104654E-16));
#46486=CARTESIAN_POINT('Ctrl Pts',(-55.4128364779651,-3.92832844003735,
0.00261578722564659));
#46487=CARTESIAN_POINT('Ctrl Pts',(-55.4371294331733,-3.93125619142034,
0.484170671996506));
#46488=CARTESIAN_POINT('Ctrl Pts',(-55.4614223883815,-3.84934041430319,
0.964764115204058));
#46489=CARTESIAN_POINT('Ctrl Pts',(-55.4857153435896,-3.67810856362453,
1.41109180011732));
#46490=CARTESIAN_POINT('Ctrl Pts',(-55.5520065208221,-3.21084713478989,
2.6290410949153));
#46491=CARTESIAN_POINT('Ctrl Pts',(-55.6182976980545,-2.07849575357617,
3.59183126052822));
#46492=CARTESIAN_POINT('Ctrl Pts',(-55.684588875287,-0.801257807025967,
3.85715550643818));
#46493=CARTESIAN_POINT('Ctrl Pts',(-55.7508800525195,0.475980139524241,
4.12247975234815));
#46494=CARTESIAN_POINT('Ctrl Pts',(-55.817171229752,1.89810465141093,3.69033807855515));
#46495=CARTESIAN_POINT('Ctrl Pts',(-55.8834624069845,2.81179026786874,2.75925681365202));
#46496=CARTESIAN_POINT('Ctrl Pts',(-55.949753584217,3.72547588432654,1.82817554874889));
#46497=CARTESIAN_POINT('Ctrl Pts',(-56.0160447614495,4.13072260535545,0.398154692735642));
#46498=CARTESIAN_POINT('Ctrl Pts',(-56.082335938682,3.8413596712738,-0.873852705023954));
#46499=CARTESIAN_POINT('Ctrl Pts',(-56.1486271159144,3.55199673719215,-2.14586010278355));
#46500=CARTESIAN_POINT('Ctrl Pts',(-56.2149182931469,2.56802414799994,-3.25985404228949));
#46501=CARTESIAN_POINT('Ctrl Pts',(-56.2812094703794,1.34147992135404,-3.70406456406613));
#46502=CARTESIAN_POINT('Ctrl Pts',(-56.3475006476119,0.114935694708133,
-4.14827508584278));
#46503=CARTESIAN_POINT('Ctrl Pts',(-56.4137918248444,-1.35418016939147,
-3.92270218989013));
#46504=CARTESIAN_POINT('Ctrl Pts',(-56.4800830020769,-2.39095433472975,
-3.13097429619016));
#46505=CARTESIAN_POINT('Ctrl Pts',(-56.541000827373,-3.34369088448296,-2.4034213468543));
#46506=CARTESIAN_POINT('Ctrl Pts',(-56.601918652669,-3.93133364605914,-1.19777508980574));
#46507=CARTESIAN_POINT('Ctrl Pts',(-56.6628364779651,-3.93840323605561,
0.00188100101654563));
#46508=CARTESIAN_POINT('Ctrl Pts',(-56.8461635220347,-3.93796868589441,
0.00220300913379331));
#46509=CARTESIAN_POINT('Ctrl Pts',(-56.7863225375156,-3.93006732093442,
-1.17658998584482));
#46510=CARTESIAN_POINT('Ctrl Pts',(-56.7264815529964,-3.36564558318113,
-2.36194343678467));
#46511=CARTESIAN_POINT('Ctrl Pts',(-56.6666405684773,-2.44147881704743,
-3.091737999908));
#46512=CARTESIAN_POINT('Ctrl Pts',(-56.6003493912448,-1.4176971500438,-3.90019630179039));
#46513=CARTESIAN_POINT('Ctrl Pts',(-56.5340582140124,0.0475622498966481,
-4.14959446622516));
#46514=CARTESIAN_POINT('Ctrl Pts',(-56.4677670367799,1.28115771015286,-3.72535872042979));
#46515=CARTESIAN_POINT('Ctrl Pts',(-56.4014758595474,2.51475317040914,-3.3011229746344));
#46516=CARTESIAN_POINT('Ctrl Pts',(-56.3351846823149,3.51668469098117,-2.20325331860879));
#46517=CARTESIAN_POINT('Ctrl Pts',(-56.2688935050824,3.82666390269889,-0.936112199443943));
#46518=CARTESIAN_POINT('Ctrl Pts',(-56.2026023278499,4.13664311441661,0.331028919720903));
#46519=CARTESIAN_POINT('Ctrl Pts',(-56.1363111506175,3.75467001728003,1.76744150202498));
#46520=CARTESIAN_POINT('Ctrl Pts',(-56.070019973385,2.85622344426113,2.71323613248452));
#46521=CARTESIAN_POINT('Ctrl Pts',(-56.0037287961525,1.95777687124224,3.65903076294405));
#46522=CARTESIAN_POINT('Ctrl Pts',(-55.93743761892,0.542856822341028,4.11420744155904));
#46523=CARTESIAN_POINT('Ctrl Pts',(-55.8711464416875,-0.738520979369014,
3.86965753487286));
#46524=CARTESIAN_POINT('Ctrl Pts',(-55.804855264455,-2.01989878107906,3.62510762818668));
#46525=CARTESIAN_POINT('Ctrl Pts',(-55.7385640872225,-3.16773433559793,
2.68083113619934));
#46526=CARTESIAN_POINT('Ctrl Pts',(-55.67227290999,-3.65471081077004,1.47062964875833));
#46527=CARTESIAN_POINT('Ctrl Pts',(-55.6469031140049,-3.84107790124023,
1.00748257370225));
#46528=CARTESIAN_POINT('Ctrl Pts',(-55.6215333180198,-3.93065480055029,
0.50538781380894));
#46529=CARTESIAN_POINT('Ctrl Pts',(-55.5961635220347,-3.92791896985871,
0.00235549104295047));
#46530=CARTESIAN_POINT('Origin',(-54.75,0.,0.));
#46531=CARTESIAN_POINT('',(-54.1628364779651,-3.92884235167783,-0.00287961617827709));
#46532=CARTESIAN_POINT('',(-54.3461635220347,-3.92934053852407,-0.00308456158941818));
#46533=CARTESIAN_POINT('',(-54.75,-3.933,-4.81653586104654E-16));
#46534=CARTESIAN_POINT('Ctrl Pts',(-54.1628364779651,-3.92884235167783,
-0.00287961617827709));
#46535=CARTESIAN_POINT('Ctrl Pts',(-54.206049036445,-3.92306180087508,0.853433875710847));
#46536=CARTESIAN_POINT('Ctrl Pts',(-54.249261594925,-3.64800779627708,1.71312716798816));
#46537=CARTESIAN_POINT('Ctrl Pts',(-54.2924741534049,-3.1322819977492,2.38924091726697));
#46538=CARTESIAN_POINT('Ctrl Pts',(-54.3587653306374,-2.34112147598905,
3.42644810793985));
#46539=CARTESIAN_POINT('Ctrl Pts',(-54.4250565078698,-0.983569492779588,
4.03162342668745));
#46540=CARTESIAN_POINT('Ctrl Pts',(-54.4913476851023,0.316713177080749,
3.92674871078222));
#46541=CARTESIAN_POINT('Ctrl Pts',(-54.5576388623348,1.61699584694123,3.82187399487699));
#46542=CARTESIAN_POINT('Ctrl Pts',(-54.6239300395673,2.8600092034525,3.00694924431876));
#46543=CARTESIAN_POINT('Ctrl Pts',(-54.6902212167998,3.47471163451067,1.85635172614531));
#46544=CARTESIAN_POINT('Ctrl Pts',(-54.7565123940323,4.08941406556879,0.705754207971926));
#46545=CARTESIAN_POINT('Ctrl Pts',(-54.8228035712648,4.07580557117382,-0.780516077816789));
#46546=CARTESIAN_POINT('Ctrl Pts',(-54.8890947484972,3.44013790762175,-1.91966503607018));
#46547=CARTESIAN_POINT('Ctrl Pts',(-54.9553859257297,2.80447024406971,-3.0588139943235));
#46548=CARTESIAN_POINT('Ctrl Pts',(-55.0216771029623,1.54674341136077,-3.8508416250417));
#46549=CARTESIAN_POINT('Ctrl Pts',(-55.0879682801947,0.24475840766927,-3.93188962154861));
#46550=CARTESIAN_POINT('Ctrl Pts',(-55.1542594574272,-1.05722659602223,
-4.01293761805551));
#46551=CARTESIAN_POINT('Ctrl Pts',(-55.2205506346596,-2.4034697706962,-3.3830059803511));
#46552=CARTESIAN_POINT('Ctrl Pts',(-55.2868418118921,-3.17550561980544,
-2.33148594950742));
#46553=CARTESIAN_POINT('Ctrl Pts',(-55.3288400339164,-3.66462248807148,
-1.6653042106689));
#46554=CARTESIAN_POINT('Ctrl Pts',(-55.3708382559408,-3.92326687582826,
-0.829907419366287));
#46555=CARTESIAN_POINT('Ctrl Pts',(-55.4128364779651,-3.92832844003735,
0.00261578722564659));
#46556=CARTESIAN_POINT('Ctrl Pts',(-55.5961635220347,-3.92791896985871,
0.00235549104295047));
#46557=CARTESIAN_POINT('Ctrl Pts',(-55.5552421407873,-3.92350608570213,
-0.809033669191091));
#46558=CARTESIAN_POINT('Ctrl Pts',(-55.51432075954,-3.67891797236441,-1.62286213955943));
#46559=CARTESIAN_POINT('Ctrl Pts',(-55.4733993782926,-3.21294484511795,
-2.27961577823905));
#46560=CARTESIAN_POINT('Ctrl Pts',(-55.4071082010601,-2.45808500846852,
-3.34353323490047));
#46561=CARTESIAN_POINT('Ctrl Pts',(-55.3408170238277,-1.12224793934446,
-3.99524166532875));
#46562=CARTESIAN_POINT('Ctrl Pts',(-55.2745258465952,0.180881441279908,
-3.93534554751764));
#46563=CARTESIAN_POINT('Ctrl Pts',(-55.2082346693627,1.48401082190435,-3.87544942970653));
#46564=CARTESIAN_POINT('Ctrl Pts',(-55.1419434921302,2.75443251402909,-3.10394876365596));
#46565=CARTESIAN_POINT('Ctrl Pts',(-55.0756523148977,3.40851348803101,-1.97527174740012));
#46566=CARTESIAN_POINT('Ctrl Pts',(-55.0093611376652,4.06259446203293,-0.846594731144286));
#46567=CARTESIAN_POINT('Ctrl Pts',(-54.9430699604327,4.10033471791204,0.639258635316805));
#46568=CARTESIAN_POINT('Ctrl Pts',(-54.8767787832002,3.50439634337196,1.79968578999994));
#46569=CARTESIAN_POINT('Ctrl Pts',(-54.8104876059678,2.90845796883184,2.96011294468314));
#46570=CARTESIAN_POINT('Ctrl Pts',(-54.7441964287352,1.67884096387245,3.79511388758835));
#46571=CARTESIAN_POINT('Ctrl Pts',(-54.6779052515028,0.380432642941623,
3.9210883283026));
#46572=CARTESIAN_POINT('Ctrl Pts',(-54.6116140742703,-0.917975677989054,
4.04706276901683));
#46573=CARTESIAN_POINT('Ctrl Pts',(-54.5453228970378,-2.28517531489115,
3.4640107075403));
#46574=CARTESIAN_POINT('Ctrl Pts',(-54.4790317198053,-3.09307335095514,
2.43978685949768));
#46575=CARTESIAN_POINT('Ctrl Pts',(-54.4347423205485,-3.63283324317415,
1.75549883161612));
#46576=CARTESIAN_POINT('Ctrl Pts',(-54.3904529212916,-3.92294163618298,
0.874288074100991));
#46577=CARTESIAN_POINT('Ctrl Pts',(-54.3461635220347,-3.92934053852407,
-0.00308456158941818));
#46578=CARTESIAN_POINT('Origin',(-54.75,0.,0.));
#46579=CARTESIAN_POINT('',(-52.9128364779651,-3.93881984523232,-0.00148943800153567));
#46580=CARTESIAN_POINT('',(-53.0961635220347,-3.93911522694479,-0.00112120486990875));
#46581=CARTESIAN_POINT('',(-54.75,-3.933,-4.81653586104654E-16));
#46582=CARTESIAN_POINT('Ctrl Pts',(-52.9128364779651,-3.93881984523232,
-0.00148943800153567));
#46583=CARTESIAN_POINT('Ctrl Pts',(-52.9749686397168,-3.93290517754326,
1.22173761791364));
#46584=CARTESIAN_POINT('Ctrl Pts',(-53.0371008014685,-3.31837611095895,
2.45009099042727));
#46585=CARTESIAN_POINT('Ctrl Pts',(-53.0992329632202,-2.33322302468783,
3.17422951142998));
#46586=CARTESIAN_POINT('Ctrl Pts',(-53.1655241404527,-1.28212555758009,
3.94684056636974));
#46587=CARTESIAN_POINT('Ctrl Pts',(-53.2318153176851,0.190874407383879,
4.14547504664396));
#46588=CARTESIAN_POINT('Ctrl Pts',(-53.2981064949176,1.40907917406434,3.67888006808928));
#46589=CARTESIAN_POINT('Ctrl Pts',(-53.3643976721501,2.62728394074473,3.21228508953463));
#46590=CARTESIAN_POINT('Ctrl Pts',(-53.4306888493826,3.59069350914173,2.08046065215113));
#46591=CARTESIAN_POINT('Ctrl Pts',(-53.496980026615,3.85671653446252,0.803368064444818));
#46592=CARTESIAN_POINT('Ctrl Pts',(-53.5632712038475,4.12273955978333,-0.473724523261566));
#46593=CARTESIAN_POINT('Ctrl Pts',(-53.62956238108,3.69137604202797,-1.89608526129067));
#46594=CARTESIAN_POINT('Ctrl Pts',(-53.6958535583125,2.76079482410662,-2.81028016634508));
#46595=CARTESIAN_POINT('Ctrl Pts',(-53.762144735545,1.83021360618522,-3.72447507139954));
#46596=CARTESIAN_POINT('Ctrl Pts',(-53.8284359127775,0.400414688097706,
-4.13050414347906));
#46597=CARTESIAN_POINT('Ctrl Pts',(-53.89472709001,-0.871750839302914,-3.8418372100261));
#46598=CARTESIAN_POINT('Ctrl Pts',(-53.9610182672425,-2.14391636670339,
-3.55317027657317));
#46599=CARTESIAN_POINT('Ctrl Pts',(-54.0273094444749,-3.25844850341708,
-2.5698073375879));
#46600=CARTESIAN_POINT('Ctrl Pts',(-54.0936006217074,-3.70333004161861,
-1.34350633679621));
#46601=CARTESIAN_POINT('Ctrl Pts',(-54.11667924046,-3.85821115610231,-0.916581752640813));
#46602=CARTESIAN_POINT('Ctrl Pts',(-54.1397578592125,-3.93192958216936,
-0.460212699595579));
#46603=CARTESIAN_POINT('Ctrl Pts',(-54.1628364779651,-3.92884235167783,
-0.00287961617827709));
#46604=CARTESIAN_POINT('Ctrl Pts',(-54.3461635220347,-3.92934053852407,
-0.00308456158941818));
#46605=CARTESIAN_POINT('Ctrl Pts',(-54.3241617440591,-3.93251934047123,
-0.438939602665642));
#46606=CARTESIAN_POINT('Ctrl Pts',(-54.3021599660835,-3.86568334434236,
-0.873847458915858));
#46607=CARTESIAN_POINT('Ctrl Pts',(-54.2801581881079,-3.72465719907194,
-1.28319578536092));
#46608=CARTESIAN_POINT('Ctrl Pts',(-54.2138670108754,-3.29974657589884,
-2.51655894756822));
#46609=CARTESIAN_POINT('Ctrl Pts',(-54.147575833643,-2.20132889432679,-3.51788963737405));
#46610=CARTESIAN_POINT('Ctrl Pts',(-54.0812846564105,-0.934018364945315,
-3.82717550787932));
#46611=CARTESIAN_POINT('Ctrl Pts',(-54.014993479178,0.333292164436233,-4.13646137838461));
#46612=CARTESIAN_POINT('Ctrl Pts',(-53.9487023019454,1.76949554162732,-3.75370242958909));
#46613=CARTESIAN_POINT('Ctrl Pts',(-53.8824111247129,2.71479846068759,-2.85473851552375));
#46614=CARTESIAN_POINT('Ctrl Pts',(-53.8161199474805,3.66010137974786,-1.95577460145841));
#46615=CARTESIAN_POINT('Ctrl Pts',(-53.749828770248,4.11450384067746,-0.540605722123302));
#46616=CARTESIAN_POINT('Ctrl Pts',(-53.6835375930156,3.8692528864193,0.740638086451396));
#46617=CARTESIAN_POINT('Ctrl Pts',(-53.6172464157831,3.62400193216114,2.02188189502609));
#46618=CARTESIAN_POINT('Ctrl Pts',(-53.5509552385505,2.67909756271524,3.16920063284027));
#46619=CARTESIAN_POINT('Ctrl Pts',(-53.484664061318,1.46862981547812,3.65551489386313));
#46620=CARTESIAN_POINT('Ctrl Pts',(-53.4183728840855,0.258162068241059,
4.14182915488595));
#46621=CARTESIAN_POINT('Ctrl Pts',(-53.3520817068531,-1.21786905678733,
3.96713893911743));
#46622=CARTESIAN_POINT('Ctrl Pts',(-53.2857905296207,-2.28137334542168,
3.21169711102494));
#46623=CARTESIAN_POINT('Ctrl Pts',(-53.222581527092,-3.29543054090254,2.49137916804033));
#46624=CARTESIAN_POINT('Ctrl Pts',(-53.1593725245633,-3.93442957764801,
1.24305768398959));
#46625=CARTESIAN_POINT('Ctrl Pts',(-53.0961635220347,-3.93911522694479,
-0.00112120486990875));
#46626=CARTESIAN_POINT('Origin',(-54.75,0.,0.));
#46627=CARTESIAN_POINT('',(-51.6628364779651,-3.93339868146552,0.0036118335011201));
#46628=CARTESIAN_POINT('',(-51.8461635220348,-3.93274891143005,0.00363589115318885));
#46629=CARTESIAN_POINT('',(-54.75,-3.933,-4.81653586104654E-16));
#46630=CARTESIAN_POINT('Ctrl Pts',(-51.6628364779651,-3.93339868146552,
0.0036118335011201));
#46631=CARTESIAN_POINT('Ctrl Pts',(-51.677597065756,-3.93610801214239,0.295253828418355));
#46632=CARTESIAN_POINT('Ctrl Pts',(-51.692357653547,-3.90643403127602,0.586349483354395));
#46633=CARTESIAN_POINT('Ctrl Pts',(-51.707118241338,-3.84231359870667,0.869648712619224));
#46634=CARTESIAN_POINT('Ctrl Pts',(-51.7734094185705,-3.5543427522962,2.14197198883212));
#46635=CARTESIAN_POINT('Ctrl Pts',(-51.8397005958029,-2.57158975789195,
3.2570419891133));
#46636=CARTESIAN_POINT('Ctrl Pts',(-51.9059917730354,-1.34553235005313,
3.70259441056227));
#46637=CARTESIAN_POINT('Ctrl Pts',(-51.9722829502679,-0.119474942214315,
4.14814683201123));
#46638=CARTESIAN_POINT('Ctrl Pts',(-52.0385741275004,1.34988687905908,3.92418167462798));
#46639=CARTESIAN_POINT('Ctrl Pts',(-52.1048653047329,2.38752678457389,3.13358876164514));
#46640=CARTESIAN_POINT('Ctrl Pts',(-52.1711564819654,3.4251666900887,2.34299584866229));
#46641=CARTESIAN_POINT('Ctrl Pts',(-52.2374476591978,4.03108467984492,0.985775180079861));
#46642=CARTESIAN_POINT('Ctrl Pts',(-52.3037388364303,3.92692140729116,-0.314564675583407));
#46643=CARTESIAN_POINT('Ctrl Pts',(-52.3700300136628,3.82275813473739,-1.61490453124667));
#46644=CARTESIAN_POINT('Ctrl Pts',(-52.4363211908953,3.00851359987363,-2.85836357399078));
#46645=CARTESIAN_POINT('Ctrl Pts',(-52.5026123681278,1.85825257794928,-3.4736954429989));
#46646=CARTESIAN_POINT('Ctrl Pts',(-52.5689035453603,0.70799155602493,-4.08902731200702));
#46647=CARTESIAN_POINT('Ctrl Pts',(-52.6351947225927,-0.778285952960015,
-4.07623200727915));
#46648=CARTESIAN_POINT('Ctrl Pts',(-52.7014858998252,-1.91778253551145,
-3.44118770494342));
#46649=CARTESIAN_POINT('Ctrl Pts',(-52.7677770770577,-3.05727911806288,
-2.80614340260768));
#46650=CARTESIAN_POINT('Ctrl Pts',(-52.8340682542902,-3.8499947741808,-1.54885010266406));
#46651=CARTESIAN_POINT('Ctrl Pts',(-52.9003594315227,-3.93175511761398,
-0.246909637889587));
#46652=CARTESIAN_POINT('Ctrl Pts',(-52.9045184470035,-3.93688464688544,
-0.16522771920707));
#46653=CARTESIAN_POINT('Ctrl Pts',(-52.9086774624843,-3.93921576248015,
-0.0833700634079406));
#46654=CARTESIAN_POINT('Ctrl Pts',(-52.9128364779651,-3.93881984523232,
-0.00148943800153567));
#46655=CARTESIAN_POINT('Ctrl Pts',(-53.0961635220347,-3.93911522694479,
-0.00112120486990875));
#46656=CARTESIAN_POINT('Ctrl Pts',(-53.0930813473308,-3.93934370689473,
-0.0617894094753985));
#46657=CARTESIAN_POINT('Ctrl Pts',(-53.089999172627,-3.93806398139047,-0.122447764242017));
#46658=CARTESIAN_POINT('Ctrl Pts',(-53.0869169979231,-3.93524599226671,
-0.183034571912559));
#46659=CARTESIAN_POINT('Ctrl Pts',(-53.0206258206906,-3.87463689823691,
-1.48613098634102));
#46660=CARTESIAN_POINT('Ctrl Pts',(-52.9543346434582,-3.10244125793682,
-2.75613037478151));
#46661=CARTESIAN_POINT('Ctrl Pts',(-52.8880434662257,-1.97340654128442,
-3.40959371435693));
#46662=CARTESIAN_POINT('Ctrl Pts',(-52.8217522889933,-0.844371824631968,
-4.06305705393239));
#46663=CARTESIAN_POINT('Ctrl Pts',(-52.7554611117607,0.641501968372705,
-4.0999843446428));
#46664=CARTESIAN_POINT('Ctrl Pts',(-52.6891699345282,1.80160289177152,-3.50341115122489));
#46665=CARTESIAN_POINT('Ctrl Pts',(-52.6228787572957,2.96170381517028,-2.90683795780702));
#46666=CARTESIAN_POINT('Ctrl Pts',(-52.5565875800633,3.79603186896307,-1.67676428026083));
#46667=CARTESIAN_POINT('Ctrl Pts',(-52.4902964028308,3.92129588868599,-0.378287228889388));
#46668=CARTESIAN_POINT('Ctrl Pts',(-52.4240052255983,4.04655990840891,0.920189822482053));
#46669=CARTESIAN_POINT('Ctrl Pts',(-52.3577140483658,3.46275989406197,2.28707024767885));
#46670=CARTESIAN_POINT('Ctrl Pts',(-52.2914228711333,2.43809417158646,3.09440777607648));
#46671=CARTESIAN_POINT('Ctrl Pts',(-52.2251316939008,1.41342844911096,3.9017453044741));
#46672=CARTESIAN_POINT('Ctrl Pts',(-52.1588405166684,-0.0521029814929644,
4.1495399360726));
#46673=CARTESIAN_POINT('Ctrl Pts',(-52.0925493394359,-1.28523347643839,
3.72395456272073));
#46674=CARTESIAN_POINT('Ctrl Pts',(-52.0262581622034,-2.51836397138382,
3.29836918936886));
#46675=CARTESIAN_POINT('Ctrl Pts',(-51.959966984971,-3.51909353067066,2.19940381106649));
#46676=CARTESIAN_POINT('Ctrl Pts',(-51.8936758077385,-3.82768596737718,
0.931924250843543));
#46677=CARTESIAN_POINT('Ctrl Pts',(-51.8778383791706,-3.9014108713081,0.629114467787446));
#46678=CARTESIAN_POINT('Ctrl Pts',(-51.8620009506027,-3.93563096151905,
0.31668647303777));
#46679=CARTESIAN_POINT('Ctrl Pts',(-51.8461635220348,-3.93274891143005,
0.00363589115318885));
#46680=CARTESIAN_POINT('Origin',(-54.75,0.,0.));
#46681=CARTESIAN_POINT('',(-50.4128364779651,-3.92648515689148,-0.000175634614104081));
#46682=CARTESIAN_POINT('',(-50.5961635220347,-3.92654186868141,-0.000527800881415484));
#46683=CARTESIAN_POINT('',(-54.75,-3.933,-4.81653586104654E-16));
#46684=CARTESIAN_POINT('Ctrl Pts',(-50.4128364779651,-3.92648515689148,
-0.000175634614104081));
#46685=CARTESIAN_POINT('Ctrl Pts',(-50.4465166690278,-3.92621997164172,
0.668244657360119));
#46686=CARTESIAN_POINT('Ctrl Pts',(-50.4801968600906,-3.76456310744387,
1.33678530445738));
#46687=CARTESIAN_POINT('Ctrl Pts',(-50.5138770511533,-3.44223647212953,
1.91589946085585));
#46688=CARTESIAN_POINT('Ctrl Pts',(-50.5801682283858,-2.80781572111349,
3.05574332659173));
#46689=CARTESIAN_POINT('Ctrl Pts',(-50.6464594056182,-1.55095633031185,
3.84914677080616));
#46690=CARTESIAN_POINT('Ctrl Pts',(-50.7127505828507,-0.249060794196362,
3.93161943669027));
#46691=CARTESIAN_POINT('Ctrl Pts',(-50.7790417600832,1.05283474191913,4.01409210257438));
#46692=CARTESIAN_POINT('Ctrl Pts',(-50.8453329373157,2.39976642334848,3.38563399012816));
#46693=CARTESIAN_POINT('Ctrl Pts',(-50.9116241145482,3.17295245283412,2.33495940140731));
#46694=CARTESIAN_POINT('Ctrl Pts',(-50.9779152917807,3.94613848231975,1.28428481268647));
#46695=CARTESIAN_POINT('Ctrl Pts',(-51.0442064690132,4.14557885986166,-0.188606252309012));
#46696=CARTESIAN_POINT('Ctrl Pts',(-51.1104976462456,3.67965047126436,-1.40706612619678));
#46697=CARTESIAN_POINT('Ctrl Pts',(-51.1767888234781,3.21372208266706,-2.62552600008455));
#46698=CARTESIAN_POINT('Ctrl Pts',(-51.2430800007106,2.08242492793056,-3.58955468286462));
#46699=CARTESIAN_POINT('Ctrl Pts',(-51.3093711779431,0.805478081371511,
-3.85627640796099));
#46700=CARTESIAN_POINT('Ctrl Pts',(-51.3756623551755,-0.471468765187465,
-4.12299813305734));
#46701=CARTESIAN_POINT('Ctrl Pts',(-51.441953532408,-1.89406530356897,-3.69241290047008));
#46702=CARTESIAN_POINT('Ctrl Pts',(-51.5082447096405,-2.80876922355138,
-2.76233200810421));
#46703=CARTESIAN_POINT('Ctrl Pts',(-51.5597752990821,-3.51980248814202,
-2.0393456528637));
#46704=CARTESIAN_POINT('Ctrl Pts',(-51.6113058885236,-3.92394015523687,
-1.01453758688934));
#46705=CARTESIAN_POINT('Ctrl Pts',(-51.6628364779651,-3.93339868146552,
0.0036118335011201));
#46706=CARTESIAN_POINT('Ctrl Pts',(-51.8461635220348,-3.93274891143005,
0.00363589115318885));
#46707=CARTESIAN_POINT('Ctrl Pts',(-51.7957097733702,-3.92356748212124,
-0.993658291421522));
#46708=CARTESIAN_POINT('Ctrl Pts',(-51.7452560247056,-3.53784138323085,
-1.99727102772681));
#46709=CARTESIAN_POINT('Ctrl Pts',(-51.694802276041,-2.85325273220719,-2.7163599762032));
#46710=CARTESIAN_POINT('Ctrl Pts',(-51.6285110988085,-1.95377174620445,
-3.66117090088337));
#46711=CARTESIAN_POINT('Ctrl Pts',(-51.562219921576,-0.538354460072711,
-4.11479900810012));
#46712=CARTESIAN_POINT('Ctrl Pts',(-51.4959287443436,0.742754971820343,
-3.868847079687));
#46713=CARTESIAN_POINT('Ctrl Pts',(-51.4296375671111,2.0238644037134,-3.62289515127387));
#46714=CARTESIAN_POINT('Ctrl Pts',(-51.3633463898786,3.17066598136777,-2.67736318723087));
#46715=CARTESIAN_POINT('Ctrl Pts',(-51.2970552126461,3.65631788266093,-1.46662954255678));
#46716=CARTESIAN_POINT('Ctrl Pts',(-51.2307640354136,4.14196978395412,-0.255895897882616));
#46717=CARTESIAN_POINT('Ctrl Pts',(-51.1644728581811,3.96647200888603,1.22003942742267));
#46718=CARTESIAN_POINT('Ctrl Pts',(-51.0981816809486,3.2104484154953,2.283130229665));
#46719=CARTESIAN_POINT('Ctrl Pts',(-51.0318905037161,2.45442482210466,3.34622103190721));
#46720=CARTESIAN_POINT('Ctrl Pts',(-50.9655993264837,1.11787541039155,3.99646731108659));
#46721=CARTESIAN_POINT('Ctrl Pts',(-50.8993081492512,-0.185187647752963,
3.9351452589817));
#46722=CARTESIAN_POINT('Ctrl Pts',(-50.8330169720187,-1.48825070589748,
3.87382320687682));
#46723=CARTESIAN_POINT('Ctrl Pts',(-50.7667257947862,-2.7578274104734,3.10093282348768));
#46724=CARTESIAN_POINT('Ctrl Pts',(-50.7004346175537,-3.4106729200051,1.97154074442055));
#46725=CARTESIAN_POINT('Ctrl Pts',(-50.665677585714,-3.75296541062707,1.37939080697223));
#46726=CARTESIAN_POINT('Ctrl Pts',(-50.6309205538744,-3.92571882340902,
0.689238742796217));
#46727=CARTESIAN_POINT('Ctrl Pts',(-50.5961635220347,-3.92654186868141,
-0.000527800881415484));
#46728=CARTESIAN_POINT('Origin',(-54.75,0.,0.));
#46729=CARTESIAN_POINT('',(-49.1628364779651,-3.93404549041159,-0.00355071844980182));
#46730=CARTESIAN_POINT('',(-49.3461635220347,-3.9346923370435,-0.00345168766750323));
#46731=CARTESIAN_POINT('',(-54.75,-3.933,-4.81653586104654E-16));
#46732=CARTESIAN_POINT('Ctrl Pts',(-49.1628364779651,-3.93404549041159,
-0.00355071844980182));
#46733=CARTESIAN_POINT('Ctrl Pts',(-49.2154362722996,-3.92439753107285,
1.03528607871439));
#46734=CARTESIAN_POINT('Ctrl Pts',(-49.2680360666341,-3.50145870567672,
2.0810673230136));
#46735=CARTESIAN_POINT('Ctrl Pts',(-49.3206358609685,-2.76386836518494,
2.80725743993962));
#46736=CARTESIAN_POINT('Ctrl Pts',(-49.386927038201,-1.83428807679852,3.72247010102922));
#46737=CARTESIAN_POINT('Ctrl Pts',(-49.4532182154335,-0.404934318547125,
4.13006351033546));
#46738=CARTESIAN_POINT('Ctrl Pts',(-49.519509392666,0.867546325602179,3.84278883717289));
#46739=CARTESIAN_POINT('Ctrl Pts',(-49.5858005698985,2.14002696975155,3.5555141640103));
#46740=CARTESIAN_POINT('Ctrl Pts',(-49.652091747131,3.25563449979882,2.57337140837882));
#46741=CARTESIAN_POINT('Ctrl Pts',(-49.7183829243635,3.70185767111709,1.34755796051894));
#46742=CARTESIAN_POINT('Ctrl Pts',(-49.784674101596,4.14808084243537,0.121744512659055));
#46743=CARTESIAN_POINT('Ctrl Pts',(-49.8509652788283,3.92491965502465,-1.34773962742924));
#46744=CARTESIAN_POINT('Ctrl Pts',(-49.9172564560608,3.1348945874868,-2.38581193716362));
#46745=CARTESIAN_POINT('Ctrl Pts',(-49.9835476332933,2.34486951994894,-3.42388424689801));
#46746=CARTESIAN_POINT('Ctrl Pts',(-50.0498388105259,0.987980572283947,
-4.0305447262785));
#46747=CARTESIAN_POINT('Ctrl Pts',(-50.1161299877584,-0.312416079919453,
-3.92709292825803));
#46748=CARTESIAN_POINT('Ctrl Pts',(-50.1824211649909,-1.61281273212285,
-3.82364113023756));
#46749=CARTESIAN_POINT('Ctrl Pts',(-50.2487123422233,-2.85671708886466,
-3.01007705481613));
#46750=CARTESIAN_POINT('Ctrl Pts',(-50.3150035194558,-3.47267821162034,
-1.86015287347675));
#46751=CARTESIAN_POINT('Ctrl Pts',(-50.3476145056255,-3.77569138009754,
-1.29446429862426));
#46752=CARTESIAN_POINT('Ctrl Pts',(-50.3802254917953,-3.9267419236211,-0.647376384056746));
#46753=CARTESIAN_POINT('Ctrl Pts',(-50.4128364779651,-3.92648515689148,
-0.000175634614104081));
#46754=CARTESIAN_POINT('Ctrl Pts',(-50.5961635220347,-3.92654186868141,
-0.000527800881415484));
#46755=CARTESIAN_POINT('Ctrl Pts',(-50.5646293766419,-3.92728859611787,
-0.626334934695071));
#46756=CARTESIAN_POINT('Ctrl Pts',(-50.5330952312491,-3.78651156323261,
-1.25182472892874));
#46757=CARTESIAN_POINT('Ctrl Pts',(-50.5015610858563,-3.50242491031551,
-1.80351945422495));
#46758=CARTESIAN_POINT('Ctrl Pts',(-50.4352699086238,-2.90521707660678,
-2.96329379905778));
#46759=CARTESIAN_POINT('Ctrl Pts',(-50.3689787313913,-1.67468709470198,
-3.79694871397818));
#46760=CARTESIAN_POINT('Ctrl Pts',(-50.3026875541588,-0.3761417015949,-3.92150227521134));
#46761=CARTESIAN_POINT('Ctrl Pts',(-50.2363963769263,0.922403691512177,
-4.0460558364445));
#46762=CARTESIAN_POINT('Ctrl Pts',(-50.1701051996938,2.28896449582153,-3.46150804399042));
#46763=CARTESIAN_POINT('Ctrl Pts',(-50.1038140224614,3.09574127487254,-2.43640075382048));
#46764=CARTESIAN_POINT('Ctrl Pts',(-50.0375228452289,3.9025180539235,-1.41129346365059));
#46765=CARTESIAN_POINT('Ctrl Pts',(-49.9712316679964,4.14951080771618,0.0543733242351024));
#46766=CARTESIAN_POINT('Ctrl Pts',(-49.9049404907639,3.7232508115865,1.28727078277528));
#46767=CARTESIAN_POINT('Ctrl Pts',(-49.8386493135314,3.29699081545681,2.52016824131552));
#46768=CARTESIAN_POINT('Ctrl Pts',(-49.7723581362989,2.19747806940468,3.52029637051022));
#46769=CARTESIAN_POINT('Ctrl Pts',(-49.7060669590665,0.929829857766153,
3.82819528103949));
#46770=CARTESIAN_POINT('Ctrl Pts',(-49.639775781834,-0.337818353872377,
4.13609419156877));
#46771=CARTESIAN_POINT('Ctrl Pts',(-49.5734846046015,-1.77360203109731,
3.75176388343262));
#46772=CARTESIAN_POINT('Ctrl Pts',(-49.507193427369,-2.71792067856389,2.85176609475624));
#46773=CARTESIAN_POINT('Ctrl Pts',(-49.4535167922576,-3.48254501599575,
2.12302880390319));
#46774=CARTESIAN_POINT('Ctrl Pts',(-49.3998401571462,-3.9249499243723,1.05620422076861));
#46775=CARTESIAN_POINT('Ctrl Pts',(-49.3461635220347,-3.9346923370435,-0.00345168766750323));
#46776=CARTESIAN_POINT('Origin',(-54.75,0.,0.));
#46777=CARTESIAN_POINT('',(-47.9128364779652,-3.93845732485478,0.00183569955874766));
#46778=CARTESIAN_POINT('',(-48.0961635220348,-3.93803051256068,0.00216112547147041));
#46779=CARTESIAN_POINT('',(-54.75,-3.933,-4.81653586104654E-16));
#46780=CARTESIAN_POINT('Ctrl Pts',(-47.9128364779652,-3.93845732485478,
0.00183569955874766));
#46781=CARTESIAN_POINT('Ctrl Pts',(-47.9180646983389,-3.93905186643222,
0.104791419839774));
#46782=CARTESIAN_POINT('Ctrl Pts',(-47.9232929187127,-3.93536614512923,
0.207703890362527));
#46783=CARTESIAN_POINT('Ctrl Pts',(-47.9285211390864,-3.92726327363148,
0.310267390732299));
#46784=CARTESIAN_POINT('Ctrl Pts',(-47.9948123163189,-3.82452298111308,
1.61072045019609));
#46785=CARTESIAN_POINT('Ctrl Pts',(-48.0611034935513,-3.01163960867816,
2.85506974856707));
#46786=CARTESIAN_POINT('Ctrl Pts',(-48.1273946707838,-1.86205261215886,
3.47165994067951));
#46787=CARTESIAN_POINT('Ctrl Pts',(-48.1936858480162,-0.712465615639556,
4.08825013279194));
#46788=CARTESIAN_POINT('Ctrl Pts',(-48.2599770252488,0.773825004964064,
4.0770812186458));
#46789=CARTESIAN_POINT('Ctrl Pts',(-48.3262682024813,1.91401581266688,3.44328420886624));
#46790=CARTESIAN_POINT('Ctrl Pts',(-48.3925593797138,3.0542066203697,2.80948719908667));
#46791=CARTESIAN_POINT('Ctrl Pts',(-48.4588505569462,3.84829761517164,1.55306209367373));
#46792=CARTESIAN_POINT('Ctrl Pts',(-48.5251417341787,3.93148257881811,0.251211875945639));
#46793=CARTESIAN_POINT('Ctrl Pts',(-48.5914329114112,4.01466754246458,-1.05063834178238));
#46794=CARTESIAN_POINT('Ctrl Pts',(-48.6577240886437,3.38694647495551,-2.39791367182562));
#46795=CARTESIAN_POINT('Ctrl Pts',(-48.7240152658762,2.33669507914591,-3.17167444440027));
#46796=CARTESIAN_POINT('Ctrl Pts',(-48.7903064431087,1.28644368333625,-3.94543521697496));
#46797=CARTESIAN_POINT('Ctrl Pts',(-48.8565976203412,-0.186338040773995,
-4.14568143208116));
#46798=CARTESIAN_POINT('Ctrl Pts',(-48.9228887975736,-1.40505265711748,
-3.68041977291906));
#46799=CARTESIAN_POINT('Ctrl Pts',(-48.9891799748061,-2.62376727346096,
-3.21515811375696));
#46800=CARTESIAN_POINT('Ctrl Pts',(-49.0554711520386,-3.58841478203762,
-2.08438858032658));
#46801=CARTESIAN_POINT('Ctrl Pts',(-49.1217623292711,-3.85583512706524,
-0.807587857174833));
#46802=CARTESIAN_POINT('Ctrl Pts',(-49.1354537121691,-3.91106652423369,
-0.54388507929504));
#46803=CARTESIAN_POINT('Ctrl Pts',(-49.1491450950671,-3.93655679120968,
-0.273953151358113));
#46804=CARTESIAN_POINT('Ctrl Pts',(-49.1628364779651,-3.93404549041159,
-0.00355071844980182));
#46805=CARTESIAN_POINT('Ctrl Pts',(-49.3461635220347,-3.9346923370435,-0.00345168766750323));
#46806=CARTESIAN_POINT('Ctrl Pts',(-49.3335489799137,-3.93698190073814,
-0.252481345787259));
#46807=CARTESIAN_POINT('Ctrl Pts',(-49.3209344377926,-3.91537565931263,
-0.501115080397896));
#46808=CARTESIAN_POINT('Ctrl Pts',(-49.3083198956715,-3.8684401147974,-0.744871634842373));
#46809=CARTESIAN_POINT('Ctrl Pts',(-49.242028718439,-3.62178728585608,-2.02584630654768));
#46810=CARTESIAN_POINT('Ctrl Pts',(-49.1757375412066,-2.6756280102654,-3.17213038074177));
#46811=CARTESIAN_POINT('Ctrl Pts',(-49.1094463639741,-1.46462883059311,
-3.65711977692308));
#46812=CARTESIAN_POINT('Ctrl Pts',(-49.0431551867416,-0.253629650920743,
-4.14210917310442));
#46813=CARTESIAN_POINT('Ctrl Pts',(-48.9768640095091,1.22220943283327,-3.9658038912729));
#46814=CARTESIAN_POINT('Ctrl Pts',(-48.9105728322766,2.28488643044238,-3.20919875890334));
#46815=CARTESIAN_POINT('Ctrl Pts',(-48.8442816550441,3.34756342805149,-2.45259362653377));
#46816=CARTESIAN_POINT('Ctrl Pts',(-48.7779904778117,3.99707833951569,-1.11568864362615));
#46817=CARTESIAN_POINT('Ctrl Pts',(-48.7116993005792,3.93504334769276,0.187340668156589));
#46818=CARTESIAN_POINT('Ctrl Pts',(-48.6454081233467,3.87300835586984,1.49036997993933));
#46819=CARTESIAN_POINT('Ctrl Pts',(-48.5791169461142,3.09942346075977,2.7595236205972));
#46820=CARTESIAN_POINT('Ctrl Pts',(-48.5128257688817,1.96967435736646,3.41175110465278));
#46821=CARTESIAN_POINT('Ctrl Pts',(-48.4465345916492,0.83992525397314,4.06397858870837));
#46822=CARTESIAN_POINT('Ctrl Pts',(-48.3802434144167,-0.645988057703424,
4.09927991616168));
#46823=CARTESIAN_POINT('Ctrl Pts',(-48.3139522371843,-1.8054354767865,3.50143762093903));
#46824=CARTESIAN_POINT('Ctrl Pts',(-48.2476610599518,-2.96488289586957,
2.90359532571638));
#46825=CARTESIAN_POINT('Ctrl Pts',(-48.1813698827193,-3.79786442235915,
1.67260940781778));
#46826=CARTESIAN_POINT('Ctrl Pts',(-48.1150787054868,-3.92170748781686,
0.373996061700655));
#46827=CARTESIAN_POINT('Ctrl Pts',(-48.1087736443361,-3.93348640219728,
0.250482844705844));
#46828=CARTESIAN_POINT('Ctrl Pts',(-48.1024685831855,-3.93885029408403,
0.1263578551207));
#46829=CARTESIAN_POINT('Ctrl Pts',(-48.0961635220348,-3.93803051256068,
0.00216112547147041));
#46830=CARTESIAN_POINT('Origin',(-54.75,0.,0.));
#46831=CARTESIAN_POINT('',(-46.6628364779651,-3.92838703301762,0.00264903870899197));
#46832=CARTESIAN_POINT('',(-46.8461635220347,-3.92797149977701,0.00239191756703917));
#46833=CARTESIAN_POINT('',(-54.75,-3.933,-4.81653586104654E-16));
#46834=CARTESIAN_POINT('Ctrl Pts',(-46.6628364779651,-3.92838703301762,
0.00264903870899197));
#46835=CARTESIAN_POINT('Ctrl Pts',(-46.6869843016106,-3.93133701178113,
0.481309096112364));
#46836=CARTESIAN_POINT('Ctrl Pts',(-46.7111321252561,-3.85042547221201,
0.959006099363471));
#46837=CARTESIAN_POINT('Ctrl Pts',(-46.7352799489016,-3.68118797282308,
1.40303876742916));
#46838=CARTESIAN_POINT('Ctrl Pts',(-46.8015711261341,-3.21659318237439,
2.62200776140054));
#46839=CARTESIAN_POINT('Ctrl Pts',(-46.8678623033666,-2.08635160875129,
3.58727380700206));
#46840=CARTESIAN_POINT('Ctrl Pts',(-46.9341534805991,-0.809697391222998,
3.85539269190742));
#46841=CARTESIAN_POINT('Ctrl Pts',(-47.0004446578316,0.466956826305223,
4.12351157681276));
#46842=CARTESIAN_POINT('Ctrl Pts',(-47.0667358350641,1.89002368773869,3.69448330102175));
#46843=CARTESIAN_POINT('Ctrl Pts',(-47.1330270122966,2.80574481596238,2.7654038948889));
#46844=CARTESIAN_POINT('Ctrl Pts',(-47.1993181895291,3.72146594418606,1.83632448875605));
#46845=CARTESIAN_POINT('Ctrl Pts',(-47.2656093667615,4.12984133920024,0.407193952281507));
#46846=CARTESIAN_POINT('Ctrl Pts',(-47.331900543994,3.84326292528247,-0.865443678881344));
#46847=CARTESIAN_POINT('Ctrl Pts',(-47.3981917212265,3.5566845113647,-2.1380813100442));
#46848=CARTESIAN_POINT('Ctrl Pts',(-47.464482898459,2.57515228851486,-3.25422603589525));
#46849=CARTESIAN_POINT('Ctrl Pts',(-47.5307740756915,1.34958316758683,-3.70111982350379));
#46850=CARTESIAN_POINT('Ctrl Pts',(-47.597065252924,0.124014046658786,-4.14801361111233));
#46851=CARTESIAN_POINT('Ctrl Pts',(-47.6633564301564,-1.34559197234754,
-3.9256564604784));
#46852=CARTESIAN_POINT('Ctrl Pts',(-47.7296476073889,-2.3840963755497,-3.13619947488313));
#46853=CARTESIAN_POINT('Ctrl Pts',(-47.7907105642476,-3.34069651779697,
-2.40900499945294));
#46854=CARTESIAN_POINT('Ctrl Pts',(-47.8517735211064,-3.93151338139049,
-1.20063478876308));
#46855=CARTESIAN_POINT('Ctrl Pts',(-47.9128364779652,-3.93845732485478,
0.00183569955874766));
#46856=CARTESIAN_POINT('Ctrl Pts',(-48.0961635220348,-3.93803051256068,
0.00216112547147041));
#46857=CARTESIAN_POINT('Ctrl Pts',(-48.036177405953,-3.93023114179386,-1.17944191749285));
#46858=CARTESIAN_POINT('Ctrl Pts',(-47.9761912898711,-3.36271357529152,
-2.36753854712791));
#46859=CARTESIAN_POINT('Ctrl Pts',(-47.9162051737893,-2.43470660670667,
-3.09707384694413));
#46860=CARTESIAN_POINT('Ctrl Pts',(-47.8499139965569,-1.40915805571296,
-3.90328963513612));
#46861=CARTESIAN_POINT('Ctrl Pts',(-47.7836228193244,0.0566436507002789,
-4.14948043718453));
#46862=CARTESIAN_POINT('Ctrl Pts',(-47.7173316420919,1.28930770376171,-3.72254594587994));
#46863=CARTESIAN_POINT('Ctrl Pts',(-47.6510404648594,2.52197175682313,-3.29561145457534));
#46864=CARTESIAN_POINT('Ctrl Pts',(-47.5847492876269,3.52149815653267,-2.19555166991778));
#46865=CARTESIAN_POINT('Ctrl Pts',(-47.5184581103945,3.8287034487138,-0.927735186340111));
#46866=CARTESIAN_POINT('Ctrl Pts',(-47.452166933162,4.13590874089496,0.340081297237703));
#46867=CARTESIAN_POINT('Ctrl Pts',(-47.3858757559295,3.75079292554741,1.77565447973578));
#46868=CARTESIAN_POINT('Ctrl Pts',(-47.319584578697,2.85027860361577,2.71948056730262));
#46869=CARTESIAN_POINT('Ctrl Pts',(-47.2532934014645,1.94976428168418,3.66330665486941));
#46870=CARTESIAN_POINT('Ctrl Pts',(-47.187002224232,0.533851453168638,4.11538564750519));
#46871=CARTESIAN_POINT('Ctrl Pts',(-47.1207110469995,-0.746988074883418,
3.8680319918724));
#46872=CARTESIAN_POINT('Ctrl Pts',(-47.054419869767,-2.0278276029354,3.62067833623963));
#46873=CARTESIAN_POINT('Ctrl Pts',(-46.9881286925346,-3.17359383052384,
2.6738920323384));
#46874=CARTESIAN_POINT('Ctrl Pts',(-46.9218375153021,-3.65792057640951,
1.46262768018602));
#46875=CARTESIAN_POINT('Ctrl Pts',(-46.8966128508797,-3.84221327033675,
1.00172567051489));
#46876=CARTESIAN_POINT('Ctrl Pts',(-46.8713881864572,-3.93073597335362,
0.50252981692053));
#46877=CARTESIAN_POINT('Ctrl Pts',(-46.8461635220347,-3.92797149977701,
0.00239191756703917));
#46878=CARTESIAN_POINT('Origin',(-54.75,0.,0.));
#46879=CARTESIAN_POINT('',(-45.4128364779651,-3.92877816963689,-0.00284985070313576));
#46880=CARTESIAN_POINT('',(-45.5961635220348,-3.92927121084188,-0.0030586176504822));
#46881=CARTESIAN_POINT('',(-54.75,-3.933,-4.81653586104654E-16));
#46882=CARTESIAN_POINT('Ctrl Pts',(-45.4128364779651,-3.92877816963689,
-0.00284985070313576));
#46883=CARTESIAN_POINT('Ctrl Pts',(-45.4559039048824,-3.92308252956803,
0.850622702455208));
#46884=CARTESIAN_POINT('Ctrl Pts',(-45.4989713317997,-3.65002117383353,
1.70741383593766));
#46885=CARTESIAN_POINT('Ctrl Pts',(-45.542038758717,-3.13750342344379,2.38238010024533));
#46886=CARTESIAN_POINT('Ctrl Pts',(-45.6083299359494,-2.3486147561188,3.42131628603418));
#46887=CARTESIAN_POINT('Ctrl Pts',(-45.6746211131819,-0.992390468762286,
4.02946119962105));
#46888=CARTESIAN_POINT('Ctrl Pts',(-45.7409122904143,0.308118608665171,
3.9274324433605));
#46889=CARTESIAN_POINT('Ctrl Pts',(-45.8072034676468,1.6086276860927,3.82540368709996));
#46890=CARTESIAN_POINT('Ctrl Pts',(-45.8734946448794,2.85342155359117,3.01320126099192));
#46891=CARTESIAN_POINT('Ctrl Pts',(-45.9397858221119,3.47064063048122,1.86395179342691));
#46892=CARTESIAN_POINT('Ctrl Pts',(-46.0060769993443,4.08785970737127,0.714702325861893));
#46893=CARTESIAN_POINT('Ctrl Pts',(-46.0723681765768,4.07750399365291,-0.771594183160101));
#46894=CARTESIAN_POINT('Ctrl Pts',(-46.1386593538093,3.4443309148399,-1.91213159150844));
#46895=CARTESIAN_POINT('Ctrl Pts',(-46.2049505310417,2.81115783602689,-3.05266899985677));
#46896=CARTESIAN_POINT('Ctrl Pts',(-46.2712417082743,1.55516739211924,-3.84744730753145));
#46897=CARTESIAN_POINT('Ctrl Pts',(-46.3375328855068,0.253362882493478,
-3.93134454403847));
#46898=CARTESIAN_POINT('Ctrl Pts',(-46.4038240627392,-1.04844162713228,
-4.01524178054549));
#46899=CARTESIAN_POINT('Ctrl Pts',(-46.4701152399717,-2.39606020247614,
-3.38825794588486));
#46900=CARTESIAN_POINT('Ctrl Pts',(-46.5364064172042,-3.17039548651101,
-2.33843005738403));
#46901=CARTESIAN_POINT('Ctrl Pts',(-46.5785497707911,-3.66266439818702,
-1.67102196844027));
#46902=CARTESIAN_POINT('Ctrl Pts',(-46.6206931243781,-3.92323866023133,
-0.832719826959837));
#46903=CARTESIAN_POINT('Ctrl Pts',(-46.6628364779651,-3.92838703301762,
0.00264903870899197));
#46904=CARTESIAN_POINT('Ctrl Pts',(-46.8461635220347,-3.92797149977701,
0.00239191756703917));
#46905=CARTESIAN_POINT('Ctrl Pts',(-46.8050970092247,-3.9234708535981,-0.811847634111943));
#46906=CARTESIAN_POINT('Ctrl Pts',(-46.7640304964146,-3.67701518999008,
-1.6285840611087));
#46907=CARTESIAN_POINT('Ctrl Pts',(-46.7229639836046,-3.20794814162277,
-2.28664194722862));
#46908=CARTESIAN_POINT('Ctrl Pts',(-46.6566728063721,-2.4507616967675,-3.34890482208725));
#46909=CARTESIAN_POINT('Ctrl Pts',(-46.5903816291397,-1.11350154287413,
-3.99768817140092));
#46910=CARTESIAN_POINT('Ctrl Pts',(-46.5240904519072,0.189493632478917,
-3.93494025843041));
#46911=CARTESIAN_POINT('Ctrl Pts',(-46.4577992746747,1.49248880783197,-3.8721923454599));
#46912=CARTESIAN_POINT('Ctrl Pts',(-46.3915080974422,2.7612190046447,-3.0979131702052));
#46913=CARTESIAN_POINT('Ctrl Pts',(-46.3252169202097,3.41282826797689,-1.96780738068143));
#46914=CARTESIAN_POINT('Ctrl Pts',(-46.2589257429772,4.06443753130908,-0.837701591157649));
#46915=CARTESIAN_POINT('Ctrl Pts',(-46.1926345657448,4.09892586116073,0.648230812635207));
#46916=CARTESIAN_POINT('Ctrl Pts',(-46.1263433885123,3.50044928339101,1.80735095888258));
#46917=CARTESIAN_POINT('Ctrl Pts',(-46.0600522112798,2.90197270562126,2.96647110513002));
#46918=CARTESIAN_POINT('Ctrl Pts',(-45.9937610340473,1.67053122023008,3.79877899383193));
#46919=CARTESIAN_POINT('Ctrl Pts',(-45.9274698568148,0.371850309848739,
3.92191152644114));
#46920=CARTESIAN_POINT('Ctrl Pts',(-45.8611786795823,-0.926830600532456,
4.04504405905032));
#46921=CARTESIAN_POINT('Ctrl Pts',(-45.7948875023499,-2.29275093590379,
3.45900123556699));
#46922=CARTESIAN_POINT('Ctrl Pts',(-45.7285963251174,-3.09840549189236,
2.43301173075218));
#46923=CARTESIAN_POINT('Ctrl Pts',(-45.6844520574232,-3.63490268312317,
1.74979026384193));
#46924=CARTESIAN_POINT('Ctrl Pts',(-45.640307789729,-3.92295429860531,0.87147780518392));
#46925=CARTESIAN_POINT('Ctrl Pts',(-45.5961635220348,-3.92927121084188,
-0.0030586176504822));
#46926=CARTESIAN_POINT('Origin',(-54.75,0.,0.));
#46927=CARTESIAN_POINT('',(-44.1628364779651,-3.93877450621935,-0.00153765925571148));
#46928=CARTESIAN_POINT('',(-44.3461635220348,-3.93907979130839,-0.00117182323445835));
#46929=CARTESIAN_POINT('',(-54.75,-3.933,-4.81653586104654E-16));
#46930=CARTESIAN_POINT('Ctrl Pts',(-44.1628364779651,-3.93877450621935,
-0.00153765925571148));
#46931=CARTESIAN_POINT('Ctrl Pts',(-44.2248235081541,-3.93270920820415,
1.21886943562029));
#46932=CARTESIAN_POINT('Ctrl Pts',(-44.2868105383432,-3.32143279835113,
2.44451926788589));
#46933=CARTESIAN_POINT('Ctrl Pts',(-44.3487975685322,-2.3401643356023,3.16911557954921));
#46934=CARTESIAN_POINT('Ctrl Pts',(-44.4150887457647,-1.29076026868109,
3.94402514324342));
#46935=CARTESIAN_POINT('Ctrl Pts',(-44.4813799229971,0.181801451039536,
4.14588285340311));
#46936=CARTESIAN_POINT('Ctrl Pts',(-44.5476711002296,1.40102445773471,3.68195507074647));
#46937=CARTESIAN_POINT('Ctrl Pts',(-44.6139622774621,2.62024746442988,3.21802728808982));
#46938=CARTESIAN_POINT('Ctrl Pts',(-44.6802534546946,3.58613175809952,2.08831401261689));
#46939=CARTESIAN_POINT('Ctrl Pts',(-44.7465446319271,3.85494910261997,0.811806682884503));
#46940=CARTESIAN_POINT('Ctrl Pts',(-44.8128358091596,4.12376644714041,-0.464700646847811));
#46941=CARTESIAN_POINT('Ctrl Pts',(-44.8791269863921,3.69551684251162,-1.88800203083967));
#46942=CARTESIAN_POINT('Ctrl Pts',(-44.9454181636245,2.76693859675673,-2.80423135207214));
#46943=CARTESIAN_POINT('Ctrl Pts',(-45.011709340857,1.83836035100179,-3.72046067330466));
#46944=CARTESIAN_POINT('Ctrl Pts',(-45.0780005180896,0.409453464120721,
-4.12961793177789));
#46945=CARTESIAN_POINT('Ctrl Pts',(-45.144291695322,-0.863340773085724,
-3.84373586289357));
#46946=CARTESIAN_POINT('Ctrl Pts',(-45.2105828725545,-2.13613501029217,
-3.55785379400925));
#46947=CARTESIAN_POINT('Ctrl Pts',(-45.276874049787,-3.25281659782392,-2.57693239776739));
#46948=CARTESIAN_POINT('Ctrl Pts',(-45.3431652270194,-3.70038086794309,
-1.35160797065096));
#46949=CARTESIAN_POINT('Ctrl Pts',(-45.3663889773347,-3.85717580345627,
-0.922340762879227));
#46950=CARTESIAN_POINT('Ctrl Pts',(-45.3896127276499,-3.93184949598054,
-0.463077797766648));
#46951=CARTESIAN_POINT('Ctrl Pts',(-45.4128364779651,-3.92877816963689,
-0.00284985070313576));
#46952=CARTESIAN_POINT('Ctrl Pts',(-45.5961635220348,-3.92927121084188,
-0.0030586176504822));
#46953=CARTESIAN_POINT('Ctrl Pts',(-45.5740166124965,-3.93244036713718,
-0.441808200690738));
#46954=CARTESIAN_POINT('Ctrl Pts',(-45.5518697029582,-3.86469781064446,
-0.879607367737818));
#46955=CARTESIAN_POINT('Ctrl Pts',(-45.5297227934199,-3.72183996581203,
-1.29134423878791));
#46956=CARTESIAN_POINT('Ctrl Pts',(-45.4634316161874,-3.2942311071373,-2.523774517367));
#46957=CARTESIAN_POINT('Ctrl Pts',(-45.3971404389549,-2.19362461318191,
-3.52269888837872));
#46958=CARTESIAN_POINT('Ctrl Pts',(-45.3308492617225,-0.925640237191606,
-3.82921047024818));
#46959=CARTESIAN_POINT('Ctrl Pts',(-45.26455808449,0.34234413879855,-4.13572205211761));
#46960=CARTESIAN_POINT('Ctrl Pts',(-45.1982669072575,1.77770639682364,-3.74982084484499));
#46961=CARTESIAN_POINT('Ctrl Pts',(-45.131975730025,2.72103964195195,-2.84879025923153));
#46962=CARTESIAN_POINT('Ctrl Pts',(-45.0656845527925,3.66437288708031,-1.94775967361802));
#46963=CARTESIAN_POINT('Ctrl Pts',(-44.99939337556,4.11567711931186,-0.53159970966378));
#46964=CARTESIAN_POINT('Ctrl Pts',(-44.9331021983276,3.86762271103424,0.749104291309692));
#46965=CARTESIAN_POINT('Ctrl Pts',(-44.8668110210951,3.61956830275662,2.02980829228316));
#46966=CARTESIAN_POINT('Ctrl Pts',(-44.8005198438626,2.67215525396966,3.17505633027576));
#46967=CARTESIAN_POINT('Ctrl Pts',(-44.7342286666301,1.46062609193479,3.65872028088043));
#46968=CARTESIAN_POINT('Ctrl Pts',(-44.6679374893976,0.24909692989985,4.14238423148512));
#46969=CARTESIAN_POINT('Ctrl Pts',(-44.6016463121651,-1.22654834538313,
3.96446409470183));
#46970=CARTESIAN_POINT('Ctrl Pts',(-44.5353551349326,-2.28839677949802,
3.20669656402809));
#46971=CARTESIAN_POINT('Ctrl Pts',(-44.4722912639667,-3.29855039918072,
2.48582003457673));
#46972=CARTESIAN_POINT('Ctrl Pts',(-44.4092273930007,-3.93421683623724,
1.24018015439934));
#46973=CARTESIAN_POINT('Ctrl Pts',(-44.3461635220348,-3.93907979130839,
-0.00117182323445835));
#46974=CARTESIAN_POINT('Origin',(-54.75,0.,0.));
#46975=CARTESIAN_POINT('',(-42.9128364779651,-3.93348651618965,0.00360571708670418));
#46976=CARTESIAN_POINT('',(-43.0961635220348,-3.93283616785734,0.00363483404017096));
#46977=CARTESIAN_POINT('',(-54.75,-3.933,-4.81653586104654E-16));
#46978=CARTESIAN_POINT('Ctrl Pts',(-42.9128364779651,-3.93348651618965,
0.00360571708670418));
#46979=CARTESIAN_POINT('Ctrl Pts',(-42.9274519341934,-3.93617042421601,
0.292363665661577));
#46980=CARTESIAN_POINT('Ctrl Pts',(-42.9420673904217,-3.90708356166905,
0.580585604486907));
#46981=CARTESIAN_POINT('Ctrl Pts',(-42.95668284665,-3.84420764986457,0.861237608845054));
#46982=CARTESIAN_POINT('Ctrl Pts',(-43.0229740238825,-3.55902201159384,
2.13418807107819));
#46983=CARTESIAN_POINT('Ctrl Pts',(-43.089265201115,-2.57871173560324,3.25140618600691));
#46984=CARTESIAN_POINT('Ctrl Pts',(-43.1555563783475,-1.35363236910501,
3.69964080465626));
#46985=CARTESIAN_POINT('Ctrl Pts',(-43.2218475555799,-0.128553002606771,
4.14787542330561));
#46986=CARTESIAN_POINT('Ctrl Pts',(-43.2881387328124,1.34129545439917,3.9271265456756));
#46987=CARTESIAN_POINT('Ctrl Pts',(-43.3544299100449,2.38066311176446,3.13880643277829));
#46988=CARTESIAN_POINT('Ctrl Pts',(-43.4207210872774,3.42003076912981,2.35048631988094));
#46989=CARTESIAN_POINT('Ctrl Pts',(-43.4870122645099,4.02891762685445,0.994594971716387));
#46990=CARTESIAN_POINT('Ctrl Pts',(-43.5533034417424,3.92760043739446,-0.305969734361532));
#46991=CARTESIAN_POINT('Ctrl Pts',(-43.6195946189749,3.82628324793448,-1.6065344404393));
#46992=CARTESIAN_POINT('Ctrl Pts',(-43.6858857962073,3.01476201128989,-2.85177250443036));
#46993=CARTESIAN_POINT('Ctrl Pts',(-43.7521769734398,1.86585041671237,-3.46962028133061));
#46994=CARTESIAN_POINT('Ctrl Pts',(-43.8184681506723,0.716938822134715,
-4.08746805823093));
#46995=CARTESIAN_POINT('Ctrl Pts',(-43.8847593279048,-0.769363130376017,
-4.07792554804035));
#46996=CARTESIAN_POINT('Ctrl Pts',(-43.9510505051373,-1.91024679794475,
-3.44537658973707));
#46997=CARTESIAN_POINT('Ctrl Pts',(-44.0173416823698,-3.05113046551329,
-2.81282763143391));
#46998=CARTESIAN_POINT('Ctrl Pts',(-44.0836328596022,-3.84659584814002,
-1.55727222501828));
#46999=CARTESIAN_POINT('Ctrl Pts',(-44.1499240368347,-3.93120533239265,
-0.255513813196189));
#47000=CARTESIAN_POINT('Ctrl Pts',(-44.1542281838782,-3.93669884867488,
-0.170993370907197));
#47001=CARTESIAN_POINT('Ctrl Pts',(-44.1585323309216,-3.93919565778025,
-0.0862781537303368));
#47002=CARTESIAN_POINT('Ctrl Pts',(-44.1628364779651,-3.93877450621935,
-0.00153765925571148));
#47003=CARTESIAN_POINT('Ctrl Pts',(-44.3461635220348,-3.93907979130839,
-0.00117182323445835));
#47004=CARTESIAN_POINT('Ctrl Pts',(-44.3429362157683,-3.93932865401114,
-0.0646982600836412));
#47005=CARTESIAN_POINT('Ctrl Pts',(-44.3397089095017,-3.93792550472575,
-0.128213467339758));
#47006=CARTESIAN_POINT('Ctrl Pts',(-44.3364816032352,-3.9348359912255,-0.191646540075454));
#47007=CARTESIAN_POINT('Ctrl Pts',(-44.2701904260027,-3.87137517589129,
-1.49460718894119));
#47008=CARTESIAN_POINT('Ctrl Pts',(-44.2038992487702,-3.09640195227602,
-2.76291356210852));
#47009=CARTESIAN_POINT('Ctrl Pts',(-44.1376080715377,-1.96593981492416,
-3.41390440965508));
#47010=CARTESIAN_POINT('Ctrl Pts',(-44.0713168943052,-0.835477677572302,
-4.06489525720164));
#47011=CARTESIAN_POINT('Ctrl Pts',(-44.0050257170728,0.650473373516086,
-4.09857057912738));
#47012=CARTESIAN_POINT('Ctrl Pts',(-43.9387345398403,1.8092658999398,-3.49945989796732));
#47013=CARTESIAN_POINT('Ctrl Pts',(-43.8724433626078,2.96805842636345,-2.9003492168073));
#47014=CARTESIAN_POINT('Ctrl Pts',(-43.8061521853753,3.79969242812238,-1.66845253256158));
#47015=CARTESIAN_POINT('Ctrl Pts',(-43.7398610081428,3.922114391023,-0.369704446682378));
#47016=CARTESIAN_POINT('Ctrl Pts',(-43.6735698309103,4.04453635392363,0.929043639196903));
#47017=CARTESIAN_POINT('Ctrl Pts',(-43.6072786536779,3.45774627796568,2.29464312670978));
#47018=CARTESIAN_POINT('Ctrl Pts',(-43.5409874764454,2.43131612646438,3.09973620931858));
#47019=CARTESIAN_POINT('Ctrl Pts',(-43.4746962992129,1.40488597496313,3.90482929192733));
#47020=CARTESIAN_POINT('Ctrl Pts',(-43.4084051219804,-0.0611842520814183,
4.14941596963223));
#47021=CARTESIAN_POINT('Ctrl Pts',(-43.3421139447479,-1.29338038724425,
3.72113287159413));
#47022=CARTESIAN_POINT('Ctrl Pts',(-43.2758227675154,-2.52557652240714,
3.292849773556));
#47023=CARTESIAN_POINT('Ctrl Pts',(-43.209531590283,-3.52389856568822,2.1916968997748));
#47024=CARTESIAN_POINT('Ctrl Pts',(-43.1432404130505,-3.82971634549056,
0.923545010949064));
#47025=CARTESIAN_POINT('Ctrl Pts',(-43.1275481160453,-3.90210883617312,
0.623350974306624));
#47026=CARTESIAN_POINT('Ctrl Pts',(-43.11185581904,-3.9356966539327,0.313799100465172));
#47027=CARTESIAN_POINT('Ctrl Pts',(-43.0961635220348,-3.93283616785734,
0.00363483404017096));
#47028=CARTESIAN_POINT('Origin',(-54.75,0.,0.));
#47029=CARTESIAN_POINT('',(-41.6628364779652,-3.92648186165433,-0.000127976707175181));
#47030=CARTESIAN_POINT('',(-41.8461635220348,-3.92653091726897,-0.000480548798261107));
#47031=CARTESIAN_POINT('',(-54.75,-3.933,-4.81653586104654E-16));
#47032=CARTESIAN_POINT('Ctrl Pts',(-41.6628364779652,-3.92648186165433,
-0.000127976707175181));
#47033=CARTESIAN_POINT('Ctrl Pts',(-41.6963715374652,-3.92628947513322,
0.665413412504115));
#47034=CARTESIAN_POINT('Ctrl Pts',(-41.7299065969653,-3.76609621217257,
1.33104174019653));
#47035=CARTESIAN_POINT('Ctrl Pts',(-41.7634416564653,-3.44642123324494,
1.90836143253966));
#47036=CARTESIAN_POINT('Ctrl Pts',(-41.8297328336978,-2.81449658480804,
3.04959101779987));
#47037=CARTESIAN_POINT('Ctrl Pts',(-41.8960240109302,-1.55937659174049,
3.84574323725253));
#47038=CARTESIAN_POINT('Ctrl Pts',(-41.9623151881627,-0.257664667409214,
3.93106494392236));
#47039=CARTESIAN_POINT('Ctrl Pts',(-42.0286063653952,1.04404725692214,4.0163866505922));
#47040=CARTESIAN_POINT('Ctrl Pts',(-42.0948975426277,2.39235111251722,3.39087784447915));
#47041=CARTESIAN_POINT('Ctrl Pts',(-42.1611887198602,3.167834723898,2.34189791328156));
#47042=CARTESIAN_POINT('Ctrl Pts',(-42.2274798970927,3.94331833527879,1.29291798208397));
#47043=CARTESIAN_POINT('Ctrl Pts',(-42.2937710743251,4.14598170244526,-0.179533074198152));
#47044=CARTESIAN_POINT('Ctrl Pts',(-42.3600622515576,3.68272106645958,-1.39900972863711));
#47045=CARTESIAN_POINT('Ctrl Pts',(-42.4263534287901,3.2194604304739,-2.61848638307606));
#47046=CARTESIAN_POINT('Ctrl Pts',(-42.4926446060227,2.09027579133607,-3.58498863567185));
#47047=CARTESIAN_POINT('Ctrl Pts',(-42.5589357832551,0.813915731527926,
-3.85450435933569));
#47048=CARTESIAN_POINT('Ctrl Pts',(-42.6252269604876,-0.462444328280213,
-4.12402008299952));
#47049=CARTESIAN_POINT('Ctrl Pts',(-42.6915181377201,-1.88597980875866,
-3.6965492777314));
#47050=CARTESIAN_POINT('Ctrl Pts',(-42.7578093149525,-2.80271704872243,
-2.76847247032855));
#47051=CARTESIAN_POINT('Ctrl Pts',(-42.8094850359567,-3.51733790513564,
-2.04501212202889));
#47052=CARTESIAN_POINT('Ctrl Pts',(-42.8611607569609,-3.92399704968205,
-1.01735284590414));
#47053=CARTESIAN_POINT('Ctrl Pts',(-42.9128364779651,-3.93348651618965,
0.00360571708670418));
#47054=CARTESIAN_POINT('Ctrl Pts',(-43.0961635220348,-3.93283616785734,
0.00363483404017096));
#47055=CARTESIAN_POINT('Ctrl Pts',(-43.0455646418076,-3.92361270030057,
-0.996471432262334));
#47056=CARTESIAN_POINT('Ctrl Pts',(-42.9949657615803,-3.53543558165237,
-2.00294475494378));
#47057=CARTESIAN_POINT('Ctrl Pts',(-42.944366881353,-2.8473010620486,-2.72259790204565));
#47058=CARTESIAN_POINT('Ctrl Pts',(-42.8780757041205,-1.94575448248074,
-3.6654380223444));
#47059=CARTESIAN_POINT('Ctrl Pts',(-42.811784526888,-0.529347807021448,
-4.11596735907168));
#47060=CARTESIAN_POINT('Ctrl Pts',(-42.7454933496556,0.751220283488789,
-3.86721227240521));
#47061=CARTESIAN_POINT('Ctrl Pts',(-42.6792021724231,2.03178837399903,-3.61845718573874));
#47062=CARTESIAN_POINT('Ctrl Pts',(-42.6129109951906,3.17651787956021,-2.67041767567851));
#47063=CARTESIAN_POINT('Ctrl Pts',(-42.5466198179581,3.65951889009668,-1.45862406643797));
#47064=CARTESIAN_POINT('Ctrl Pts',(-42.4803286407256,4.14251990063314,-0.246830457197423));
#47065=CARTESIAN_POINT('Ctrl Pts',(-42.4140374634931,3.9637924161449,1.22871725122344));
#47066=CARTESIAN_POINT('Ctrl Pts',(-42.3477462862606,3.20544402649396,2.29015092672527));
#47067=CARTESIAN_POINT('Ctrl Pts',(-42.2814551090281,2.44709563684303,3.35158460222709));
#47068=CARTESIAN_POINT('Ctrl Pts',(-42.2151639317957,1.1091263420294,3.99890424480987));
#47069=CARTESIAN_POINT('Ctrl Pts',(-42.1488727545632,-0.193799390301712,
3.93473054610924));
#47070=CARTESIAN_POINT('Ctrl Pts',(-42.0825815773307,-1.49672512263282,
3.87055684740861));
#47071=CARTESIAN_POINT('Ctrl Pts',(-42.0162904000982,-2.76460729248141,
3.09488980742457));
#47072=CARTESIAN_POINT('Ctrl Pts',(-41.9499992228657,-3.4149795293652,1.96407166065373));
#47073=CARTESIAN_POINT('Ctrl Pts',(-41.9153873225887,-3.75455139919333,
1.37364972878524));
#47074=CARTESIAN_POINT('Ctrl Pts',(-41.8807754223118,-3.92578480029153,
0.68641057942328));
#47075=CARTESIAN_POINT('Ctrl Pts',(-41.8461635220348,-3.92653091726897,
-0.000480548798261107));
#47076=CARTESIAN_POINT('Origin',(-54.75,0.,0.));
#47077=CARTESIAN_POINT('',(-40.4128364779651,-3.93395781977791,-0.00356119310522762));
#47078=CARTESIAN_POINT('',(-40.5961635220348,-3.93460565980472,-0.0034672176766425));
#47079=CARTESIAN_POINT('',(-54.75,-3.933,-4.81653586104654E-16));
#47080=CARTESIAN_POINT('Ctrl Pts',(-40.4128364779651,-3.93395781977791,
-0.00356119310522762));
#47081=CARTESIAN_POINT('Ctrl Pts',(-40.465291140737,-3.92433020604628,1.03246856934012));
#47082=CARTESIAN_POINT('Ctrl Pts',(-40.5177458035087,-3.50397405571284,
2.07540741768839));
#47083=CARTESIAN_POINT('Ctrl Pts',(-40.5702004662806,-2.77000551514533,
2.80120190636642));
#47084=CARTESIAN_POINT('Ctrl Pts',(-40.6364916435131,-1.84243042391868,
3.71844679063188));
#47085=CARTESIAN_POINT('Ctrl Pts',(-40.7027828207456,-0.413972119407498,
4.12916740833972));
#47086=CARTESIAN_POINT('Ctrl Pts',(-40.769073997978,0.859134186788709,3.84467828605429));
#47087=CARTESIAN_POINT('Ctrl Pts',(-40.8353651752105,2.13224049298506,3.56018916376883));
#47088=CARTESIAN_POINT('Ctrl Pts',(-40.901656352443,3.24999480086639,2.58049030148992));
#47089=CARTESIAN_POINT('Ctrl Pts',(-40.9679475296755,3.69889963386485,1.35565636234294));
#47090=CARTESIAN_POINT('Ctrl Pts',(-41.0342387069079,4.14780446686328,0.130822423196035));
#47091=CARTESIAN_POINT('Ctrl Pts',(-41.1005298841405,3.92785982497892,-1.33914659281891));
#47092=CARTESIAN_POINT('Ctrl Pts',(-41.1668210613729,3.14010850249658,-2.37894541062108));
#47093=CARTESIAN_POINT('Ctrl Pts',(-41.2331122386054,2.35235718001424,-3.41874422842326));
#47094=CARTESIAN_POINT('Ctrl Pts',(-41.2994034158379,0.996799176933934,
-4.02837284801268));
#47095=CARTESIAN_POINT('Ctrl Pts',(-41.3656945930704,-0.303820768464218,
-3.92776725568309));
#47096=CARTESIAN_POINT('Ctrl Pts',(-41.4319857703029,-1.60444071386237,
-3.8271616633535));
#47097=CARTESIAN_POINT('Ctrl Pts',(-41.4982769475354,-2.85012260157836,
-3.01632185910491));
#47098=CARTESIAN_POINT('Ctrl Pts',(-41.5645681247679,-3.46859889353324,
-1.86774848144669));
#47099=CARTESIAN_POINT('Ctrl Pts',(-41.5973242425003,-3.77420339596868,
-1.30020983824283));
#47100=CARTESIAN_POINT('Ctrl Pts',(-41.6300803602327,-3.92666977948211,
-0.650210380788743));
#47101=CARTESIAN_POINT('Ctrl Pts',(-41.6628364779652,-3.92648186165433,
-0.000127976707175181));
#47102=CARTESIAN_POINT('Ctrl Pts',(-41.8461635220348,-3.92653091726897,
-0.000480548798261107));
#47103=CARTESIAN_POINT('Ctrl Pts',(-41.8144842450793,-3.92721381668161,
-0.629172244864202));
#47104=CARTESIAN_POINT('Ctrl Pts',(-41.7828049681238,-3.7850758618333,-1.257572396157));
#47105=CARTESIAN_POINT('Ctrl Pts',(-41.7511256911683,-3.49846946496413,
-1.81118029938491));
#47106=CARTESIAN_POINT('Ctrl Pts',(-41.6848345139358,-2.89872485976027,
-2.96964485909509));
#47107=CARTESIAN_POINT('Ctrl Pts',(-41.6185433367033,-1.66637334543348,
-3.80060472495772));
#47108=CARTESIAN_POINT('Ctrl Pts',(-41.5522521594708,-0.367558472842394,
-3.92231608150187));
#47109=CARTESIAN_POINT('Ctrl Pts',(-41.4859609822384,0.931256399748549,
-4.04402743804601));
#47110=CARTESIAN_POINT('Ctrl Pts',(-41.4196698050059,2.29653463060386,-3.45649028527188));
#47111=CARTESIAN_POINT('Ctrl Pts',(-41.3533786277734,3.10106599882443,-2.42961979435086));
#47112=CARTESIAN_POINT('Ctrl Pts',(-41.2870874505409,3.90559736704504,-1.40274930342978));
#47113=CARTESIAN_POINT('Ctrl Pts',(-41.2207962733084,4.1493818726309,0.0634545256380817));
#47114=CARTESIAN_POINT('Ctrl Pts',(-41.1545050960759,3.7204246634379,1.29541614852119));
#47115=CARTESIAN_POINT('Ctrl Pts',(-41.0882139188435,3.29146745424492,2.52737777140422));
#47116=CARTESIAN_POINT('Ctrl Pts',(-41.021922741611,2.18976853027304,3.52509718810241));
#47117=CARTESIAN_POINT('Ctrl Pts',(-40.9556315643785,0.921449508239053,
3.83022107428964));
#47118=CARTESIAN_POINT('Ctrl Pts',(-40.889340387146,-0.346869513795076,
4.1353449604769));
#47119=CARTESIAN_POINT('Ctrl Pts',(-40.8230492099135,-1.78180863389144,
3.74787331615304));
#47120=CARTESIAN_POINT('Ctrl Pts',(-40.756758032681,-2.72415534711707,2.84581101251294));
#47121=CARTESIAN_POINT('Ctrl Pts',(-40.7032265291323,-3.48511990573802,
2.11737695198714));
#47122=CARTESIAN_POINT('Ctrl Pts',(-40.6496950255835,-3.92486997045577,
1.05338356108175));
#47123=CARTESIAN_POINT('Ctrl Pts',(-40.5961635220348,-3.93460565980472,
-0.0034672176766425));
#47124=CARTESIAN_POINT('Origin',(-54.75,0.,0.));
#47125=CARTESIAN_POINT('',(-39.1628364779651,-3.93851028872272,0.00178997264115022));
#47126=CARTESIAN_POINT('',(-39.3461635220348,-3.93809135854538,0.00211875562057622));
#47127=CARTESIAN_POINT('',(-54.75,-3.933,-4.81653586104654E-16));
#47128=CARTESIAN_POINT('Ctrl Pts',(-39.1628364779651,-3.93851028872272,
0.00178997264115022));
#47129=CARTESIAN_POINT('Ctrl Pts',(-39.1679195667762,-3.93907624687778,
0.101884155187649));
#47130=CARTESIAN_POINT('Ctrl Pts',(-39.1730026555873,-3.93559258861192,
0.201938296474208));
#47131=CARTESIAN_POINT('Ctrl Pts',(-39.1780857443984,-3.92793289817642,
0.301671711616751));
#47132=CARTESIAN_POINT('Ctrl Pts',(-39.2443769216309,-3.82803893309399,
1.60234650698859));
#47133=CARTESIAN_POINT('Ctrl Pts',(-39.3106680988634,-3.01788080397012,
2.84847184552886));
#47134=CARTESIAN_POINT('Ctrl Pts',(-39.3769592760959,-1.86964598706206,
3.46757646739465));
#47135=CARTESIAN_POINT('Ctrl Pts',(-39.4432504533283,-0.721411170153998,
4.08668108926045));
#47136=CARTESIAN_POINT('Ctrl Pts',(-39.5095416305608,0.764900334538259,
4.07876499445177));
#47137=CARTESIAN_POINT('Ctrl Pts',(-39.5758328077933,1.90647549585776,3.44746484505069));
#47138=CARTESIAN_POINT('Ctrl Pts',(-39.6421239850258,3.04805065717726,2.8161646956496));
#47139=CARTESIAN_POINT('Ctrl Pts',(-39.7084151622583,3.84488947512401,1.5614804916561));
#47140=CARTESIAN_POINT('Ctrl Pts',(-39.7747063394908,3.93092337866962,0.259815444489133));
#47141=CARTESIAN_POINT('Ctrl Pts',(-39.8409975167232,4.01695728221523,-1.04184960267776));
#47142=CARTESIAN_POINT('Ctrl Pts',(-39.9072886939557,3.39218627135978,-2.39049549301812));
#47143=CARTESIAN_POINT('Ctrl Pts',(-39.9735798711882,2.34363078990284,-3.16655291994083));
#47144=CARTESIAN_POINT('Ctrl Pts',(-40.0398710484207,1.29507530844585,-3.94261034686359));
#47145=CARTESIAN_POINT('Ctrl Pts',(-40.1061622256532,-0.177264643612693,
-4.14607931036863));
#47146=CARTESIAN_POINT('Ctrl Pts',(-40.1724534028857,-1.39699458073947,
-3.68348595973311));
#47147=CARTESIAN_POINT('Ctrl Pts',(-40.2387445801181,-2.61672451786624,
-3.2208926090976));
#47148=CARTESIAN_POINT('Ctrl Pts',(-40.3050357573506,-3.58384444006126,
-2.09223694432154));
#47149=CARTESIAN_POINT('Ctrl Pts',(-40.3713269345831,-3.8540584621877,-0.816024536521914));
#47150=CARTESIAN_POINT('Ctrl Pts',(-40.3851634490438,-3.91045842943398,
-0.549649248397481));
#47151=CARTESIAN_POINT('Ctrl Pts',(-40.3989999635045,-3.93649739604398,
-0.276845588281384));
#47152=CARTESIAN_POINT('Ctrl Pts',(-40.4128364779651,-3.93395781977791,
-0.00356119310522762));
#47153=CARTESIAN_POINT('Ctrl Pts',(-40.5961635220348,-3.93460565980472,
-0.0034672176766425));
#47154=CARTESIAN_POINT('Ctrl Pts',(-40.5834038483511,-3.93692624134911,
-0.255376283841459));
#47155=CARTESIAN_POINT('Ctrl Pts',(-40.5706441746673,-3.91481571134161,
-0.506879545074775));
#47156=CARTESIAN_POINT('Ctrl Pts',(-40.5578845009836,-3.86680067610839,
-0.753336050786185));
#47157=CARTESIAN_POINT('Ctrl Pts',(-40.4915933237511,-3.6173449855192,-2.03376784748931));
#47158=CARTESIAN_POINT('Ctrl Pts',(-40.4253021465186,-2.66867929798575,
-3.17797847793916));
#47159=CARTESIAN_POINT('Ctrl Pts',(-40.3590109692861,-1.4566216042955,-3.66031640381895));
#47160=CARTESIAN_POINT('Ctrl Pts',(-40.2927197920536,-0.244563910605384,
-4.14265432969868));
#47161=CARTESIAN_POINT('Ctrl Pts',(-40.2264286148211,1.23088578924157,-3.96311955100839));
#47162=CARTESIAN_POINT('Ctrl Pts',(-40.1601374375887,2.29190438838525,-3.20419052939536));
#47163=CARTESIAN_POINT('Ctrl Pts',(-40.0938462603562,3.35292298752899,-2.44526150778228));
#47164=CARTESIAN_POINT('Ctrl Pts',(-40.0275550831237,3.99951048596956,-1.10693824324645));
#47165=CARTESIAN_POINT('Ctrl Pts',(-39.9612639058912,3.9346239231132,0.195952182513227));
#47166=CARTESIAN_POINT('Ctrl Pts',(-39.8949727286587,3.86973736025686,1.49884260827283));
#47167=CARTESIAN_POINT('Ctrl Pts',(-39.8286815514262,3.09337673610367,2.76630019525617));
#47168=CARTESIAN_POINT('Ctrl Pts',(-39.7623903741937,1.96220291842955,3.4160536267853));
#47169=CARTESIAN_POINT('Ctrl Pts',(-39.6960991969613,0.831029100755363,
4.06580705831447));
#47170=CARTESIAN_POINT('Ctrl Pts',(-39.6298080197288,-0.654957910439967,
4.09785633438925));
#47171=CARTESIAN_POINT('Ctrl Pts',(-39.5635168424963,-1.81309415664482,
3.49747798467794));
#47172=CARTESIAN_POINT('Ctrl Pts',(-39.4972256652638,-2.97123040284968,
2.89709963496662));
#47173=CARTESIAN_POINT('Ctrl Pts',(-39.4309344880313,-3.80151588406417,
1.66429365946932));
#47174=CARTESIAN_POINT('Ctrl Pts',(-39.3646433107988,-3.92251659781723,
0.365412388972747));
#47175=CARTESIAN_POINT('Ctrl Pts',(-39.3584833812108,-3.9337602641381,0.244717335671718));
#47176=CARTESIAN_POINT('Ctrl Pts',(-39.3523234516228,-3.93887957109934,
0.123451751506461));
#47177=CARTESIAN_POINT('Ctrl Pts',(-39.3461635220348,-3.93809135854538,
0.00211875562057622));
#47178=CARTESIAN_POINT('Origin',(-54.75,0.,0.));
#47179=CARTESIAN_POINT('',(-37.9128364779651,-3.92844641092988,0.00268183597320199));
#47180=CARTESIAN_POINT('',(-38.0961635220348,-3.9280248704326,0.00242793667101629));
#47181=CARTESIAN_POINT('',(-54.75,-3.933,-4.81653586104654E-16));
#47182=CARTESIAN_POINT('Ctrl Pts',(-37.9128364779651,-3.92844641092988,
0.00268183597320199));
#47183=CARTESIAN_POINT('Ctrl Pts',(-37.936839170048,-3.93141775465169,0.478447039929781));
#47184=CARTESIAN_POINT('Ctrl Pts',(-37.9608418621308,-3.85150376888296,
0.953247942279258));
#47185=CARTESIAN_POINT('Ctrl Pts',(-37.9848445542137,-3.6842497503381,1.39497901464505));
#47186=CARTESIAN_POINT('Ctrl Pts',(-38.0511357314461,-3.22232382353224,
2.61496186932779));
#47187=CARTESIAN_POINT('Ctrl Pts',(-38.1174269086786,-2.09419747098634,
3.58269917161015));
#47188=CARTESIAN_POINT('Ctrl Pts',(-38.1837180859111,-0.818133097235401,
3.85361141130945));
#47189=CARTESIAN_POINT('Ctrl Pts',(-38.2500092631436,0.457931276515689,
4.12452365100879));
#47190=CARTESIAN_POINT('Ctrl Pts',(-38.3163004403761,1.88193367147187,3.69861082812487));
#47191=CARTESIAN_POINT('Ctrl Pts',(-38.3825916176086,2.79968592545767,2.77153773074816));
#47192=CARTESIAN_POINT('Ctrl Pts',(-38.4488827948411,3.71743817944343,1.8444646333715));
#47193=CARTESIAN_POINT('Ctrl Pts',(-38.5151739720736,4.12894029245886,0.416231261502113));
#47194=CARTESIAN_POINT('Ctrl Pts',(-38.581465149306,3.84514777132169,-0.857030507547004));
#47195=CARTESIAN_POINT('Ctrl Pts',(-38.6477563265385,3.56135525018452,-2.13029227659612));
#47196=CARTESIAN_POINT('Ctrl Pts',(-38.714047503771,2.58226809489474,-3.24858244282497));
#47197=CARTESIAN_POINT('Ctrl Pts',(-38.7803386810035,1.35767994975888,-3.69815735579074));
#47198=CARTESIAN_POINT('Ctrl Pts',(-38.846629858236,0.133091804623014,-4.14773226875652));
#47199=CARTESIAN_POINT('Ctrl Pts',(-38.9129210354685,-1.33699733035893,
-3.92859192845923));
#47200=CARTESIAN_POINT('Ctrl Pts',(-38.979212212701,-2.3772269973294,-3.14140963220887));
#47201=CARTESIAN_POINT('Ctrl Pts',(-39.0404203011223,-3.33769371541464,
-2.41458706540369));
#47202=CARTESIAN_POINT('Ctrl Pts',(-39.1016283895437,-3.93169529530333,
-1.20349559357064));
#47203=CARTESIAN_POINT('Ctrl Pts',(-39.1628364779651,-3.93851028872272,
0.00178997264115022));
#47204=CARTESIAN_POINT('Ctrl Pts',(-39.3461635220348,-3.93809135854538,
0.00211875562057622));
#47205=CARTESIAN_POINT('Ctrl Pts',(-39.2860322743903,-3.93039708158953,
-1.18229485151587));
#47206=CARTESIAN_POINT('Ctrl Pts',(-39.2259010267458,-3.35977318684557,
-2.37313214528199));
#47207=CARTESIAN_POINT('Ctrl Pts',(-39.1657697791014,-2.42792273491924,
-3.10239486001197));
#47208=CARTESIAN_POINT('Ctrl Pts',(-39.0994786018689,-1.4006122119768,-3.90636427300412));
#47209=CARTESIAN_POINT('Ctrl Pts',(-39.0331874246364,0.0657247801994387,
-4.14934653349288));
#47210=CARTESIAN_POINT('Ctrl Pts',(-38.9668962474039,1.29745152200931,-3.71971534155534));
#47211=CARTESIAN_POINT('Ctrl Pts',(-38.9006050701714,2.52917826381926,-3.29008414961777));
#47212=CARTESIAN_POINT('Ctrl Pts',(-38.834313892939,3.52629475526267,-2.18783950525372));
#47213=CARTESIAN_POINT('Ctrl Pts',(-38.7680227157065,3.83072465649444,-0.91935372968844));
#47214=CARTESIAN_POINT('Ctrl Pts',(-38.701731538474,4.1351545577262,0.349132045876837));
#47215=CARTESIAN_POINT('Ctrl Pts',(-38.6354403612415,3.74689786874632,1.78385895264344));
#47216=CARTESIAN_POINT('Ctrl Pts',(-38.569149184009,2.84432011107059,2.7257119767));
#47217=CARTESIAN_POINT('Ctrl Pts',(-38.5028580067765,1.94174235339486,3.66756500075656));
#47218=CARTESIAN_POINT('Ctrl Pts',(-38.4365668295441,0.524843527023436,
4.1165441421031));
#47219=CARTESIAN_POINT('Ctrl Pts',(-38.3702756523116,-0.755451592569169,
3.86638792226687));
#47220=CARTESIAN_POINT('Ctrl Pts',(-38.3039844750791,-2.03574671216185,
3.61623170243063));
#47221=CARTESIAN_POINT('Ctrl Pts',(-38.2376932978466,-3.17943812497561,
2.66694012141135));
#47222=CARTESIAN_POINT('Ctrl Pts',(-38.1714021206141,-3.66111282180858,
1.45461870610661));
#47223=CARTESIAN_POINT('Ctrl Pts',(-38.1463225877544,-3.84334184369755,
0.99596861055748));
#47224=CARTESIAN_POINT('Ctrl Pts',(-38.1212430548946,-3.93081712177783,
0.499671336424599));
#47225=CARTESIAN_POINT('Ctrl Pts',(-38.0961635220348,-3.9280248704326,0.00242793667101629));
#47226=CARTESIAN_POINT('Origin',(-54.75,0.,0.));
#47227=CARTESIAN_POINT('',(-36.6628364779652,-3.92871471926708,-0.00281959343416821));
#47228=CARTESIAN_POINT('',(-36.8461635220348,-3.92920254662071,-0.00303214147515514));
#47229=CARTESIAN_POINT('',(-54.75,-3.933,-4.81653586104654E-16));
#47230=CARTESIAN_POINT('Ctrl Pts',(-36.6628364779652,-3.92871471926708,
-0.00281959343416821));
#47231=CARTESIAN_POINT('Ctrl Pts',(-36.7057587733198,-3.92310430500018,
0.847811380770198));
#47232=CARTESIAN_POINT('Ctrl Pts',(-36.7486810686744,-3.65202702481909,
1.70169988563318));
#47233=CARTESIAN_POINT('Ctrl Pts',(-36.791603364029,-3.14270982152566,2.37550787240382));
#47234=CARTESIAN_POINT('Ctrl Pts',(-36.8578945412614,-2.35609678715395,
3.41616807714502));
#47235=CARTESIAN_POINT('Ctrl Pts',(-36.9241857184939,-1.00120669152006,
4.02727967275646));
#47236=CARTESIAN_POINT('Ctrl Pts',(-36.9904768957264,0.299522564462462,
3.92809736482489));
#47237=CARTESIAN_POINT('Ctrl Pts',(-37.0567680729589,1.60025182044498,3.82891505689333));
#47238=CARTESIAN_POINT('Ctrl Pts',(-37.1230592501914,2.84682023677614,3.01943884541876));
#47239=CARTESIAN_POINT('Ctrl Pts',(-37.1893504274239,3.46655300322102,1.87154293299026));
#47240=CARTESIAN_POINT('Ctrl Pts',(-37.2556416046563,4.0862857696659,0.72364702056176));
#47241=CARTESIAN_POINT('Ctrl Pts',(-37.3219327818888,4.0791828862245,-0.762668592820669));
#47242=CARTESIAN_POINT('Ctrl Pts',(-37.3882239591213,3.44850742484189,-1.9045889884636));
#47243=CARTESIAN_POINT('Ctrl Pts',(-37.4545151363538,2.81783196345931,-3.04650938410646));
#47244=CARTESIAN_POINT('Ctrl Pts',(-37.5208063135863,1.56358392413559,-3.84403456200987));
#47245=CARTESIAN_POINT('Ctrl Pts',(-37.5870974908188,0.261966143792537,
-3.93078063667676));
#47246=CARTESIAN_POINT('Ctrl Pts',(-37.6533886680512,-1.03965163655066,
-4.01752671134365));
#47247=CARTESIAN_POINT('Ctrl Pts',(-37.7196798452837,-2.3886391579132,-3.39349368277382));
#47248=CARTESIAN_POINT('Ctrl Pts',(-37.7859710225162,-3.16527016806154,
-2.34536296494725));
#47249=CARTESIAN_POINT('Ctrl Pts',(-37.8282595076659,-3.66069882554678,
-1.67673914280205));
#47250=CARTESIAN_POINT('Ctrl Pts',(-37.8705479928155,-3.92321143043598,
-0.835532048235915));
#47251=CARTESIAN_POINT('Ctrl Pts',(-37.9128364779651,-3.92844641092988,
0.00268183597320199));
#47252=CARTESIAN_POINT('Ctrl Pts',(-38.0961635220348,-3.9280248704326,0.00242793667101629));
#47253=CARTESIAN_POINT('Ctrl Pts',(-38.0549518776621,-3.92343653658755,
-0.814661371646528));
#47254=CARTESIAN_POINT('Ctrl Pts',(-38.0137402332894,-3.67510497528553,
-1.63430543817939));
#47255=CARTESIAN_POINT('Ctrl Pts',(-37.9725285889167,-3.2029360731075,-2.29365716395305));
#47256=CARTESIAN_POINT('Ctrl Pts',(-37.9062374116842,-2.44342664672121,
-3.35426036911786));
#47257=CARTESIAN_POINT('Ctrl Pts',(-37.8399462344517,-1.10474981309637,
-4.00011552985729));
#47258=CARTESIAN_POINT('Ctrl Pts',(-37.7736550572192,0.198104916065548,
-3.93451612226931));
#47259=CARTESIAN_POINT('Ctrl Pts',(-37.7073638799867,1.50095964522754,-3.86891671468132));
#47260=CARTESIAN_POINT('Ctrl Pts',(-37.6410727027542,2.76799226992662,-3.09186273876585));
#47261=CARTESIAN_POINT('Ctrl Pts',(-37.5747815255217,3.41712670159429,-1.96033358881028));
#47262=CARTESIAN_POINT('Ctrl Pts',(-37.5084903482892,4.06626113326188,-0.828804438854842));
#47263=CARTESIAN_POINT('Ctrl Pts',(-37.4421991710568,4.09749737189823,0.65719988514059));
#47264=CARTESIAN_POINT('Ctrl Pts',(-37.3759079938243,3.49648545740553,1.81500747114662));
#47265=CARTESIAN_POINT('Ctrl Pts',(-37.3096168165918,2.8954735429128,2.97281505715271));
#47266=CARTESIAN_POINT('Ctrl Pts',(-37.2433256393593,1.66221347529096,3.80242590516937));
#47267=CARTESIAN_POINT('Ctrl Pts',(-37.1770344621268,0.363266195714995,
3.92271593990913));
#47268=CARTESIAN_POINT('Ctrl Pts',(-37.1107432848943,-0.935681083860891,
4.04300597464889));
#47269=CARTESIAN_POINT('Ctrl Pts',(-37.0444521076619,-2.30031557539088,
3.45397519611184));
#47270=CARTESIAN_POINT('Ctrl Pts',(-36.9781609304294,-3.10372279248287,
2.42622494867826));
#47271=CARTESIAN_POINT('Ctrl Pts',(-36.9341617942979,-3.63696454484935,
1.74408103550773));
#47272=CARTESIAN_POINT('Ctrl Pts',(-36.8901626581663,-3.92296807898683,
0.868667435112945));
#47273=CARTESIAN_POINT('Ctrl Pts',(-36.8461635220348,-3.92920254662071,
-0.00303214147515514));
#47274=CARTESIAN_POINT('Origin',(-54.75,0.,0.));
#47275=CARTESIAN_POINT('',(-35.4128364779651,-3.93872791654916,-0.00158551424731923));
#47276=CARTESIAN_POINT('',(-35.5961635220348,-3.93904295656044,-0.00122215278806678));
#47277=CARTESIAN_POINT('',(-54.75,-3.933,-4.81653586104654E-16));
#47278=CARTESIAN_POINT('Ctrl Pts',(-35.4128364779651,-3.93872791654916,
-0.00158551424731923));
#47279=CARTESIAN_POINT('Ctrl Pts',(-35.4746783765915,-3.93251546723464,
1.21600245087171));
#47280=CARTESIAN_POINT('Ctrl Pts',(-35.5365202752179,-3.32448100290972,
2.43894589304352));
#47281=CARTESIAN_POINT('Ctrl Pts',(-35.5983621738442,-2.34709443789658,
3.16398646864385));
#47282=CARTESIAN_POINT('Ctrl Pts',(-35.6646533510767,-1.29938879746337,
3.94119082952965));
#47283=CARTESIAN_POINT('Ctrl Pts',(-35.7309445283092,0.172727623926127,
4.14627080274248));
#47284=CARTESIAN_POINT('Ctrl Pts',(-35.7972357055417,1.39296303095743,3.68501243804582));
#47285=CARTESIAN_POINT('Ctrl Pts',(-35.8635268827742,2.61319843798872,3.22375407334915));
#47286=CARTESIAN_POINT('Ctrl Pts',(-35.9298180600067,3.58155283066183,2.09615737074299));
#47287=CARTESIAN_POINT('Ctrl Pts',(-35.9961092372392,3.85316320683496,0.820241413036307));
#47288=CARTESIAN_POINT('Ctrl Pts',(-36.0624004144716,4.12477358300807,-0.455674544670307));
#47289=CARTESIAN_POINT('Ctrl Pts',(-36.1286915917041,3.69963994268129,-1.87990975747744));
#47290=CARTESIAN_POINT('Ctrl Pts',(-36.1949827689366,2.77306911667835,-2.79816910645));
#47291=CARTESIAN_POINT('Ctrl Pts',(-36.2612739461691,1.84649829067536,-3.71642845542261));
#47292=CARTESIAN_POINT('Ctrl Pts',(-36.3275651234016,0.418490278996138,
-4.1287119405606));
#47293=CARTESIAN_POINT('Ctrl Pts',(-36.393856300634,-0.854926571749036,
-3.84561610552638));
#47294=CARTESIAN_POINT('Ctrl Pts',(-36.4601474778665,-2.12834342249421,
-3.56252027049216));
#47295=CARTESIAN_POINT('Ctrl Pts',(-36.526438655099,-3.24716911230534,-2.58404511528574));
#47296=CARTESIAN_POINT('Ctrl Pts',(-36.5927298323315,-3.69741397065613,
-1.35970313074704));
#47297=CARTESIAN_POINT('Ctrl Pts',(-36.6160987142094,-3.85613371814269,
-0.928099644290867));
#47298=CARTESIAN_POINT('Ctrl Pts',(-36.6394675960873,-3.93176928816201,
-0.465942420245586));
#47299=CARTESIAN_POINT('Ctrl Pts',(-36.6628364779652,-3.92871471926708,
-0.00281959343416821));
#47300=CARTESIAN_POINT('Ctrl Pts',(-36.8461635220348,-3.92920254662071,
-0.00303214147515514));
#47301=CARTESIAN_POINT('Ctrl Pts',(-36.8238714809338,-3.93236122247111,
-0.444676330372303));
#47302=CARTESIAN_POINT('Ctrl Pts',(-36.8015794398329,-3.86370557634453,
-0.885367161184453));
#47303=CARTESIAN_POINT('Ctrl Pts',(-36.7792873987319,-3.7190049061588,-1.29948650709933));
#47304=CARTESIAN_POINT('Ctrl Pts',(-36.7129962214994,-3.28869986008875,
-2.53097799911303));
#47305=CARTESIAN_POINT('Ctrl Pts',(-36.646705044267,-2.18590982529467,-3.52749126681019));
#47306=CARTESIAN_POINT('Ctrl Pts',(-36.5804138670345,-0.917257675925253,
-3.83122709195405));
#47307=CARTESIAN_POINT('Ctrl Pts',(-36.514122689802,0.35139447344417,-4.13496291709791));
#47308=CARTESIAN_POINT('Ctrl Pts',(-36.4478315125695,1.78590873738895,-3.74592129968847));
#47309=CARTESIAN_POINT('Ctrl Pts',(-36.381540335337,2.72726779032845,-2.84282835816787));
#47310=CARTESIAN_POINT('Ctrl Pts',(-36.3152491581045,3.668626843268,-1.93973541664722));
#47311=CARTESIAN_POINT('Ctrl Pts',(-36.2489579808721,4.11683068520223,-0.522591151015356));
#47312=CARTESIAN_POINT('Ctrl Pts',(-36.1826668036396,3.86597401100417,0.757566908204662));
#47313=CARTESIAN_POINT('Ctrl Pts',(-36.1163756264071,3.61511733680615,2.03772496742454));
#47314=CARTESIAN_POINT('Ctrl Pts',(-36.0500844491746,2.66520014647603,3.1808968202326));
#47315=CARTESIAN_POINT('Ctrl Pts',(-35.9837932719421,1.4526153724709,3.66190814382716));
#47316=CARTESIAN_POINT('Ctrl Pts',(-35.9175020947096,0.240030598465757,
4.14291946742173));
#47317=CARTESIAN_POINT('Ctrl Pts',(-35.8512109174772,-1.23522175921441,
3.96177026180279));
#47318=CARTESIAN_POINT('Ctrl Pts',(-35.7849197402447,-2.2954092529038,3.20168065800605));
#47319=CARTESIAN_POINT('Ctrl Pts',(-35.7220010008414,-3.3016617199574,2.48025917024576));
#47320=CARTESIAN_POINT('Ctrl Pts',(-35.6590822614381,-3.93400637947865,
1.23730393257168));
#47321=CARTESIAN_POINT('Ctrl Pts',(-35.5961635220348,-3.93904295656044,
-0.00122215278806678));
#47322=CARTESIAN_POINT('Origin',(-54.75,0.,0.));
#47323=CARTESIAN_POINT('',(-34.1628364779651,-3.93357436621185,0.00359891632991313));
#47324=CARTESIAN_POINT('',(-34.3461635220348,-3.93292354923884,0.0036330978440403));
#47325=CARTESIAN_POINT('',(-54.75,-3.933,-4.81653586104654E-16));
#47326=CARTESIAN_POINT('Ctrl Pts',(-34.1628364779651,-3.93357436621185,
0.00359891632991313));
#47327=CARTESIAN_POINT('Ctrl Pts',(-34.1773068026308,-3.9362323744975,0.289473138192191));
#47328=CARTESIAN_POINT('Ctrl Pts',(-34.1917771272964,-3.90772657673974,
0.574821677658488));
#47329=CARTESIAN_POINT('Ctrl Pts',(-34.206247451962,-3.84608328852811,0.852822380024853));
#47330=CARTESIAN_POINT('Ctrl Pts',(-34.2725386291945,-3.5636842243429,2.1263939312628));
#47331=CARTESIAN_POINT('Ctrl Pts',(-34.338829806427,-2.58582136213101,3.24575480973049));
#47332=CARTESIAN_POINT('Ctrl Pts',(-34.4051209836595,-1.361725904702,3.69666947868347));
#47333=CARTESIAN_POINT('Ctrl Pts',(-34.471412160892,-0.137630447272919,
4.14758414763648));
#47334=CARTESIAN_POINT('Ctrl Pts',(-34.5377033381245,1.33269760537326,3.93005260707466));
#47335=CARTESIAN_POINT('Ctrl Pts',(-34.6039945153569,2.37378803635881,3.14400907005788));
#47336=CARTESIAN_POINT('Ctrl Pts',(-34.6702856925894,3.41487846734437,2.35796553304111));
#47337=CARTESIAN_POINT('Ctrl Pts',(-34.7365768698219,4.02673127666927,1.0034099995692));
#47338=CARTESIAN_POINT('Ctrl Pts',(-34.8028680470544,3.92826065557925,-0.297373327644713));
#47339=CARTESIAN_POINT('Ctrl Pts',(-34.8691592242869,3.82979003448924,-1.59815665485862));
#47340=CARTESIAN_POINT('Ctrl Pts',(-34.9354504015194,3.02099598298444,-2.84516777581461));
#47341=CARTESIAN_POINT('Ctrl Pts',(-35.0017415787519,1.87343931866343,-3.46552850131871));
#47342=CARTESIAN_POINT('Ctrl Pts',(-35.0680327559843,0.725882654342432,
-4.08588922682282));
#47343=CARTESIAN_POINT('Ctrl Pts',(-35.1343239332168,-0.760436622794699,
-4.07959955687498));
#47344=CARTESIAN_POINT('Ctrl Pts',(-35.2006151104493,-1.90270191092192,
-3.44954897230645));
#47345=CARTESIAN_POINT('Ctrl Pts',(-35.2669062876818,-3.04496719904915,
-2.81949838773792));
#47346=CARTESIAN_POINT('Ctrl Pts',(-35.3331974649143,-3.8431784981664,-1.56568688854873));
#47347=CARTESIAN_POINT('Ctrl Pts',(-35.3994886421468,-3.93063671798657,
-0.264116764674724));
#47348=CARTESIAN_POINT('Ctrl Pts',(-35.4039379207529,-3.93650666935296,
-0.176759014393482));
#47349=CARTESIAN_POINT('Ctrl Pts',(-35.408387199359,-3.93917487756493,-0.0891861249111568));
#47350=CARTESIAN_POINT('Ctrl Pts',(-35.4128364779651,-3.93872791654916,
-0.00158551424731923));
#47351=CARTESIAN_POINT('Ctrl Pts',(-35.5961635220348,-3.93904295656044,
-0.00122215278806678));
#47352=CARTESIAN_POINT('Ctrl Pts',(-35.5927910842056,-3.93931291656347,
-0.0676070209899404));
#47353=CARTESIAN_POINT('Ctrl Pts',(-35.5894186463764,-3.93778065259506,
-0.133979164464208));
#47354=CARTESIAN_POINT('Ctrl Pts',(-35.5860462085472,-3.93440714360982,
-0.200257590314247));
#47355=CARTESIAN_POINT('Ctrl Pts',(-35.5197550313147,-3.8680949109277,-1.50307623286285));
#47356=CARTESIAN_POINT('Ctrl Pts',(-35.4534638540823,-3.0903478158649,-2.76968351598535));
#47357=CARTESIAN_POINT('Ctrl Pts',(-35.3871726768498,-1.95846367235667,
-3.41819875347027));
#47358=CARTESIAN_POINT('Ctrl Pts',(-35.3208814996173,-0.826579528848437,
-4.06671399095518));
#47359=CARTESIAN_POINT('Ctrl Pts',(-35.2545903223848,0.659441663105231,
-4.09713718280251));
#47360=CARTESIAN_POINT('Ctrl Pts',(-35.1882991451523,1.81692024231754,-3.49549188344405));
#47361=CARTESIAN_POINT('Ctrl Pts',(-35.1220079679198,2.97439882152978,-2.89384658408562));
#47362=CARTESIAN_POINT('Ctrl Pts',(-35.0557167906874,3.80333478800069,-1.66013279352146));
#47363=CARTESIAN_POINT('Ctrl Pts',(-34.9894256134549,3.92291410771786,-0.361119893712047));
#47364=CARTESIAN_POINT('Ctrl Pts',(-34.9231344362224,4.04249342743504,0.937893006097444));
#47365=CARTESIAN_POINT('Ctrl Pts',(-34.8568432589899,3.45271610039835,2.30220501515221));
#47366=CARTESIAN_POINT('Ctrl Pts',(-34.7905520817574,2.42452643613527,3.10504979584027));
#47367=CARTESIAN_POINT('Ctrl Pts',(-34.7242609045249,1.39633677187219,3.90789457652833));
#47368=CARTESIAN_POINT('Ctrl Pts',(-34.6579697272925,-0.0702652296172822,
4.14927212884968));
#47369=CARTESIAN_POINT('Ctrl Pts',(-34.59167855006,-1.30152110318205,3.71829335746095));
#47370=CARTESIAN_POINT('Ctrl Pts',(-34.5253873728275,-2.53277697674682,
3.28731458607222));
#47371=CARTESIAN_POINT('Ctrl Pts',(-34.459096195595,-3.52868672238688,2.1839794909734));
#47372=CARTESIAN_POINT('Ctrl Pts',(-34.3928050183625,-3.83172838051812,
0.915161347576742));
#47373=CARTESIAN_POINT('Ctrl Pts',(-34.3772578529199,-3.90280026355969,
0.617587425744959));
#47374=CARTESIAN_POINT('Ctrl Pts',(-34.3617106874774,-3.93576191957382,
0.310911343410304));
#47375=CARTESIAN_POINT('Ctrl Pts',(-34.3461635220348,-3.93292354923884,
0.0036330978440403));
#47376=CARTESIAN_POINT('Origin',(-54.75,0.,0.));
#47377=CARTESIAN_POINT('',(-32.9128364779652,-3.9264796012353,-8.02974850103166E-5));
#47378=CARTESIAN_POINT('',(-33.0961635220348,-3.92652099442121,-0.000433216618794752));
#47379=CARTESIAN_POINT('',(-54.75,-3.933,-4.81653586104654E-16));
#47380=CARTESIAN_POINT('Ctrl Pts',(-32.9128364779652,-3.9264796012353,-8.02974850103167E-5));
#47381=CARTESIAN_POINT('Ctrl Pts',(-32.9462264059025,-3.92635941678331,
0.662581741630279));
#47382=CARTESIAN_POINT('Ctrl Pts',(-32.9796163338399,-3.76762221461801,
1.32529785623839));
#47383=CARTESIAN_POINT('Ctrl Pts',(-33.0130062617773,-3.45058948713258,
1.90081426379763));
#47384=CARTESIAN_POINT('Ctrl Pts',(-33.0792974390098,-2.82116396798668,
3.04342410246678));
#47385=CARTESIAN_POINT('Ctrl Pts',(-33.1455886162423,-1.56778938426622,
3.84232128384968));
#47386=CARTESIAN_POINT('Ctrl Pts',(-33.2118797934748,-0.266267306492336,
3.9304916226421));
#47387=CARTESIAN_POINT('Ctrl Pts',(-33.2781709707073,1.0352547712814,4.01866196143452));
#47388=CARTESIAN_POINT('Ctrl Pts',(-33.3444621479397,2.38492434310865,3.39610545763665));
#47389=CARTESIAN_POINT('Ctrl Pts',(-33.4107533251722,3.16270182207219,2.34882520823234));
#47390=CARTESIAN_POINT('Ctrl Pts',(-33.4770445024047,3.94047930103577,1.30154495882797));
#47391=CARTESIAN_POINT('Ctrl Pts',(-33.5433356796372,4.14636468713564,-0.170459036182738));
#47392=CARTESIAN_POINT('Ctrl Pts',(-33.6096268568697,3.68577402262817,-1.39094663027945));
#47393=CARTESIAN_POINT('Ctrl Pts',(-33.6759180341022,3.22518335812068,-2.61143422437624));
#47394=CARTESIAN_POINT('Ctrl Pts',(-33.7422092113346,2.09811664300563,-3.58040541755886));
#47395=CARTESIAN_POINT('Ctrl Pts',(-33.8085003885671,0.822349483294592,
-3.85271384889815));
#47396=CARTESIAN_POINT('Ctrl Pts',(-33.8747915657996,-0.453417676416301,
-4.1250222802374));
#47397=CARTESIAN_POINT('Ctrl Pts',(-33.9410827430321,-1.87788528072323,
-3.70066794973349));
#47398=CARTESIAN_POINT('Ctrl Pts',(-34.0073739202646,-2.79665144979747,
-2.77459967247749));
#47399=CARTESIAN_POINT('Ctrl Pts',(-34.0591947728315,-3.5148653687333,-2.05067758109228));
#47400=CARTESIAN_POINT('Ctrl Pts',(-34.1110156253983,-3.92405555729255,
-1.02016843140461));
#47401=CARTESIAN_POINT('Ctrl Pts',(-34.1628364779651,-3.93357436621185,
0.00359891632991313));
#47402=CARTESIAN_POINT('Ctrl Pts',(-34.3461635220348,-3.93292354923884,
0.0036330978440403));
#47403=CARTESIAN_POINT('Ctrl Pts',(-34.2954195102449,-3.92365946195074,
-0.999284827832049));
#47404=CARTESIAN_POINT('Ctrl Pts',(-34.244675498455,-3.53302188146874,-2.00861752797984));
#47405=CARTESIAN_POINT('Ctrl Pts',(-34.1939314866651,-2.84133575425134,
-2.72882278753667));
#47406=CARTESIAN_POINT('Ctrl Pts',(-34.1276403094326,-1.93772789923092,
-3.66968758755893));
#47407=CARTESIAN_POINT('Ctrl Pts',(-34.0613491322001,-0.520338618567738,
-4.11711599590891));
#47408=CARTESIAN_POINT('Ctrl Pts',(-33.9950579549676,0.759681997058345,
-3.8655589424444));
#47409=CARTESIAN_POINT('Ctrl Pts',(-33.9287667777351,2.03970261268443,-3.6140018889799));
#47410=CARTESIAN_POINT('Ctrl Pts',(-33.8624756005026,3.18235456327333,-2.66345937370094));
#47411=CARTESIAN_POINT('Ctrl Pts',(-33.7961844232701,3.66270236963661,-1.45061160398805));
#47412=CARTESIAN_POINT('Ctrl Pts',(-33.7298932460376,4.14305017599989,-0.237763834275166));
#47413=CARTESIAN_POINT('Ctrl Pts',(-33.6636020688052,3.96109383813746,1.23738918987177));
#47414=CARTESIAN_POINT('Ctrl Pts',(-33.5973108915727,3.20042428446631,2.29716065471372));
#47415=CARTESIAN_POINT('Ctrl Pts',(-33.5310197143402,2.4397547307952,3.35693211955562));
#47416=CARTESIAN_POINT('Ctrl Pts',(-33.4647285371077,1.10037196131553,4.00132202509275));
#47417=CARTESIAN_POINT('Ctrl Pts',(-33.3984373598752,-0.202410204614914,
3.93429698716736));
#47418=CARTESIAN_POINT('Ctrl Pts',(-33.3321461826427,-1.50519237054536,
3.86727194924197));
#47419=CARTESIAN_POINT('Ctrl Pts',(-33.2658550054103,-2.77137393292651,
3.08883196785406));
#47420=CARTESIAN_POINT('Ctrl Pts',(-33.1995638281778,-3.41926978209264,
1.9565931696279));
#47421=CARTESIAN_POINT('Ctrl Pts',(-33.1650970594635,-3.75613024100211,
1.36790830360129));
#47422=CARTESIAN_POINT('Ctrl Pts',(-33.1306302907491,-3.92585128094651,
0.683582009327261));
#47423=CARTESIAN_POINT('Ctrl Pts',(-33.0961635220348,-3.92652099442121,
-0.000433216618794752));
#47424=CARTESIAN_POINT('Origin',(-54.75,0.,0.));
#47425=CARTESIAN_POINT('',(-31.6628364779652,-3.93387008195027,-0.00357098358684305));
#47426=CARTESIAN_POINT('',(-31.8461635220348,-3.9345187971462,-0.00348206949214982));
#47427=CARTESIAN_POINT('',(-54.75,-3.933,-4.81653586104654E-16));
#47428=CARTESIAN_POINT('Ctrl Pts',(-31.6628364779652,-3.93387008195027,
-0.00357098358684305));
#47429=CARTESIAN_POINT('Ctrl Pts',(-31.7151460091743,-3.9242645441804,1.02965144060316));
#47430=CARTESIAN_POINT('Ctrl Pts',(-31.7674555403835,-3.50648141256207,
2.06974646053407));
#47431=CARTESIAN_POINT('Ctrl Pts',(-31.8197650715926,-2.77612939768722,
2.79513295595455));
#47432=CARTESIAN_POINT('Ctrl Pts',(-31.8860562488251,-1.85056394640085,
3.71440567009357));
#47433=CARTESIAN_POINT('Ctrl Pts',(-31.9523474260576,-0.42300793747674,
4.1282515289858));
#47434=CARTESIAN_POINT('Ctrl Pts',(-32.0186386032901,0.850717933004561,
3.84654932018698));
#47435=CARTESIAN_POINT('Ctrl Pts',(-32.0849297805226,2.12444380348579,3.56484711138817));
#47436=CARTESIAN_POINT('Ctrl Pts',(-32.151220957755,3.24433953552423,2.58759683489839));
#47437=CARTESIAN_POINT('Ctrl Pts',(-32.2175121349875,3.69592388009588,1.36374827101759));
#47438=CARTESIAN_POINT('Ctrl Pts',(-32.28380331222,4.14750822466752,0.139899707136798));
#47439=CARTESIAN_POINT('Ctrl Pts',(-32.3500944894525,3.93078118177237,-1.33054714413501));
#47440=CARTESIAN_POINT('Ctrl Pts',(-32.416385666685,3.14530737741631,-2.37206748970955));
#47441=CARTESIAN_POINT('Ctrl Pts',(-32.4826768439175,2.35983357306016,-3.4135878352842));
#47442=CARTESIAN_POINT('Ctrl Pts',(-32.5489680211499,1.00561300724294,-4.02618167516146));
#47443=CARTESIAN_POINT('Ctrl Pts',(-32.6152591983824,-0.29522400180688,
-3.92842277039063));
#47444=CARTESIAN_POINT('Ctrl Pts',(-32.6815503756149,-1.59606101085663,
-3.8306638656198));
#47445=CARTESIAN_POINT('Ctrl Pts',(-32.7478415528474,-2.84351446313897,
-3.02255221620097));
#47446=CARTESIAN_POINT('Ctrl Pts',(-32.8141327300799,-3.46450296199443,
-1.87533514351389));
#47447=CARTESIAN_POINT('Ctrl Pts',(-32.847033979375,-3.77270834109907,-1.30595507696754));
#47448=CARTESIAN_POINT('Ctrl Pts',(-32.8799352286701,-3.92659802672648,
-0.653043939341669));
#47449=CARTESIAN_POINT('Ctrl Pts',(-32.9128364779652,-3.9264796012353,-8.02974850103167E-5));
#47450=CARTESIAN_POINT('Ctrl Pts',(-33.0961635220348,-3.92652099442121,
-0.000433216618794752));
#47451=CARTESIAN_POINT('Ctrl Pts',(-33.0643391135166,-3.9271393649852,-0.632009102469086));
#47452=CARTESIAN_POINT('Ctrl Pts',(-33.0325147049985,-3.78363313240224,
-1.26331978720999));
#47453=CARTESIAN_POINT('Ctrl Pts',(-33.0006902964803,-3.49449726309091,
-1.81883246958498));
#47454=CARTESIAN_POINT('Ctrl Pts',(-32.9343991192478,-2.89221875897201,
-2.97598169550694));
#47455=CARTESIAN_POINT('Ctrl Pts',(-32.8681079420153,-1.65805161478326,
-3.80424253228636));
#47456=CARTESIAN_POINT('Ctrl Pts',(-32.8018167647829,-0.358973483605743,
-3.92311110118416));
#47457=CARTESIAN_POINT('Ctrl Pts',(-32.7355255875504,0.940104647571701,
-4.04197967008195));
#47458=CARTESIAN_POINT('Ctrl Pts',(-32.6692344103179,2.30409376573791,-3.4514559710982));
#47459=CARTESIAN_POINT('Ctrl Pts',(-32.6029432330854,3.10637586968665,-2.42282719779908));
#47460=CARTESIAN_POINT('Ctrl Pts',(-32.5366520558529,3.90865797363544,-1.3941984244999));
#47461=CARTESIAN_POINT('Ctrl Pts',(-32.4703608786204,4.14923306336671,0.0725354231147142));
#47462=CARTESIAN_POINT('Ctrl Pts',(-32.4040697013879,3.71758069567479,1.30355530964841));
#47463=CARTESIAN_POINT('Ctrl Pts',(-32.3377785241555,3.28592832798287,2.53457519618211));
#47464=CARTESIAN_POINT('Ctrl Pts',(-32.271487346923,2.18204850286777,3.5298811216349));
#47465=CARTESIAN_POINT('Ctrl Pts',(-32.2051961696905,0.913064745270451,
3.83222852203658));
#47466=CARTESIAN_POINT('Ctrl Pts',(-32.138904992458,-0.355919012326873,
4.13457592243826));
#47467=CARTESIAN_POINT('Ctrl Pts',(-32.0726138152255,-1.79000670240642,
3.74396479778884));
#47468=CARTESIAN_POINT('Ctrl Pts',(-32.006322637993,-2.73037696785918,2.83984229976781));
#47469=CARTESIAN_POINT('Ctrl Pts',(-31.952936266007,-3.48768674710849,2.11172398877361));
#47470=CARTESIAN_POINT('Ctrl Pts',(-31.8995498940209,-3.92479174814375,
1.05056336001));
#47471=CARTESIAN_POINT('Ctrl Pts',(-31.8461635220348,-3.9345187971462,-0.00348206949214982));
#47472=CARTESIAN_POINT('Origin',(-54.75,0.,0.));
#47473=CARTESIAN_POINT('',(-30.4128364779652,-3.93856210802547,0.00174382912284086));
#47474=CARTESIAN_POINT('',(-30.5961635220348,-3.93815120456093,0.00207590725787368));
#47475=CARTESIAN_POINT('',(-54.75,-3.933,-4.81653586104654E-16));
#47476=CARTESIAN_POINT('Ctrl Pts',(-30.4128364779652,-3.93856210802547,
0.00174382912284086));
#47477=CARTESIAN_POINT('Ctrl Pts',(-30.4177744352136,-3.93909995995488,
0.0989767503555888));
#47478=CARTESIAN_POINT('Ctrl Pts',(-30.422712392462,-3.93581264589787,0.196172692623262));
#47479=CARTESIAN_POINT('Ctrl Pts',(-30.4276503497104,-3.92858370921048,
0.29307458759238));
#47480=CARTESIAN_POINT('Ctrl Pts',(-30.4939415269429,-3.83153655002342,
1.59396488906649));
#47481=CARTESIAN_POINT('Ctrl Pts',(-30.5602327041754,-3.02410754460245,
2.84186029924427));
#47482=CARTESIAN_POINT('Ctrl Pts',(-30.6265238814079,-1.8772304069739,3.46347638555528));
#47483=CARTESIAN_POINT('Ctrl Pts',(-30.6928150586404,-0.73035326934548,
4.08509247186621));
#47484=CARTESIAN_POINT('Ctrl Pts',(-30.7591062358729,0.755972000490423,
4.08042923431056));
#47485=CARTESIAN_POINT('Ctrl Pts',(-30.8253974131053,1.8989260476558,3.4516289690088));
#47486=CARTESIAN_POINT('Ctrl Pts',(-30.8916885903378,3.04188009482125,2.82282870370701));
#47487=CARTESIAN_POINT('Ctrl Pts',(-30.9579797675703,3.84146291931614,1.56989141065905));
#47488=CARTESIAN_POINT('Ctrl Pts',(-31.0242709448028,3.93034535068678,0.268417768602042));
#47489=CARTESIAN_POINT('Ctrl Pts',(-31.0905621220353,4.01922778205741,-1.03305587345496));
#47490=CARTESIAN_POINT('Ctrl Pts',(-31.1568532992678,3.39740982030379,-2.38306586452101));
#47491=CARTESIAN_POINT('Ctrl Pts',(-31.2231444765002,2.35055527543642,-3.16141622873111));
#47492=CARTESIAN_POINT('Ctrl Pts',(-31.2894356537327,1.30370073056905,-3.93976659294122));
#47493=CARTESIAN_POINT('Ctrl Pts',(-31.3557268309652,-0.168190397412086,
-4.14645733029538));
#47494=CARTESIAN_POINT('Ctrl Pts',(-31.4220180081977,-1.3889298132156,-3.68653450385688));
#47495=CARTESIAN_POINT('Ctrl Pts',(-31.4883091854302,-2.60966922901911,
-3.22661167741839));
#47496=CARTESIAN_POINT('Ctrl Pts',(-31.5546003626627,-3.57925693264501,
-2.10007528718724));
#47497=CARTESIAN_POINT('Ctrl Pts',(-31.6208915398952,-3.85226333763363,
-0.82445730737876));
#47498=CARTESIAN_POINT('Ctrl Pts',(-31.6348731859185,-3.90984383440576,
-0.555413374245061));
#47499=CARTESIAN_POINT('Ctrl Pts',(-31.6488548319418,-3.93643751518581,
-0.279737675669086));
#47500=CARTESIAN_POINT('Ctrl Pts',(-31.6628364779652,-3.93387008195027,
-0.00357098358684305));
#47501=CARTESIAN_POINT('Ctrl Pts',(-31.8461635220348,-3.9345187971462,-0.00348206949214982));
#47502=CARTESIAN_POINT('Ctrl Pts',(-31.8332587167884,-3.9368700652382,-0.258270894477957));
#47503=CARTESIAN_POINT('Ctrl Pts',(-31.820353911542,-3.91424928270523,-0.512643972429283));
#47504=CARTESIAN_POINT('Ctrl Pts',(-31.8074491062956,-3.86514271671165,
-0.761796858497929));
#47505=CARTESIAN_POINT('Ctrl Pts',(-31.7411579290631,-3.61288535928538,
-2.04167964735));
#47506=CARTESIAN_POINT('Ctrl Pts',(-31.6748667518306,-2.66171780360684,
-3.18381135366156));
#47507=CARTESIAN_POINT('Ctrl Pts',(-31.6085755745981,-1.44860740125792,
-3.66349549899918));
#47508=CARTESIAN_POINT('Ctrl Pts',(-31.5422843973656,-0.235496998908926,
-4.14317964433682));
#47509=CARTESIAN_POINT('Ctrl Pts',(-31.4759932201332,1.23955625011055,-3.96041622870047));
#47510=CARTESIAN_POINT('Ctrl Pts',(-31.4097020429007,2.29891136885762,-3.19916695286502));
#47511=CARTESIAN_POINT('Ctrl Pts',(-31.3434108656682,3.35826648760463,-2.43791767702961));
#47512=CARTESIAN_POINT('Ctrl Pts',(-31.2771196884357,4.00192347607932,-1.09818254099537));
#47513=CARTESIAN_POINT('Ctrl Pts',(-31.2108285112032,3.93418565297491,0.204562758323147));
#47514=CARTESIAN_POINT('Ctrl Pts',(-31.1445373339707,3.86644782987051,1.50730805764167));
#47515=CARTESIAN_POINT('Ctrl Pts',(-31.0782461567383,3.08731519518687,2.77306352024438));
#47516=CARTESIAN_POINT('Ctrl Pts',(-31.0119549795058,1.95472208118354,3.42033978714103));
#47517=CARTESIAN_POINT('Ctrl Pts',(-30.9456638022733,0.822128967180207,
4.06761605403768));
#47518=CARTESIAN_POINT('Ctrl Pts',(-30.8793726250408,-0.663924626142901,
4.09641312522832));
#47519=CARTESIAN_POINT('Ctrl Pts',(-30.8130814478083,-1.82074415237652,
3.49350159664385));
#47520=CARTESIAN_POINT('Ctrl Pts',(-30.7467902705758,-2.97756367861014,
2.89059006805938));
#47521=CARTESIAN_POINT('Ctrl Pts',(-30.6804990933433,-3.80514913775434,
1.65596993969977));
#47522=CARTESIAN_POINT('Ctrl Pts',(-30.6142079161109,-3.92330692024899,
0.35682696603929));
#47523=CARTESIAN_POINT('Ctrl Pts',(-30.6081931180855,-3.93402773147151,
0.238951814038115));
#47524=CARTESIAN_POINT('Ctrl Pts',(-30.6021783200602,-3.93890819421201,
0.120545479065067));
#47525=CARTESIAN_POINT('Ctrl Pts',(-30.5961635220348,-3.93815120456093,
0.00207590725787368));
#47526=CARTESIAN_POINT('Origin',(-54.75,0.,0.));
#47527=CARTESIAN_POINT('',(-29.1628364779652,-3.92850656573534,0.00271417295257592));
#47528=CARTESIAN_POINT('',(-29.3461635220348,-3.92807907470128,0.00246354187033206));
#47529=CARTESIAN_POINT('',(-54.75,-3.933,-4.81653586104654E-16));
#47530=CARTESIAN_POINT('Ctrl Pts',(-29.1628364779652,-3.92850656573534,
0.00271417295257592));
#47531=CARTESIAN_POINT('Ctrl Pts',(-29.1866940384854,-3.93149841301045,
0.475584504066331));
#47532=CARTESIAN_POINT('Ctrl Pts',(-29.2105515990055,-3.85257530886676,
0.94748964595665));
#47533=CARTESIAN_POINT('Ctrl Pts',(-29.2344091595257,-3.68729388150453,
1.38691258036898));
#47534=CARTESIAN_POINT('Ctrl Pts',(-29.3007003367582,-3.22803903081511,
2.60790345244531));
#47535=CARTESIAN_POINT('Ctrl Pts',(-29.3669915139907,-2.10203330270165,
3.57810737626403));
#47536=CARTESIAN_POINT('Ctrl Pts',(-29.4332826912232,-0.826564884657816,
3.85181167317628));
#47537=CARTESIAN_POINT('Ctrl Pts',(-29.4995738684556,0.448903533386023,
4.12551597008853));
#47538=CARTESIAN_POINT('Ctrl Pts',(-29.5658650456881,1.87383464136024,3.70272064009429));
#47539=CARTESIAN_POINT('Ctrl Pts',(-29.6321562229206,2.7936136253755,2.77765829184995));
#47540=CARTESIAN_POINT('Ctrl Pts',(-29.6984474001531,3.71339260939076,1.85259594360561));
#47541=CARTESIAN_POINT('Ctrl Pts',(-29.7647385773856,4.12801946944707,0.425266577111169));
#47542=CARTESIAN_POINT('Ctrl Pts',(-29.8310297546181,3.84701420036357,-0.848613231317707));
#47543=CARTESIAN_POINT('Ctrl Pts',(-29.8973209318506,3.56600893128009,-2.12249303974651));
#47544=CARTESIAN_POINT('Ctrl Pts',(-29.963612109083,2.58937153305671,-3.24292329010991));
#47545=CARTESIAN_POINT('Ctrl Pts',(-30.0299032863155,1.36577022908884,-3.69517717511638));
#47546=CARTESIAN_POINT('Ctrl Pts',(-30.096194463548,0.142168925120821,-4.1474310601229));
#47547=CARTESIAN_POINT('Ctrl Pts',(-30.1624856407805,-1.32839628459159,
-3.93150857977258));
#47548=CARTESIAN_POINT('Ctrl Pts',(-30.228776818013,-2.37034623297127,-3.14660474321217));
#47549=CARTESIAN_POINT('Ctrl Pts',(-30.2901300379971,-3.33468246992064,
-2.42016753450283));
#47550=CARTESIAN_POINT('Ctrl Pts',(-30.3514832579811,-3.93187939570464,
-1.20635751845283));
#47551=CARTESIAN_POINT('Ctrl Pts',(-30.4128364779652,-3.93856210802547,
0.00174382912284086));
#47552=CARTESIAN_POINT('Ctrl Pts',(-30.5961635220348,-3.93815120456093,
0.00207590725787368));
#47553=CARTESIAN_POINT('Ctrl Pts',(-30.5358871428277,-3.93056514845859,
-1.18514880164594));
#47554=CARTESIAN_POINT('Ctrl Pts',(-30.4756107636206,-3.35682441040137,
-2.37872422133875));
#47555=CARTESIAN_POINT('Ctrl Pts',(-30.4153343844134,-2.42112723417837,
-3.10770101362506));
#47556=CARTESIAN_POINT('Ctrl Pts',(-30.3490432071809,-1.39205965976785,
-3.90942020066774));
#47557=CARTESIAN_POINT('Ctrl Pts',(-30.2827520299484,0.0748055948983133,
-4.14919275579165));
#47558=CARTESIAN_POINT('Ctrl Pts',(-30.216460852716,1.30558912588946,-3.71686692101367));
#47559=CARTESIAN_POINT('Ctrl Pts',(-30.1501696754835,2.53637265688055,-3.28454108623571));
#47560=CARTESIAN_POINT('Ctrl Pts',(-30.083878498251,3.53107446419656,-2.18011686155598));
#47561=CARTESIAN_POINT('Ctrl Pts',(-30.0175873210185,3.83272751635967,-0.91096786963422));
#47562=CARTESIAN_POINT('Ctrl Pts',(-29.951296143786,4.13438056852279,0.358181122287614));
#47563=CARTESIAN_POINT('Ctrl Pts',(-29.8850049665535,3.74298486553277,1.79205488145162));
#47564=CARTESIAN_POINT('Ctrl Pts',(-29.818713789321,2.83834799516436,2.73193033083072));
#47565=CARTESIAN_POINT('Ctrl Pts',(-29.7524226120885,1.9337111247959,3.67180578020988));
#47566=CARTESIAN_POINT('Ctrl Pts',(-29.6861314348561,0.515833087049026,
4.11768291980425));
#47567=CARTESIAN_POINT('Ctrl Pts',(-29.6198402576236,-0.763911491890319,
3.86472533393052));
#47568=CARTESIAN_POINT('Ctrl Pts',(-29.5535490803911,-2.04365607082952,
3.61176774805681));
#47569=CARTESIAN_POINT('Ctrl Pts',(-29.4872579031586,-3.18526719096115,
2.6599754367152));
#47570=CARTESIAN_POINT('Ctrl Pts',(-29.4209667259261,-3.66428753167743,
1.44660276488046));
#47571=CARTESIAN_POINT('Ctrl Pts',(-29.396032324629,-3.84446362604685,0.990211395990211));
#47572=CARTESIAN_POINT('Ctrl Pts',(-29.3710979233319,-3.93089823856218,
0.496812372634598));
#47573=CARTESIAN_POINT('Ctrl Pts',(-29.3461635220348,-3.92807907470128,
0.00246354187033206));
#47574=CARTESIAN_POINT('Origin',(-54.75,0.,0.));
#47575=CARTESIAN_POINT('',(-27.9128364779652,-3.92865200925827,-0.00278885010489755));
#47576=CARTESIAN_POINT('',(-28.0961635220348,-3.92913455543446,-0.00300513829252201));
#47577=CARTESIAN_POINT('',(-54.75,-3.933,-4.81653586104654E-16));
#47578=CARTESIAN_POINT('Ctrl Pts',(-27.9128364779652,-3.92865200925827,
-0.00278885010489754));
#47579=CARTESIAN_POINT('Ctrl Pts',(-27.9556136417571,-3.92312711758811,
0.844999904541822));
#47580=CARTESIAN_POINT('Ctrl Pts',(-27.9983908055491,-3.65402535614722,
1.69598532263604));
#47581=CARTESIAN_POINT('Ctrl Pts',(-28.041167969341,-3.14790116705762,2.36862426665854));
#47582=CARTESIAN_POINT('Ctrl Pts',(-28.1074591465735,-2.36356753325771,
3.41100350593077));
#47583=CARTESIAN_POINT('Ctrl Pts',(-28.173750323806,-1.01001811882594,4.02507885654247));
#47584=CARTESIAN_POINT('Ctrl Pts',(-28.2400415010384,0.290925085644865,
3.92874347199063));
#47585=CARTESIAN_POINT('Ctrl Pts',(-28.3063326782709,1.59186829011552,3.83240808743879));
#47586=CARTESIAN_POINT('Ctrl Pts',(-28.3726238555034,2.84020528462515,3.02566196772358));
#47587=CARTESIAN_POINT('Ctrl Pts',(-28.4389150327359,3.46244877230814,1.87912510847689));
#47588=CARTESIAN_POINT('Ctrl Pts',(-28.5052062099684,4.08469225999124,0.732588249230013));
#47589=CARTESIAN_POINT('Ctrl Pts',(-28.5714973872008,4.08084224084741,-0.753739349548403));
#47590=CARTESIAN_POINT('Ctrl Pts',(-28.6377885644333,3.45266741762393,-1.89703726306168));
#47591=CARTESIAN_POINT('Ctrl Pts',(-28.7040797416658,2.82449259440052,-3.04033517657484));
#47592=CARTESIAN_POINT('Ctrl Pts',(-28.7703709188983,1.5719929670974,-3.84060340482301));
#47593=CARTESIAN_POINT('Ctrl Pts',(-28.8366620961308,0.270568150359426,
-3.93019790216441));
#47594=CARTESIAN_POINT('Ctrl Pts',(-28.9029532733633,-1.03085666637862,
-4.01979239950582));
#47595=CARTESIAN_POINT('Ctrl Pts',(-28.9692444505958,-2.38120667255164,
-3.39871316594053));
#47596=CARTESIAN_POINT('Ctrl Pts',(-29.0355356278283,-3.16012968900548,
-2.35228463899091));
#47597=CARTESIAN_POINT('Ctrl Pts',(-29.0779692445406,-3.65872576330176,
-1.68245572837013));
#47598=CARTESIAN_POINT('Ctrl Pts',(-29.1204028612529,-3.92318519599903,
-0.838344088982128));
#47599=CARTESIAN_POINT('Ctrl Pts',(-29.1628364779652,-3.92850656573534,
0.00271417295257592));
#47600=CARTESIAN_POINT('Ctrl Pts',(-29.3461635220348,-3.92807907470128,
0.00246354187033206));
#47601=CARTESIAN_POINT('Ctrl Pts',(-29.3048067460994,-3.92340314417738,
-0.81747488713848));
#47602=CARTESIAN_POINT('Ctrl Pts',(-29.2634499701641,-3.67318732149573,
-1.64002626562861));
#47603=CARTESIAN_POINT('Ctrl Pts',(-29.2220931942287,-3.19790866357844,
-2.30066139481159));
#47604=CARTESIAN_POINT('Ctrl Pts',(-29.1558020169962,-2.43607989346235,
-3.35959985034084));
#47605=CARTESIAN_POINT('Ctrl Pts',(-29.0895108397637,-1.09599279192933,
-4.00252372907152));
#47606=CARTESIAN_POINT('Ctrl Pts',(-29.0232196625312,0.206715250794351,
-3.93407314106582));
#47607=CARTESIAN_POINT('Ctrl Pts',(-28.9569284852988,1.50942329351825,-3.8656225530601));
#47608=CARTESIAN_POINT('Ctrl Pts',(-28.8906373080663,2.7747522774328,-3.08579749831771));
#47609=CARTESIAN_POINT('Ctrl Pts',(-28.8243461308338,3.42140876829489,-1.95285040758408));
#47610=CARTESIAN_POINT('Ctrl Pts',(-28.7580549536013,4.06806525915686,-0.819903316850643));
#47611=CARTESIAN_POINT('Ctrl Pts',(-28.6917637763688,4.09604925696662,0.666165809873902));
#47612=CARTESIAN_POINT('Ctrl Pts',(-28.6254725991363,3.49250488440095,1.82265529011987));
#47613=CARTESIAN_POINT('Ctrl Pts',(-28.5591814219038,2.88896051183525,2.97914477036591));
#47614=CARTESIAN_POINT('Ctrl Pts',(-28.4928902446714,1.65388776889405,3.80605460413334));
#47615=CARTESIAN_POINT('Ctrl Pts',(-28.4265990674389,0.354680341655036,
3.92350156485376));
#47616=CARTESIAN_POINT('Ctrl Pts',(-28.3603078902064,-0.944527085583904,
4.04094852557418));
#47617=CARTESIAN_POINT('Ctrl Pts',(-28.2940167129739,-2.30786919712065,
3.44893261324767));
#47618=CARTESIAN_POINT('Ctrl Pts',(-28.2277255357414,-3.10902522725881,
2.41942654578203));
#47619=CARTESIAN_POINT('Ctrl Pts',(-28.1838715311726,-3.63901883535004,
1.7383711524227));
#47620=CARTESIAN_POINT('Ctrl Pts',(-28.1400175266037,-3.92298296771959,
0.865856957318394));
#47621=CARTESIAN_POINT('Ctrl Pts',(-28.0961635220348,-3.92913455543446,
-0.00300513829252201));
#47622=CARTESIAN_POINT('Origin',(-54.75,0.,0.));
#47623=CARTESIAN_POINT('',(-26.6628364779652,-3.93868009607648,-0.00163299323942157));
#47624=CARTESIAN_POINT('',(-26.8461635220348,-3.93900474281862,-0.00127218255392029));
#47625=CARTESIAN_POINT('',(-54.75,-3.933,-4.81653586104654E-16));
#47626=CARTESIAN_POINT('Ctrl Pts',(-26.6628364779652,-3.93868009607648,
-0.00163299323942157));
#47627=CARTESIAN_POINT('Ctrl Pts',(-26.7245332450289,-3.93232394690408,
1.21313664908943));
#47628=CARTESIAN_POINT('Ctrl Pts',(-26.7862300120925,-3.32752073202559,
2.43337087631873));
#47629=CARTESIAN_POINT('Ctrl Pts',(-26.8479267791562,-2.3540132983783,3.15884220328027));
#47630=CARTESIAN_POINT('Ctrl Pts',(-26.9142179563887,-1.3080111025996,3.93833763880378));
#47631=CARTESIAN_POINT('Ctrl Pts',(-26.9805091336212,0.16365296950363,4.14663889280402));
#47632=CARTESIAN_POINT('Ctrl Pts',(-27.0468003108537,1.38489493234366,3.6880521553437));
#47633=CARTESIAN_POINT('Ctrl Pts',(-27.1130914880862,2.60613689518355,3.22946541788343));
#47634=CARTESIAN_POINT('Ctrl Pts',(-27.1793826653187,3.57695674876007,2.10399068896269));
#47635=CARTESIAN_POINT('Ctrl Pts',(-27.2456738425512,3.8513588556613,0.828672214500858));
#47636=CARTESIAN_POINT('Ctrl Pts',(-27.3119650197836,4.1257609625625,-0.4466462599609));
#47637=CARTESIAN_POINT('Ctrl Pts',(-27.3782561970162,3.70374532278838,-1.87180847996394));
#47638=CARTESIAN_POINT('Ctrl Pts',(-27.4445473742486,2.77918635450782,-2.79209345851531));
#47639=CARTESIAN_POINT('Ctrl Pts',(-27.5108385514811,1.85462738622716,-3.71237843706677));
#47640=CARTESIAN_POINT('Ctrl Pts',(-27.5771297287136,0.427525089440144,
-4.12778617416664));
#47641=CARTESIAN_POINT('Ctrl Pts',(-27.6434209059461,-0.846508275594557,
-3.84747792891868));
#47642=CARTESIAN_POINT('Ctrl Pts',(-27.7097120831786,-2.12054164062919,
-3.56716968367073));
#47643=CARTESIAN_POINT('Ctrl Pts',(-27.776003260411,-3.24150607391136,-2.59114545607491));
#47644=CARTESIAN_POINT('Ctrl Pts',(-27.8422944376435,-3.69442936396844,
-1.36779177831066));
#47645=CARTESIAN_POINT('Ctrl Pts',(-27.8658084510841,-3.85508489573833,
-0.933858394979657));
#47646=CARTESIAN_POINT('Ctrl Pts',(-27.8893224645246,-3.9316889655563,-0.468806566203696));
#47647=CARTESIAN_POINT('Ctrl Pts',(-27.9128364779652,-3.92865200925827,
-0.00278885010489754));
#47648=CARTESIAN_POINT('Ctrl Pts',(-28.0961635220348,-3.92913455543446,
-0.00300513829252201));
#47649=CARTESIAN_POINT('Ctrl Pts',(-28.0737263493712,-3.93228191306054,
-0.44754399059901));
#47650=CARTESIAN_POINT('Ctrl Pts',(-28.0512891767076,-3.86270663719881,
-0.891126837505349));
#47651=CARTESIAN_POINT('Ctrl Pts',(-28.028852004044,-3.71615203369125,-1.30762255129638));
#47652=CARTESIAN_POINT('Ctrl Pts',(-27.9625608268115,-3.28315286124596,
-2.53816935830421));
#47653=CARTESIAN_POINT('Ctrl Pts',(-27.896269649579,-2.17818456761584,-3.53226674971499));
#47654=CARTESIAN_POINT('Ctrl Pts',(-27.8299784723465,-0.908870721295116,
-3.83322536333816));
#47655=CARTESIAN_POINT('Ctrl Pts',(-27.763687295114,0.360443125025604,-4.13418397696132));
#47656=CARTESIAN_POINT('Ctrl Pts',(-27.6973961178816,1.79410252403693,-3.74200381279686));
#47657=CARTESIAN_POINT('Ctrl Pts',(-27.6311049406491,2.73348287598629,-2.83685284088832));
#47658=CARTESIAN_POINT('Ctrl Pts',(-27.5648137634166,3.67286322793571,-1.93170186897973));
#47659=CARTESIAN_POINT('Ctrl Pts',(-27.4985225861841,4.11796453282311,-0.513580089327008));
#47660=CARTESIAN_POINT('Ctrl Pts',(-27.4322314089516,3.86430679422603,0.766025896602054));
#47661=CARTESIAN_POINT('Ctrl Pts',(-27.3659402317191,3.61064905562898,2.04563188253097));
#47662=CARTESIAN_POINT('Ctrl Pts',(-27.2996490544866,2.65823227354765,3.18672207473626));
#47663=CARTESIAN_POINT('Ctrl Pts',(-27.2333578772542,1.44459769545578,3.66507846743426));
#47664=CARTESIAN_POINT('Ctrl Pts',(-27.1670667000217,0.230963117363835,
4.14343486013229));
#47665=CARTESIAN_POINT('Ctrl Pts',(-27.1007755227892,-1.24388925673868,
3.95905745332295));
#47666=CARTESIAN_POINT('Ctrl Pts',(-27.0344843455567,-2.30241073205211,
3.19664941698299));
#47667=CARTESIAN_POINT('Ctrl Pts',(-26.9717107377161,-3.30476451058249,
2.47469658576527));
#47668=CARTESIAN_POINT('Ctrl Pts',(-26.9089371298754,-3.93379819990021,
1.23442900344055));
#47669=CARTESIAN_POINT('Ctrl Pts',(-26.8461635220348,-3.93900474281862,
-0.00127218255392029));
#47670=CARTESIAN_POINT('Origin',(-54.75,0.,0.));
#47671=CARTESIAN_POINT('',(-25.4128364779652,-3.93366221636038,0.00359143100450002));
#47672=CARTESIAN_POINT('',(-25.5961635220348,-3.93301104109986,0.00363068149465887));
#47673=CARTESIAN_POINT('',(-54.75,-3.933,-4.81653586104654E-16));
#47674=CARTESIAN_POINT('Ctrl Pts',(-25.4128364779652,-3.93366221636038,
0.00359143100450002));
#47675=CARTESIAN_POINT('Ctrl Pts',(-25.4271616710682,-3.93629385844204,
0.286582248783829));
#47676=CARTESIAN_POINT('Ctrl Pts',(-25.4414868641711,-3.90836307935993,
0.569057703773814));
#47677=CARTESIAN_POINT('Ctrl Pts',(-25.4558120572741,-3.84794050571348,
0.844403066465243));
#47678=CARTESIAN_POINT('Ctrl Pts',(-25.5221032345066,-3.56832936821265,
2.11858960671787));
#47679=CARTESIAN_POINT('Ctrl Pts',(-25.5883944117391,-2.59291860342171,
3.24008788735299));
#47680=CARTESIAN_POINT('Ctrl Pts',(-25.6546855889715,-1.36981291807769,
3.69368044687598));
#47681=CARTESIAN_POINT('Ctrl Pts',(-25.720976766204,-0.146707232733672,
4.14727300639897));
#47682=CARTESIAN_POINT('Ctrl Pts',(-25.7872679434365,1.32409337316342,3.93295984480984));
#47683=CARTESIAN_POINT('Ctrl Pts',(-25.853559120669,2.36690159128718,3.14919664856431));
#47684=CARTESIAN_POINT('Ctrl Pts',(-25.9198502979015,3.40970980941095,2.36543345231877));
#47685=CARTESIAN_POINT('Ctrl Pts',(-25.986141475134,4.02452563976139,1.01222022141682));
#47686=CARTESIAN_POINT('Ctrl Pts',(-26.0524326523664,3.92890205868327,-0.288775496607364));
#47687=CARTESIAN_POINT('Ctrl Pts',(-26.1187238295989,3.83327847760514,-1.58977121463163));
#47688=CARTESIAN_POINT('Ctrl Pts',(-26.1850150068314,3.02721548509852,-2.83854941977796));
#47689=CARTESIAN_POINT('Ctrl Pts',(-26.2513061840639,1.88101924745432,-3.46142012256138));
#47690=CARTESIAN_POINT('Ctrl Pts',(-26.3175973612964,0.734823009810316,
-4.08429082534469));
#47691=CARTESIAN_POINT('Ctrl Pts',(-26.3838885385289,-0.75150647297135,
-4.08125402576508));
#47692=CARTESIAN_POINT('Ctrl Pts',(-26.4501797157614,-1.89514791058069,
-3.4537048326671));
#47693=CARTESIAN_POINT('Ctrl Pts',(-26.5164708929938,-3.03878934819016,
-2.82615563956904));
#47694=CARTESIAN_POINT('Ctrl Pts',(-26.5827620702263,-3.83974274062748,
-1.57409405295251));
#47695=CARTESIAN_POINT('Ctrl Pts',(-26.6490532474588,-3.93004927711913,
-0.272718451120987));
#47696=CARTESIAN_POINT('Ctrl Pts',(-26.6536476576276,-3.93630810803581,
-0.182524649349915));
#47697=CARTESIAN_POINT('Ctrl Pts',(-26.6582420677964,-3.93915342325037,
-0.0920939730132787));
#47698=CARTESIAN_POINT('Ctrl Pts',(-26.6628364779652,-3.93868009607648,
-0.00163299323942157));
#47699=CARTESIAN_POINT('Ctrl Pts',(-26.8461635220348,-3.93900474281862,
-0.00127218255392029));
#47700=CARTESIAN_POINT('Ctrl Pts',(-26.842645952643,-3.93929649562107,-0.0705156882063396));
#47701=CARTESIAN_POINT('Ctrl Pts',(-26.8391283832511,-3.93762942433138,
-0.139744855324124));
#47702=CARTESIAN_POINT('Ctrl Pts',(-26.8356108138592,-3.93395945147371,
-0.208867681384836));
#47703=CARTESIAN_POINT('Ctrl Pts',(-26.7693196366268,-3.86479611905754,
-1.51153807754211));
#47704=CARTESIAN_POINT('Ctrl Pts',(-26.7030284593943,-3.08427887770083,
-2.7764402039861));
#47705=CARTESIAN_POINT('Ctrl Pts',(-26.6367372821618,-1.95097814939022,
-3.42247672523399));
#47706=CARTESIAN_POINT('Ctrl Pts',(-26.5704461049293,-0.8176774210796,-4.06851324648187));
#47707=CARTESIAN_POINT('Ctrl Pts',(-26.5041549276968,0.66840679418499,-4.09568416253368));
#47708=CARTESIAN_POINT('Ctrl Pts',(-26.4378637504643,1.82456588224294,-3.49150712666056));
#47709=CARTESIAN_POINT('Ctrl Pts',(-26.3715725732318,2.98072497030096,-2.8873300907874));
#47710=CARTESIAN_POINT('Ctrl Pts',(-26.3052813959994,3.80695893115228,-1.65180510298944));
#47711=CARTESIAN_POINT('Ctrl Pts',(-26.2389902187669,3.92369503494019,-0.352533611095581));
#47712=CARTESIAN_POINT('Ctrl Pts',(-26.1726990415344,4.04043113872808,0.946737880798055));
#47713=CARTESIAN_POINT('Ctrl Pts',(-26.1064078643019,3.44766938545265,2.30975587678741));
#47714=CARTESIAN_POINT('Ctrl Pts',(-26.0401166870694,2.41772513311934,3.11034851019134));
#47715=CARTESIAN_POINT('Ctrl Pts',(-25.973825509837,1.38778088078586,3.9109411435954));
#47716=CARTESIAN_POINT('Ctrl Pts',(-25.9075343326045,-0.0793458706057278,
4.14910841441386));
#47717=CARTESIAN_POINT('Ctrl Pts',(-25.841243155372,-1.30965558526044,3.71543603392153));
#47718=CARTESIAN_POINT('Ctrl Pts',(-25.7749519781395,-2.53996529991508,
3.28176365342923));
#47719=CARTESIAN_POINT('Ctrl Pts',(-25.708660800907,-3.53345797783293,2.17625162162621));
#47720=CARTESIAN_POINT('Ctrl Pts',(-25.6423696236745,-3.83372206282286,
0.906773300881576));
#47721=CARTESIAN_POINT('Ctrl Pts',(-25.6269675897946,-3.90348515654062,
0.611823823105227));
#47722=CARTESIAN_POINT('Ctrl Pts',(-25.6115655559147,-3.93582675359008,
0.308023204452773));
#47723=CARTESIAN_POINT('Ctrl Pts',(-25.5961635220348,-3.93301104109986,
0.00363068149465887));
#47724=CARTESIAN_POINT('Origin',(-54.75,0.,0.));
#47725=CARTESIAN_POINT('',(-24.1628364779652,-3.92647812505579,-3.26061429916406E-5));
#47726=CARTESIAN_POINT('',(-24.3461635220348,-3.92651210140376,-0.000385812242292873));
#47727=CARTESIAN_POINT('',(-54.75,-3.933,-4.81653586104654E-16));
#47728=CARTESIAN_POINT('Ctrl Pts',(-24.1628364779652,-3.92647837592232,
-3.26048887833164E-5));
#47729=CARTESIAN_POINT('Ctrl Pts',(-24.1960812743399,-3.9264297878317,0.659749642360009));
#47730=CARTESIAN_POINT('Ctrl Pts',(-24.2293260707147,-3.76914112069753,
1.31955365614632));
#47731=CARTESIAN_POINT('Ctrl Pts',(-24.2625708670894,-3.45474121382766,
1.89325799077861));
#47732=CARTESIAN_POINT('Ctrl Pts',(-24.3288620443219,-2.82781783871468,
3.03724261012995));
#47733=CARTESIAN_POINT('Ctrl Pts',(-24.3951532215543,-1.57619466759501,
3.83888092698731));
#47734=CARTESIAN_POINT('Ctrl Pts',(-24.4614443987868,-0.274868670242791,
3.92989947559545));
#47735=CARTESIAN_POINT('Ctrl Pts',(-24.5277355760193,1.02645732710936,4.02091802420358));
#47736=CARTESIAN_POINT('Ctrl Pts',(-24.5940267532518,2.37748615069405,3.40131680456257));
#47737=CARTESIAN_POINT('Ctrl Pts',(-24.6603179304843,3.15755377194132,2.35574125308056));
#47738=CARTESIAN_POINT('Ctrl Pts',(-24.7266091077168,3.93762139318864,1.31016570159849));
#47739=CARTESIAN_POINT('Ctrl Pts',(-24.7929002849492,4.14672781209847,-0.161384181724622));
#47740=CARTESIAN_POINT('Ctrl Pts',(-24.8591914621817,3.68880932514741,-1.38287686974364));
#47741=CARTESIAN_POINT('Ctrl Pts',(-24.9254826394142,3.23089083819637,-2.60436955776259));
#47742=CARTESIAN_POINT('Ctrl Pts',(-24.9917738166467,2.10594744538451,-3.57580505047746));
#47743=CARTESIAN_POINT('Ctrl Pts',(-25.0580649938792,0.830779296277255,
-3.85090488522419));
#47744=CARTESIAN_POINT('Ctrl Pts',(-25.1243561711117,-0.444388852830141,
-4.12600471997094));
#47745=CARTESIAN_POINT('Ctrl Pts',(-25.1906473483441,-1.86978175823297,
-3.70476889674934));
#47746=CARTESIAN_POINT('Ctrl Pts',(-25.2569385255766,-2.79057245582902,
-2.78071358520342));
#47747=CARTESIAN_POINT('Ctrl Pts',(-25.3089045097062,-3.5123848715306,-2.05634202236053));
#47748=CARTESIAN_POINT('Ctrl Pts',(-25.3608704938357,-3.92411568741188,
-1.02298435333687));
#47749=CARTESIAN_POINT('Ctrl Pts',(-25.4128364779652,-3.93366221636038,
0.00359143100450002));
#47750=CARTESIAN_POINT('Ctrl Pts',(-25.5961635220348,-3.93301104109986,
0.00363068149465887));
#47751=CARTESIAN_POINT('Ctrl Pts',(-25.5452743786822,-3.92370777650038,
-1.00209848759207));
#47752=CARTESIAN_POINT('Ctrl Pts',(-25.4943852353297,-3.53060027531191,
-2.01428933941688));
#47753=CARTESIAN_POINT('Ctrl Pts',(-25.4434960919771,-2.83535683738727,
-2.73503460286112));
#47754=CARTESIAN_POINT('Ctrl Pts',(-25.3772049147446,-1.92969203489976,
-3.67391957617286));
#47755=CARTESIAN_POINT('Ctrl Pts',(-25.3109137375121,-0.511326937862769,
-4.11824491311015));
#47756=CARTESIAN_POINT('Ctrl Pts',(-25.2446225602796,0.76814007199996,-3.86388709772353));
#47757=CARTESIAN_POINT('Ctrl Pts',(-25.1783313830471,2.04760708186283,-3.60952928233688));
#47758=CARTESIAN_POINT('Ctrl Pts',(-25.1120402058146,3.18817600455133,-2.65648831462615));
#47759=CARTESIAN_POINT('Ctrl Pts',(-25.0457490285822,3.66586830603292,-1.4425921935841));
#47760=CARTESIAN_POINT('Ctrl Pts',(-24.9794578513497,4.14356060751448,-0.22869607254211));
#47761=CARTESIAN_POINT('Ctrl Pts',(-24.9131666741172,3.95837628778912,1.2460552018313));
#47762=CARTESIAN_POINT('Ctrl Pts',(-24.8468754968847,3.19538921345563,2.30415938005552));
#47763=CARTESIAN_POINT('Ctrl Pts',(-24.7805843196522,2.43240213912218,3.36226355827968));
#47764=CARTESIAN_POINT('Ctrl Pts',(-24.7142931424197,1.09161231018076,4.00372064035487));
#47765=CARTESIAN_POINT('Ctrl Pts',(-24.6480019651873,-0.211020049449589,
3.93384458423267));
#47766=CARTESIAN_POINT('Ctrl Pts',(-24.5817107879548,-1.51365240908001,
3.86396852811048));
#47767=CARTESIAN_POINT('Ctrl Pts',(-24.5154196107223,-2.77812729939929,
3.08275933379082));
#47768=CARTESIAN_POINT('Ctrl Pts',(-24.4491284334898,-3.42354365763898,
1.94910530716183));
#47769=CARTESIAN_POINT('Ctrl Pts',(-24.4148067963381,-3.7577019421051,1.36216653518887));
#47770=CARTESIAN_POINT('Ctrl Pts',(-24.3804851591865,-3.92591825646931,
0.680753029737708));
#47771=CARTESIAN_POINT('Ctrl Pts',(-24.3461635220348,-3.92651210140376,
-0.000385812242292873));
#47772=CARTESIAN_POINT('Origin',(-54.75,0.,0.));
#47773=CARTESIAN_POINT('',(-22.9128364779652,-3.93378229249503,-0.00358008960437806));
#47774=CARTESIAN_POINT('',(-23.0961635220348,-3.93443176527693,-0.00349624190913098));
#47775=CARTESIAN_POINT('',(-54.75,-3.933,-4.81653586104654E-16));
#47776=CARTESIAN_POINT('Ctrl Pts',(-22.9128364779652,-3.93378229249503,
-0.00358008960437806));
#47777=CARTESIAN_POINT('Ctrl Pts',(-22.9650008776117,-3.92420053618949,
1.02683468227007));
#47778=CARTESIAN_POINT('Ctrl Pts',(-23.0171652772582,-3.50898078364747,
2.06408445940646));
#47779=CARTESIAN_POINT('Ctrl Pts',(-23.0693296769046,-2.78223998347954,
2.78905061777197));
#47780=CARTESIAN_POINT('Ctrl Pts',(-23.1356208541371,-1.85868860528863,
3.71034675876961));
#47781=CARTESIAN_POINT('Ctrl Pts',(-23.2019120313696,-0.432041729477022,
4.12731587666033));
#47782=CARTESIAN_POINT('Ctrl Pts',(-23.2682032086021,0.842297604559967,
3.84840193060951));
#47783=CARTESIAN_POINT('Ctrl Pts',(-23.3344943858346,2.11663693859703,3.56948798455867));
#47784=CARTESIAN_POINT('Ctrl Pts',(-23.4007855630671,3.23866873085946,2.59469097456621));
#47785=CARTESIAN_POINT('Ctrl Pts',(-23.4670767402996,3.69293042406328,1.37183364778468));
#47786=CARTESIAN_POINT('Ctrl Pts',(-23.533367917532,4.14719211726705,0.14897632100329));
#47787=CARTESIAN_POINT('Ctrl Pts',(-23.5996590947645,3.93368371141241,-1.3219413225671));
#47788=CARTESIAN_POINT('Ctrl Pts',(-23.665950271997,3.15049118734441,-2.36517820737289));
#47789=CARTESIAN_POINT('Ctrl Pts',(-23.7322414492295,2.36729866327638,-3.40841509217874));
#47790=CARTESIAN_POINT('Ctrl Pts',(-23.798532626462,1.01442202099493,-4.02397121821994));
#47791=CARTESIAN_POINT('Ctrl Pts',(-23.8648238036945,-0.286625821123579,
-3.92905946924091));
#47792=CARTESIAN_POINT('Ctrl Pts',(-23.931114980927,-1.58767366324201,-3.83414772026189));
#47793=CARTESIAN_POINT('Ctrl Pts',(-23.9974061581594,-2.83689270519751,
-3.02876809626271));
#47794=CARTESIAN_POINT('Ctrl Pts',(-24.0636973353919,-3.46039043662218,
-1.88291282334053));
#47795=CARTESIAN_POINT('Ctrl Pts',(-24.0967437162497,-3.77120620965261,
-1.31170001135402));
#47796=CARTESIAN_POINT('Ctrl Pts',(-24.1297900971074,-3.92652667402376,
-0.655877061868211));
#47797=CARTESIAN_POINT('Ctrl Pts',(-24.1628364779652,-3.92647837592232,
-3.26048887833164E-5));
#47798=CARTESIAN_POINT('Ctrl Pts',(-24.3461635220348,-3.92651210140376,
-0.000385812242292873));
#47799=CARTESIAN_POINT('Ctrl Pts',(-24.314193981954,-3.92706524953448,-0.634845509286078));
#47800=CARTESIAN_POINT('Ctrl Pts',(-24.2822244418732,-3.78218336924519,
-1.26906689884118));
#47801=CARTESIAN_POINT('Ctrl Pts',(-24.2502549017923,-3.49050832372137,
-1.82647592817378));
#47802=CARTESIAN_POINT('Ctrl Pts',(-24.1839637245598,-2.885698805404,-2.98230427794211));
#47803=CARTESIAN_POINT('Ctrl Pts',(-24.1176725473274,-1.64972194260919,
-3.80786211854049));
#47804=CARTESIAN_POINT('Ctrl Pts',(-24.0513813700949,-0.350386775003562,
-3.92388733045038));
#47805=CARTESIAN_POINT('Ctrl Pts',(-23.9850901928624,0.948948392601992,
-4.03991254236027));
#47806=CARTESIAN_POINT('Ctrl Pts',(-23.9187990156299,2.31164186501836,-3.44640512558175));
#47807=CARTESIAN_POINT('Ctrl Pts',(-23.8525078383975,3.11167086202694,-2.41602299669911));
#47808=CARTESIAN_POINT('Ctrl Pts',(-23.786216661165,3.91169985903557,-1.38564086781641));
#47809=CARTESIAN_POINT('Ctrl Pts',(-23.7199254839325,4.14906438063636,0.0816159731704677));
#47810=CARTESIAN_POINT('Ctrl Pts',(-23.6536343067,3.71471892191887,1.31168822717304));
#47811=CARTESIAN_POINT('Ctrl Pts',(-23.5873431294675,3.28037346320138,2.54176048117561));
#47812=CARTESIAN_POINT('Ctrl Pts',(-23.521051952235,2.17431802416562,3.53464814819388));
#47813=CARTESIAN_POINT('Ctrl Pts',(-23.4547607750026,0.904675609021257,
3.83421761466514));
#47814=CARTESIAN_POINT('Ctrl Pts',(-23.3884695977701,-0.364966806123031,
4.13378708113639));
#47815=CARTESIAN_POINT('Ctrl Pts',(-23.3221784205376,-1.7981961973759,3.7400383470607));
#47816=CARTESIAN_POINT('Ctrl Pts',(-23.2558872433051,-2.73658551099054,
2.83385998510919));
#47817=CARTESIAN_POINT('Ctrl Pts',(-23.2026460028817,-3.4902455475549,2.10606992239897));
#47818=CARTESIAN_POINT('Ctrl Pts',(-23.1494047624583,-3.92471524826081,
1.04774360683275));
#47819=CARTESIAN_POINT('Ctrl Pts',(-23.0961635220348,-3.93443176527693,
-0.00349624190913098));
#47820=CARTESIAN_POINT('Origin',(-54.75,0.,0.));
#47821=CARTESIAN_POINT('',(-21.6628364779652,-3.93861276308604,0.00169727802626606));
#47822=CARTESIAN_POINT('',(-21.8461635220348,-3.93821003127031,0.00203258821323272));
#47823=CARTESIAN_POINT('',(-54.75,-3.933,-4.81653586104654E-16));
#47824=CARTESIAN_POINT('Ctrl Pts',(-21.6628364779652,-3.93861276308604,
0.00169727802626606));
#47825=CARTESIAN_POINT('Ctrl Pts',(-21.667629303651,-3.93912300404395,0.0960692092454155));
#47826=CARTESIAN_POINT('Ctrl Pts',(-21.6724221293367,-3.93602631799819,
0.190407079145342));
#47827=CARTESIAN_POINT('Ctrl Pts',(-21.6772149550225,-3.92921570361644,
0.284476059837029));
#47828=CARTESIAN_POINT('Ctrl Pts',(-21.743506132255,-3.83501581514877,1.58557563657516));
#47829=CARTESIAN_POINT('Ctrl Pts',(-21.8097973094874,-3.03031980075104,
2.83523514138036));
#47830=CARTESIAN_POINT('Ctrl Pts',(-21.8760884867199,-1.88480583556769,
3.45935971479932));
#47831=CARTESIAN_POINT('Ctrl Pts',(-21.9423796639524,-0.739291870384334,
4.08348428821828));
#47832=CARTESIAN_POINT('Ctrl Pts',(-22.0086708411849,0.747040045584634,
4.082073930251));
#47833=CARTESIAN_POINT('Ctrl Pts',(-22.0749620184174,1.89136750422079,3.45577656079557));
#47834=CARTESIAN_POINT('Ctrl Pts',(-22.1412531956499,3.03569496285695,2.82947919134014));
#47835=CARTESIAN_POINT('Ctrl Pts',(-22.2075443728823,3.8380179641603,1.57829481039657));
#47836=CARTESIAN_POINT('Ctrl Pts',(-22.2738355501148,3.92974849763818,0.277018807081612));
#47837=CARTESIAN_POINT('Ctrl Pts',(-22.3401267273473,4.02147903111605,-1.02425719623327));
#47838=CARTESIAN_POINT('Ctrl Pts',(-22.4064179045798,3.40261709676853,-2.37562482191952));
#47839=CARTESIAN_POINT('Ctrl Pts',(-22.4727090818123,2.35746850258097,-3.15626439537392));
#47840=CARTESIAN_POINT('Ctrl Pts',(-22.5390002590448,1.31231990839341,-3.93690396882831));
#47841=CARTESIAN_POINT('Ctrl Pts',(-22.6052914362772,-0.159115345634208,
-4.14681549005081));
#47842=CARTESIAN_POINT('Ctrl Pts',(-22.6715826135097,-1.38085839317283,
-3.68956539068907));
#47843=CARTESIAN_POINT('Ctrl Pts',(-22.7378737907422,-2.60260144071159,
-3.23231529132727));
#47844=CARTESIAN_POINT('Ctrl Pts',(-22.8041649679747,-3.57465228176129,
-2.10790357138104));
#47845=CARTESIAN_POINT('Ctrl Pts',(-22.8704561452072,-3.85044976200099,
-0.832886129355597));
#47846=CARTESIAN_POINT('Ctrl Pts',(-22.8845829227932,-3.9092227363964,-0.561177455988717));
#47847=CARTESIAN_POINT('Ctrl Pts',(-22.8987097003792,-3.93637715299624,
-0.282629410640403));
#47848=CARTESIAN_POINT('Ctrl Pts',(-22.9128364779652,-3.93378229249503,
-0.00358008960437806));
#47849=CARTESIAN_POINT('Ctrl Pts',(-23.0961635220348,-3.93443176527693,
-0.00349624190913098));
#47850=CARTESIAN_POINT('Ctrl Pts',(-23.0831135852258,-3.93681337645008,
-0.261165174641599));
#47851=CARTESIAN_POINT('Ctrl Pts',(-23.0700636484167,-3.91367637085558,
-0.51840836169853));
#47852=CARTESIAN_POINT('Ctrl Pts',(-23.0570137116076,-3.86346624454843,
-0.770254017452239));
#47853=CARTESIAN_POINT('Ctrl Pts',(-22.9907225343752,-3.60840842851518,
-2.04958166823441));
#47854=CARTESIAN_POINT('Ctrl Pts',(-22.9244313571426,-2.65474356047235,
-3.18962897997126));
#47855=CARTESIAN_POINT('Ctrl Pts',(-22.8581401799102,-1.44058625986577,
-3.66665704723695));
#47856=CARTESIAN_POINT('Ctrl Pts',(-22.7918490026777,-0.226428959259131,
-4.14368511450266));
#47857=CARTESIAN_POINT('Ctrl Pts',(-22.7255578254452,1.24822077391129,-3.95769393729713));
#47858=CARTESIAN_POINT('Ctrl Pts',(-22.6592666482127,2.30590733829799,-3.19412805337387));
#47859=CARTESIAN_POINT('Ctrl Pts',(-22.5929754709802,3.36359390268457,-2.43056216945069));
#47860=CARTESIAN_POINT('Ctrl Pts',(-22.5266842937477,4.00431729828756,-1.08942157880993));
#47861=CARTESIAN_POINT('Ctrl Pts',(-22.4603931165152,3.93372853937707,0.213172354344517));
#47862=CARTESIAN_POINT('Ctrl Pts',(-22.3941019392827,3.86313978046657,1.51576628749911));
#47863=CARTESIAN_POINT('Ctrl Pts',(-22.3278107620503,3.08123886704243,2.77981356316738));
#47864=CARTESIAN_POINT('Ctrl Pts',(-22.2615195848178,1.94723188145956,3.42460956519045));
#47865=CARTESIAN_POINT('Ctrl Pts',(-22.1952284075853,0.813224895876891,
4.06940556721341));
#47866=CARTESIAN_POINT('Ctrl Pts',(-22.1289372303528,-0.672888161864364,
4.09495029559142));
#47867=CARTESIAN_POINT('Ctrl Pts',(-22.0626460531203,-1.82838542734041,
3.48950847588248));
#47868=CARTESIAN_POINT('Ctrl Pts',(-21.9963548758879,-2.98388269281665,
2.88406665617344));
#47869=CARTESIAN_POINT('Ctrl Pts',(-21.9300636986554,-3.80876416602755,
1.6476382883772));
#47870=CARTESIAN_POINT('Ctrl Pts',(-21.8637725214229,-3.92407845132676,
0.348239834021639));
#47871=CARTESIAN_POINT('Ctrl Pts',(-21.8579028549602,-3.93428880542434,
0.233186280176151));
#47872=CARTESIAN_POINT('Ctrl Pts',(-21.8520331884975,-3.93893616145868,
0.117639041623225));
#47873=CARTESIAN_POINT('Ctrl Pts',(-21.8461635220348,-3.93821003127031,
0.00203258821323272));
#47874=CARTESIAN_POINT('Origin',(-54.75,0.,0.));
#47875=CARTESIAN_POINT('',(-20.4128364779652,-3.92856748927321,0.00274604364064041));
#47876=CARTESIAN_POINT('',(-20.5961635220349,-3.92813410533466,0.00249872673611579));
#47877=CARTESIAN_POINT('',(-54.75,-3.933,-4.81653586104654E-16));
#47878=CARTESIAN_POINT('Ctrl Pts',(-20.4128364779652,-3.92856748927321,
0.00274604364064041));
#47879=CARTESIAN_POINT('Ctrl Pts',(-20.4365489069227,-3.9315789798689,0.472721489178729));
#47880=CARTESIAN_POINT('Ctrl Pts',(-20.4602613358802,-3.85364009669069,
0.941731212379603));
#47881=CARTESIAN_POINT('Ctrl Pts',(-20.4839737648377,-3.69032035174204,
1.3788395032363));
#47882=CARTESIAN_POINT('Ctrl Pts',(-20.5502649420702,-3.2337387768493,2.60083254456009));
#47883=CARTESIAN_POINT('Ctrl Pts',(-20.6165561193027,-2.1098590663668,3.57349844295636));
#47884=CARTESIAN_POINT('Ctrl Pts',(-20.6828472965352,-0.834992713105839,
3.84999348612781));
#47885=CARTESIAN_POINT('Ctrl Pts',(-20.7491384737677,0.439873640155124,
4.12648852929926));
#47886=CARTESIAN_POINT('Ctrl Pts',(-20.8154296510002,1.86572663619477,3.70681271724578));
#47887=CARTESIAN_POINT('Ctrl Pts',(-20.8817208282327,2.78752794479972,2.78376554887926));
#47888=CARTESIAN_POINT('Ctrl Pts',(-20.9480120054651,3.70932925340478,1.86071838051265));
#47889=CARTESIAN_POINT('Ctrl Pts',(-21.0143031826976,4.12707887457528,0.434299855833041));
#47890=CARTESIAN_POINT('Ctrl Pts',(-21.0805943599301,3.84886220346862,-0.840191890509009));
#47891=CARTESIAN_POINT('Ctrl Pts',(-21.1468855371626,3.570645532362,-2.11468363685091));
#47892=CARTESIAN_POINT('Ctrl Pts',(-21.2131767143951,2.59646256897831,-3.23724860485509));
#47893=CARTESIAN_POINT('Ctrl Pts',(-21.2794678916276,1.37385396682755,-3.69217929575456));
#47894=CARTESIAN_POINT('Ctrl Pts',(-21.34575906886,0.15124536467666,-4.14710998665408));
#47895=CARTESIAN_POINT('Ctrl Pts',(-21.4120502460925,-1.31978887624136,
-3.9344064004487));
#47896=CARTESIAN_POINT('Ctrl Pts',(-21.478341423325,-2.36345411543157,-3.15178478301042));
#47897=CARTESIAN_POINT('Ctrl Pts',(-21.5398397748717,-3.33166277390398,
-2.42574639650694));
#47898=CARTESIAN_POINT('Ctrl Pts',(-21.6013381264185,-3.93206569046954,
-1.20922057769968));
#47899=CARTESIAN_POINT('Ctrl Pts',(-21.6628364779652,-3.93861276308604,
0.00169727802626606));
#47900=CARTESIAN_POINT('Ctrl Pts',(-21.8461635220348,-3.93821003127031,
0.00203258821323272));
#47901=CARTESIAN_POINT('Ctrl Pts',(-21.785742011265,-3.9307353505068,-1.18800378168487));
#47902=CARTESIAN_POINT('Ctrl Pts',(-21.7253205004952,-3.35386723851819,
-2.38431476535265));
#47903=CARTESIAN_POINT('Ctrl Pts',(-21.6648989897255,-2.4143201370314,-3.11299228236934));
#47904=CARTESIAN_POINT('Ctrl Pts',(-21.598607812493,-1.38350044004909,-3.9124574034903));
#47905=CARTESIAN_POINT('Ctrl Pts',(-21.5323166352605,0.0838860513029625,
-4.14901910481729));
#47906=CARTESIAN_POINT('Ctrl Pts',(-21.466025458028,1.31372047642571,-3.71400069789792));
#47907=CARTESIAN_POINT('Ctrl Pts',(-21.3997342807955,2.54355490154839,-3.27898229097857));
#47908=CARTESIAN_POINT('Ctrl Pts',(-21.333443103563,3.53583726044157,-2.17238377581286));
#47909=CARTESIAN_POINT('Ctrl Pts',(-21.2671519263305,3.83471201871666,-0.902577646342112));
#47910=CARTESIAN_POINT('Ctrl Pts',(-21.2008607490981,4.13358677699174,0.367228483128639));
#47911=CARTESIAN_POINT('Ctrl Pts',(-21.1345695718656,3.73905393464871,1.80024222690445));
#47912=CARTESIAN_POINT('Ctrl Pts',(-21.0682783946331,2.83236228450172,2.73813559991076));
#47913=CARTESIAN_POINT('Ctrl Pts',(-21.0019872174006,1.92567063435478,3.67602897291702));
#47914=CARTESIAN_POINT('Ctrl Pts',(-20.9356960401681,0.506820176403872,
4.11880197515389));
#47915=CARTESIAN_POINT('Ctrl Pts',(-20.8694048629356,-0.772367732324979,
3.86304423482693));
#47916=CARTESIAN_POINT('Ctrl Pts',(-20.8031136857032,-2.05155564105398,
3.60728649449995));
#47917=CARTESIAN_POINT('Ctrl Pts',(-20.7368225084707,-3.19108100056096,
2.65299801160893));
#47918=CARTESIAN_POINT('Ctrl Pts',(-20.6705313312382,-3.66744469081024,
1.43857989490129));
#47919=CARTESIAN_POINT('Ctrl Pts',(-20.6457420615037,-3.84557862208538,
0.984454028952772));
#47920=CARTESIAN_POINT('Ctrl Pts',(-20.6209527917693,-3.93097931647737,
0.493952925906998));
#47921=CARTESIAN_POINT('Ctrl Pts',(-20.5961635220349,-3.92813410533466,
0.00249872673611579));
#47922=CARTESIAN_POINT('Origin',(-54.75,0.,0.));
#47923=CARTESIAN_POINT('',(-19.1628364779652,-3.92859004817972,-0.00275762651098022));
#47924=CARTESIAN_POINT('',(-19.3461635220348,-3.92906724673901,-0.00297761340060153));
#47925=CARTESIAN_POINT('',(-54.75,-3.933,-4.81653586104654E-16));
#47926=CARTESIAN_POINT('Ctrl Pts',(-19.1628364779652,-3.92859004817972,
-0.00275762651098022));
#47927=CARTESIAN_POINT('Ctrl Pts',(-19.2054685101945,-3.92315095775244,
0.842188267718036));
#47928=CARTESIAN_POINT('Ctrl Pts',(-19.2481005424238,-3.65601617471943,
1.69027015247434));
#47929=CARTESIAN_POINT('Ctrl Pts',(-19.290732574653,-3.15307743517508,2.36172931597933));
#47930=CARTESIAN_POINT('Ctrl Pts',(-19.3570237518855,-2.37102695864804,
3.40582259712777));
#47931=CARTESIAN_POINT('Ctrl Pts',(-19.423314929118,-1.01882470847633,4.02285876152022));
#47932=CARTESIAN_POINT('Ctrl Pts',(-19.4896061063505,0.282326213391258,
3.92937076176308));
#47933=CARTESIAN_POINT('Ctrl Pts',(-19.555897283583,1.58347713525885,3.83588276200594));
#47934=CARTESIAN_POINT('Ctrl Pts',(-19.6221884608154,2.83357672882233,3.03187059809921));
#47935=CARTESIAN_POINT('Ctrl Pts',(-19.6884796380479,3.45832795740103,1.8866982835697));
#47936=CARTESIAN_POINT('Ctrl Pts',(-19.7547708152804,4.08307918597977,0.741525969040118));
#47937=CARTESIAN_POINT('Ctrl Pts',(-19.8210619925129,4.08248204957366,-0.744806496112277));
#47938=CARTESIAN_POINT('Ctrl Pts',(-19.8873531697454,3.45681087326069,-1.88947645147357));
#47939=CARTESIAN_POINT('Ctrl Pts',(-19.9536443469779,2.83113969694779,-3.03414640683473));
#47940=CARTESIAN_POINT('Ctrl Pts',(-20.0199355242103,1.5803944807282,-3.83715385240487));
#47941=CARTESIAN_POINT('Ctrl Pts',(-20.0862267014428,0.279168860993574,
-3.92959634329253));
#47942=CARTESIAN_POINT('Ctrl Pts',(-20.1525178786753,-1.02205675874106,
-4.02203883418018));
#47943=CARTESIAN_POINT('Ctrl Pts',(-20.2188090559078,-2.37376278199073,
-3.40391637038534));
#47944=CARTESIAN_POINT('Ctrl Pts',(-20.2851002331403,-3.15497407396417,
-2.35919504636229));
#47945=CARTESIAN_POINT('Ctrl Pts',(-20.3276789814153,-3.65674520459068,
-1.68817171972752));
#47946=CARTESIAN_POINT('Ctrl Pts',(-20.3702577296902,-3.92315996648268,
-0.841155955046957));
#47947=CARTESIAN_POINT('Ctrl Pts',(-20.4128364779652,-3.92856748927321,
0.00274604364064041));
#47948=CARTESIAN_POINT('Ctrl Pts',(-20.5961635220349,-3.92813410533466,
0.00249872673611579));
#47949=CARTESIAN_POINT('Ctrl Pts',(-20.5546616145368,-3.92337068588254,
-0.820288185989406));
#47950=CARTESIAN_POINT('Ctrl Pts',(-20.5131597070388,-3.67126222185311,
-1.64574653828059));
#47951=CARTESIAN_POINT('Ctrl Pts',(-20.4716577995407,-3.19286593711536,
-2.30765460625607));
#47952=CARTESIAN_POINT('Ctrl Pts',(-20.4053666223083,-2.42872147217945,
-3.36492324018196));
#47953=CARTESIAN_POINT('Ctrl Pts',(-20.3390754450758,-1.08723052131588,
-4.00491275750937));
#47954=CARTESIAN_POINT('Ctrl Pts',(-20.2727842678433,0.215324595425315,
-3.93361131694164));
#47955=CARTESIAN_POINT('Ctrl Pts',(-20.2064930906108,1.51787971216637,-3.86230987637392));
#47956=CARTESIAN_POINT('Ctrl Pts',(-20.1402019133783,2.78149899478498,-3.07971747791123));
#47957=CARTESIAN_POINT('Ctrl Pts',(-20.0739107361458,3.42567444756889,-1.94535787284501));
#47958=CARTESIAN_POINT('Ctrl Pts',(-20.0076195589133,4.06984990035283,-0.810998267778726));
#47959=CARTESIAN_POINT('Ctrl Pts',(-19.9413283816809,4.09458152330189,0.675128543891286));
#47960=CARTESIAN_POINT('Ctrl Pts',(-19.8750372044484,3.48850758344289,1.8302943791718));
#47961=CARTESIAN_POINT('Ctrl Pts',(-19.8087460272159,2.8824336435839,2.98546021445231));
#47962=CARTESIAN_POINT('Ctrl Pts',(-19.7424548499834,1.64555414091693,3.80966507334347));
#47963=CARTESIAN_POINT('Ctrl Pts',(-19.6761636727509,0.346092788792513,
3.92426839751211));
#47964=CARTESIAN_POINT('Ctrl Pts',(-19.6098724955184,-0.953368563331904,
4.03887172168075));
#47965=CARTESIAN_POINT('Ctrl Pts',(-19.5435813182859,-2.31541176491369,
3.44387351112686));
#47966=CARTESIAN_POINT('Ctrl Pts',(-19.4772901410534,-3.11431277082326,
2.41261655462562));
#47967=CARTESIAN_POINT('Ctrl Pts',(-19.4335812680472,-3.64106556161118,
1.73266062036312));
#47968=CARTESIAN_POINT('Ctrl Pts',(-19.389872395041,-3.92299895519764,0.863046365293776));
#47969=CARTESIAN_POINT('Ctrl Pts',(-19.3461635220348,-3.92906724673901,
-0.00297761340060153));
#47970=CARTESIAN_POINT('Origin',(-54.75,0.,0.));
#47971=CARTESIAN_POINT('',(-17.9128364779652,-3.93863106461684,-0.00168008665984931));
#47972=CARTESIAN_POINT('',(-18.0961635220349,-3.93896517016805,-0.00132190172209247));
#47973=CARTESIAN_POINT('',(-54.75,-3.933,-4.81653586104654E-16));
#47974=CARTESIAN_POINT('Ctrl Pts',(-17.9128364779652,-3.93863106461684,
-0.00168008665984931));
#47975=CARTESIAN_POINT('Ctrl Pts',(-17.9743881134662,-3.93213463944834,
1.21027201576146));
#47976=CARTESIAN_POINT('Ctrl Pts',(-18.0359397489673,-3.33055199309392,
2.427794228091));
#47977=CARTESIAN_POINT('Ctrl Pts',(-18.0974913844683,-2.36092088390748,
3.15368280809849));
#47978=CARTESIAN_POINT('Ctrl Pts',(-18.1637825617008,-1.31662714279099,
3.93546558473174));
#47979=CARTESIAN_POINT('Ctrl Pts',(-18.2300737389333,0.154577531237571,
4.14698712182452));
#47980=CARTESIAN_POINT('Ctrl Pts',(-18.2963649161657,1.37682020053737,3.69107420808071));
#47981=CARTESIAN_POINT('Ctrl Pts',(-18.3626560933982,2.59906286983725,3.23516129433688));
#47982=CARTESIAN_POINT('Ctrl Pts',(-18.4289472706308,3.57234353440834,2.11181392975638));
#47983=CARTESIAN_POINT('Ctrl Pts',(-18.4952384478632,3.84953605774138,0.837099046896719));
#47984=CARTESIAN_POINT('Ctrl Pts',(-18.5615296250957,4.12672858107439,-0.437615835962802));
#47985=CARTESIAN_POINT('Ctrl Pts',(-18.6278208023282,3.70783296316955,-1.86369823710145));
#47986=CARTESIAN_POINT('Ctrl Pts',(-18.6941119795607,2.78529028094574,-2.78600443736826));
#47987=CARTESIAN_POINT('Ctrl Pts',(-18.7604031567931,1.86274759872194,-3.70831063763507));
#47988=CARTESIAN_POINT('Ctrl Pts',(-18.8266943340256,0.436557852179171,
-4.12684063703003));
#47989=CARTESIAN_POINT('Ctrl Pts',(-18.8929855112581,-0.838085924942725,
-3.84932132415304));
#47990=CARTESIAN_POINT('Ctrl Pts',(-18.9592766884906,-2.11272970206469,
-3.57180201127604));
#47991=CARTESIAN_POINT('Ctrl Pts',(-19.0255678657231,-3.23582750976577,
-2.598233386127));
#47992=CARTESIAN_POINT('Ctrl Pts',(-19.0918590429556,-3.69142706217513,
-1.37587387460027));
#47993=CARTESIAN_POINT('Ctrl Pts',(-19.1155181879588,-3.85402933179616,
-0.939617013029593));
#47994=CARTESIAN_POINT('Ctrl Pts',(-19.139177332962,-3.93160853503985,-0.471670234850337));
#47995=CARTESIAN_POINT('Ctrl Pts',(-19.1628364779652,-3.92859004817972,
-0.00275762651098022));
#47996=CARTESIAN_POINT('Ctrl Pts',(-19.3461635220348,-3.92906724673901,
-0.00297761340060153));
#47997=CARTESIAN_POINT('Ctrl Pts',(-19.3235812178085,-3.93220244552808,
-0.450411180295741));
#47998=CARTESIAN_POINT('Ctrl Pts',(-19.3009989135823,-3.86170098893934,
-0.8968863949304));
#47999=CARTESIAN_POINT('Ctrl Pts',(-19.278416609356,-3.71328136207362,-1.31575233241029));
#48000=CARTESIAN_POINT('Ctrl Pts',(-19.2121254321235,-3.27759013717716,
-2.54534856049627));
#48001=CARTESIAN_POINT('Ctrl Pts',(-19.145834254891,-2.17044887714702,-3.53702531421994));
#48002=CARTESIAN_POINT('Ctrl Pts',(-19.0795430776586,-0.90047941347239,
-3.83520527482935));
#48003=CARTESIAN_POINT('Ctrl Pts',(-19.0132519004261,0.369490050202456,
-4.13338523543881));
#48004=CARTESIAN_POINT('Ctrl Pts',(-18.9469607231936,1.80228771752193,-3.73806840293375));
#48005=CARTESIAN_POINT('Ctrl Pts',(-18.8806695459611,2.73968486915726,-2.83086373601366));
#48006=CARTESIAN_POINT('Ctrl Pts',(-18.8143783687286,3.67708202079254,-1.92365906909362));
#48007=CARTESIAN_POINT('Ctrl Pts',(-18.7480871914961,4.11907865674376,-0.504566567758773));
#48008=CARTESIAN_POINT('Ctrl Pts',(-18.6817960142637,3.86262106868525,0.774481215986085));
#48009=CARTESIAN_POINT('Ctrl Pts',(-18.6155048370312,3.60616348062672,2.05352899973102));
#48010=CARTESIAN_POINT('Ctrl Pts',(-18.5492136597987,2.65125166855823,3.19253206588583));
#48011=CARTESIAN_POINT('Ctrl Pts',(-18.4829224825662,1.43657309929127,3.66823123651701));
#48012=CARTESIAN_POINT('Ctrl Pts',(-18.4166313053337,0.221894530024308,
4.14393040714819));
#48013=CARTESIAN_POINT('Ctrl Pts',(-18.3503401281012,-1.25255079644121,
3.95632568225578));
#48014=CARTESIAN_POINT('Ctrl Pts',(-18.2840489508687,-2.3094011834078,3.19160286505716));
#48015=CARTESIAN_POINT('Ctrl Pts',(-18.2214204745908,-3.30785877841104,
2.46913229181379));
#48016=CARTESIAN_POINT('Ctrl Pts',(-18.1587919983128,-3.9335922899934,1.23155535200719));
#48017=CARTESIAN_POINT('Ctrl Pts',(-18.0961635220349,-3.93896517016805,
-0.00132190172209248));
#48018=CARTESIAN_POINT('Origin',(-54.75,0.,0.));
#48019=CARTESIAN_POINT('',(-16.6628364779652,-3.93375005137208,0.00358326100158749));
#48020=CARTESIAN_POINT('',(-16.8461635220349,-3.93309862886983,0.00362758403216595));
#48021=CARTESIAN_POINT('',(-54.75,-3.933,-4.81653586104654E-16));
#48022=CARTESIAN_POINT('Ctrl Pts',(-16.6628364779652,-3.93375005137208,
0.00358326100158748));
#48023=CARTESIAN_POINT('Ctrl Pts',(-16.6770165395055,-3.93635487154669,
0.283691000235229));
#48024=CARTESIAN_POINT('Ctrl Pts',(-16.6911966010458,-3.90899307237427,
0.563293683724424));
#48025=CARTESIAN_POINT('Ctrl Pts',(-16.7053766625861,-3.84977929252528,
0.83597970849176));
#48026=CARTESIAN_POINT('Ctrl Pts',(-16.7716678398186,-3.57295742095455,
2.11077513482312));
#48027=CARTESIAN_POINT('Ctrl Pts',(-16.8379590170511,-2.60000342548255,
3.23440544601643));
#48028=CARTESIAN_POINT('Ctrl Pts',(-16.9042501942836,-1.37789337049898,
3.69067372354986));
#48029=CARTESIAN_POINT('Ctrl Pts',(-16.9705413715161,-0.155783315515329,
4.14694200108332));
#48030=CARTESIAN_POINT('Ctrl Pts',(-17.0368325487485,1.31548279897993,3.93584824495684));
#48031=CARTESIAN_POINT('Ctrl Pts',(-17.103123725981,2.3600038095325,3.15436914345143));
#48032=CARTESIAN_POINT('Ctrl Pts',(-17.1694149032135,3.40452482008502,2.37289004194606));
#48033=CARTESIAN_POINT('Ctrl Pts',(-17.235706080446,4.0223007266949,1.02102559506183));
#48034=CARTESIAN_POINT('Ctrl Pts',(-17.3019972576785,3.92952464363444,-0.280176282429607));
#48035=CARTESIAN_POINT('Ctrl Pts',(-17.368288434911,3.83674856057397,-1.58137815992119));
#48036=CARTESIAN_POINT('Ctrl Pts',(-17.4345796121435,3.03342048784297,-2.83191746801997));
#48037=CARTESIAN_POINT('Ctrl Pts',(-17.500870789376,1.88859016677985,-3.45729516473628));
#48038=CARTESIAN_POINT('Ctrl Pts',(-17.5671619666084,0.743759845716805,
-4.08267286145256));
#48039=CARTESIAN_POINT('Ctrl Pts',(-17.6334531438409,-0.742572723678316,
-4.08288894678644));
#48040=CARTESIAN_POINT('Ctrl Pts',(-17.6997443210734,-1.88758483310244,
-3.4578441509137));
#48041=CARTESIAN_POINT('Ctrl Pts',(-17.7660354983059,-3.03259694252663,
-2.83279935504092));
#48042=CARTESIAN_POINT('Ctrl Pts',(-17.8323266755384,-3.83628859197978,
-1.58249367796145));
#48043=CARTESIAN_POINT('Ctrl Pts',(-17.8986178527708,-3.92944301260406,
-0.281318831334825));
#48044=CARTESIAN_POINT('Ctrl Pts',(-17.9033573945023,-3.93610316381045,
-0.188290275455156));
#48045=CARTESIAN_POINT('Ctrl Pts',(-17.9080969362338,-3.93913129629941,
-0.0950016941068158));
#48046=CARTESIAN_POINT('Ctrl Pts',(-17.9128364779652,-3.93863106461684,
-0.00168008665984931));
#48047=CARTESIAN_POINT('Ctrl Pts',(-18.0961635220349,-3.93896517016805,
-0.00132190172209248));
#48048=CARTESIAN_POINT('Ctrl Pts',(-18.0925008210803,-3.93927939230012,
-0.0734242577495321));
#48049=CARTESIAN_POINT('Ctrl Pts',(-18.0888381201258,-3.93747181923847,
-0.145510539624574));
#48050=CARTESIAN_POINT('Ctrl Pts',(-18.0851754191713,-3.93349291696148,
-0.217476772047698));
#48051=CARTESIAN_POINT('Ctrl Pts',(-18.0188842419388,-3.86147881608094,
-1.5199926824495));
#48052=CARTESIAN_POINT('Ctrl Pts',(-17.9525930647063,-3.07819516685206,
-2.78318359374845));
#48053=CARTESIAN_POINT('Ctrl Pts',(-17.8863018874738,-1.943483281878,-3.42673830445617));
#48054=CARTESIAN_POINT('Ctrl Pts',(-17.8200107102413,-0.808771396903944,
-4.07029301516389));
#48055=CARTESIAN_POINT('Ctrl Pts',(-17.7537195330088,0.677368723815286,
-4.09421152528039));
#48056=CARTESIAN_POINT('Ctrl Pts',(-17.6874283557764,1.83220278309591,-3.48750564670253));
#48057=CARTESIAN_POINT('Ctrl Pts',(-17.6211371785439,2.98703684237646,-2.88079976812471));
#48058=CARTESIAN_POINT('Ctrl Pts',(-17.5548460013114,3.81056484021844,-1.64346950085261));
#48059=CARTESIAN_POINT('Ctrl Pts',(-17.4885548240789,3.92445716894955,-0.343945639959133));
#48060=CARTESIAN_POINT('Ctrl Pts',(-17.4222636468464,4.03834949768068,0.955578220934493));
#48061=CARTESIAN_POINT('Ctrl Pts',(-17.3559724696139,3.44260615730077,2.31729567544951));
#48062=CARTESIAN_POINT('Ctrl Pts',(-17.2896812923815,2.4109122499921,3.11563232699311));
#48063=CARTESIAN_POINT('Ctrl Pts',(-17.223390115149,1.37921834268355,3.91396897853661));
#48064=CARTESIAN_POINT('Ctrl Pts',(-17.1570989379165,-0.0884261315536491,
4.14892482710885));
#48065=CARTESIAN_POINT('Ctrl Pts',(-17.090807760684,-1.31778379451791,3.71256091466152));
#48066=CARTESIAN_POINT('Ctrl Pts',(-17.0245165834515,-2.54714145748224,
3.27619700221418));
#48067=CARTESIAN_POINT('Ctrl Pts',(-16.9582254062191,-3.53821230917362,
2.1685133287472));
#48068=CARTESIAN_POINT('Ctrl Pts',(-16.8919342289866,-3.83569738285571,
0.898380911039564));
#48069=CARTESIAN_POINT('Ctrl Pts',(-16.8766773266693,-3.90416351816185,
0.606060167376271));
#48070=CARTESIAN_POINT('Ctrl Pts',(-16.8614204243521,-3.93589115117029,
0.305134686198502));
#48071=CARTESIAN_POINT('Ctrl Pts',(-16.8461635220349,-3.93309862886983,
0.00362758403216595));
#48072=CARTESIAN_POINT('Origin',(-54.75,0.,0.));
#48073=CARTESIAN_POINT('',(-15.4128364779652,-3.9264779963057,1.50935765152131E-5));
#48074=CARTESIAN_POINT('',(-15.5961635220349,-3.92650423935062,-0.000338343577294592));
#48075=CARTESIAN_POINT('',(-54.75,-3.933,-4.81653586104654E-16));
#48076=CARTESIAN_POINT('Ctrl Pts',(-15.4128364779652,-3.92647818587147,
1.50931378117836E-5));
#48077=CARTESIAN_POINT('Ctrl Pts',(-15.4459361427773,-3.92650057953867,
0.6569171123658));
#48078=CARTESIAN_POINT('Ctrl Pts',(-15.4790358075893,-3.77065293631031,
1.31380914345544));
#48079=CARTESIAN_POINT('Ctrl Pts',(-15.5121354724014,-3.45887639344497,
1.88569264967426));
#48080=CARTESIAN_POINT('Ctrl Pts',(-15.5784266496339,-2.8344581651224,3.03104657039658));
#48081=CARTESIAN_POINT('Ctrl Pts',(-15.6447178268664,-1.58459240146811,
3.83542218314378));
#48082=CARTESIAN_POINT('Ctrl Pts',(-15.7110090040989,-0.283468717462426,
3.92928850561862));
#48083=CARTESIAN_POINT('Ctrl Pts',(-15.7773001813313,1.01765496654326,4.02315482809346));
#48084=CARTESIAN_POINT('Ctrl Pts',(-15.8435913585638,2.37003657090034,3.40651186029594));
#48085=CARTESIAN_POINT('Ctrl Pts',(-15.9098825357963,3.15239059816314,2.36264601470027));
#48086=CARTESIAN_POINT('Ctrl Pts',(-15.9761737130288,3.93474462542595,1.31878016910461));
#48087=CARTESIAN_POINT('Ctrl Pts',(-16.0424648902613,4.14707107559447,-0.152308554289197));
#48088=CARTESIAN_POINT('Ctrl Pts',(-16.1087560674938,3.69182695947925,-1.37480048568096));
#48089=CARTESIAN_POINT('Ctrl Pts',(-16.1750472447262,3.23658284336407,-2.59729241707265));
#48090=CARTESIAN_POINT('Ctrl Pts',(-16.2413384219587,2.11376816096522,-3.57118755646233));
#48091=CARTESIAN_POINT('Ctrl Pts',(-16.3076295991912,0.839205130099,-3.84907747697835));
#48092=CARTESIAN_POINT('Ctrl Pts',(-16.3739207764237,-0.435357900767366,
-4.12696739749439));
#48093=CARTESIAN_POINT('Ctrl Pts',(-16.4402119536562,-1.86166928010115,
-3.70885209913657));
#48094=CARTESIAN_POINT('Ctrl Pts',(-16.5065031308887,-2.78448009593333,
-2.78681417922285));
#48095=CARTESIAN_POINT('Ctrl Pts',(-16.5586142465808,-3.5098964061186,-2.06200543810343));
#48096=CARTESIAN_POINT('Ctrl Pts',(-16.610725362273,-3.92417744937094,-1.02580062171259));
#48097=CARTESIAN_POINT('Ctrl Pts',(-16.6628364779652,-3.93375005137208,
0.00358326100158748));
#48098=CARTESIAN_POINT('Ctrl Pts',(-16.8461635220349,-3.93309862886983,
0.00362758403216595));
#48099=CARTESIAN_POINT('Ctrl Pts',(-16.7951292471196,-3.92375765336736,
-1.0049124210695));
#48100=CARTESIAN_POINT('Ctrl Pts',(-16.7440949722044,-3.52817075580835,
-2.01996018179993));
#48101=CARTESIAN_POINT('Ctrl Pts',(-16.6930606972891,-2.8293643400936,-2.74123331826628));
#48102=CARTESIAN_POINT('Ctrl Pts',(-16.6267695200566,-1.92164692797642,
-3.67813396791647));
#48103=CARTESIAN_POINT('Ctrl Pts',(-16.5604783428241,-0.502312808069129,
-4.11935410526842));
#48104=CARTESIAN_POINT('Ctrl Pts',(-16.4941871655917,0.77659446780288,-3.86219674625004));
#48105=CARTESIAN_POINT('Ctrl Pts',(-16.4278959883592,2.05550174367482,-3.60503938723167));
#48106=CARTESIAN_POINT('Ctrl Pts',(-16.3616048111267,3.19398217551149,-2.64950453184305));
#48107=CARTESIAN_POINT('Ctrl Pts',(-16.2953136338942,3.6690166841218,-1.43456587363645));
#48108=CARTESIAN_POINT('Ctrl Pts',(-16.2290224566617,4.14405119273209,-0.219627215429928));
#48109=CARTESIAN_POINT('Ctrl Pts',(-16.1627312794292,3.95563977811609,1.25471524559453));
#48110=CARTESIAN_POINT('Ctrl Pts',(-16.0964401021967,3.19033883757841,2.31114706922889));
#48111=CARTESIAN_POINT('Ctrl Pts',(-16.0301489249643,2.42503789704064,3.36757889286337));
#48112=CARTESIAN_POINT('Ctrl Pts',(-15.9638577477318,1.08284743058101,4.00610007910764));
#48113=CARTESIAN_POINT('Ctrl Pts',(-15.8975665704993,-0.219628883567405,
3.93337333947203));
#48114=CARTESIAN_POINT('Ctrl Pts',(-15.8312753932668,-1.52210519771575,
3.86064659983643));
#48115=CARTESIAN_POINT('Ctrl Pts',(-15.7649842160343,-2.78486735955289,
3.07667193432105));
#48116=CARTESIAN_POINT('Ctrl Pts',(-15.6986930388018,-3.42780113553339,
1.94160810912049));
#48117=CARTESIAN_POINT('Ctrl Pts',(-15.6645165332128,-3.75926650853602,
1.3564244272893));
#48118=CARTESIAN_POINT('Ctrl Pts',(-15.6303400276238,-3.92598571797408,
0.677923637937626));
#48119=CARTESIAN_POINT('Ctrl Pts',(-15.5961635220349,-3.92650423935062,
-0.000338343577294592));
#48120=CARTESIAN_POINT('Origin',(-54.75,0.,0.));
#48121=CARTESIAN_POINT('',(-14.1628364779652,-3.93369446688928,-0.00358851098580137));
#48122=CARTESIAN_POINT('',(-14.3461635220349,-3.93434458032143,-0.00350973384803158));
#48123=CARTESIAN_POINT('',(-54.75,-3.933,-4.81653586104654E-16));
#48124=CARTESIAN_POINT('Ctrl Pts',(-14.1628364779652,-3.93369446688928,
-0.00358851098580137));
#48125=CARTESIAN_POINT('Ctrl Pts',(-14.214855746049,-3.92413817277373,1.02401828417443));
#48126=CARTESIAN_POINT('Ctrl Pts',(-14.2668750141329,-3.5114721763875,2.05842142212482));
#48127=CARTESIAN_POINT('Ctrl Pts',(-14.3188942822167,-2.78833724325426,
2.78295492095141));
#48128=CARTESIAN_POINT('Ctrl Pts',(-14.3851854594492,-1.86680436166715,
3.70627007610107));
#48129=CARTESIAN_POINT('Ctrl Pts',(-14.4514766366817,-0.441073452138983,
4.12636045584482));
#48130=CARTESIAN_POINT('Ctrl Pts',(-14.5177678139141,0.833873241785975,
3.85023610844839));
#48131=CARTESIAN_POINT('Ctrl Pts',(-14.5840589911466,2.10881993571108,3.57411176105193));
#48132=CARTESIAN_POINT('Ctrl Pts',(-14.6503501683791,3.23298241403293,2.60177268651509));
#48133=CARTESIAN_POINT('Ctrl Pts',(-14.7166413456116,3.68991928010443,1.37991245391873));
#48134=CARTESIAN_POINT('Ctrl Pts',(-14.7829325228441,4.14685614617589,0.158052221322513));
#48135=CARTESIAN_POINT('Ctrl Pts',(-14.8492237000766,3.93656739999716,-1.31332916933317));
#48136=CARTESIAN_POINT('Ctrl Pts',(-14.915514877309,3.1556599074528,-2.35827759660763));
#48137=CARTESIAN_POINT('Ctrl Pts',(-14.9818060545415,2.37475241490839,-3.40322602388214));
#48138=CARTESIAN_POINT('Ctrl Pts',(-15.048097231774,1.02322617599829,-4.02174148777539));
#48139=CARTESIAN_POINT('Ctrl Pts',(-15.1143884090065,-0.278026267596332,
-3.9296773491844));
#48140=CARTESIAN_POINT('Ctrl Pts',(-15.180679586239,-1.57927871119088,-3.8376132105934));
#48141=CARTESIAN_POINT('Ctrl Pts',(-15.2469707634715,-2.83025735946995,
-3.03496946951824));
#48142=CARTESIAN_POINT('Ctrl Pts',(-15.3132619407039,-3.45626133711414,
-1.89048148463201));
#48143=CARTESIAN_POINT('Ctrl Pts',(-15.3464534531244,-3.76969699577422,
-1.31744463793124));
#48144=CARTESIAN_POINT('Ctrl Pts',(-15.3796449655448,-3.92645573006452,
-0.658709750573194));
#48145=CARTESIAN_POINT('Ctrl Pts',(-15.4128364779652,-3.92647818587147,
1.50931378117836E-5));
#48146=CARTESIAN_POINT('Ctrl Pts',(-15.5961635220349,-3.92650423935062,
-0.000338343577294592));
#48147=CARTESIAN_POINT('Ctrl Pts',(-15.5640488503914,-3.92699147885803,
-0.637681467142005));
#48148=CARTESIAN_POINT('Ctrl Pts',(-15.5319341787479,-3.78072656664845,
-1.27481372777769));
#48149=CARTESIAN_POINT('Ctrl Pts',(-15.4998195071044,-3.48650266596134,
-1.83411063854145));
#48150=CARTESIAN_POINT('Ctrl Pts',(-15.4335283298719,-2.87916503028493,
-2.98861257611725));
#48151=CARTESIAN_POINT('Ctrl Pts',(-15.3672371526394,-1.64138436880819,
-3.8114634663832));
#48152=CARTESIAN_POINT('Ctrl Pts',(-15.3009459754069,-0.341798388164035,
-3.9246447655826));
#48153=CARTESIAN_POINT('Ctrl Pts',(-15.2346547981745,0.957787592480191,
-4.03782606478201));
#48154=CARTESIAN_POINT('Ctrl Pts',(-15.168363620942,2.31917889229184,-3.44133777291475));
#48155=CARTESIAN_POINT('Ctrl Pts',(-15.1020724437095,3.11695095048374,-2.4092072236412));
#48156=CARTESIAN_POINT('Ctrl Pts',(-15.035781266477,3.91472300867565,-1.37707667436765));
#48157=CARTESIAN_POINT('Ctrl Pts',(-14.9694900892445,4.14887582524779,0.0906961323124485));
#48158=CARTESIAN_POINT('Ctrl Pts',(-14.903198912012,3.71183935587708,1.31981486214107));
#48159=CARTESIAN_POINT('Ctrl Pts',(-14.8369077347795,3.27480288650638,2.54893359196969));
#48160=CARTESIAN_POINT('Ctrl Pts',(-14.7706165575471,2.16657713119312,3.53939824494685));
#48161=CARTESIAN_POINT('Ctrl Pts',(-14.7043253803146,0.896282139672688,
3.83618834264823));
#48162=CARTESIAN_POINT('Ctrl Pts',(-14.6380342030821,-0.374012851847812,
4.13297844034962));
#48163=CARTESIAN_POINT('Ctrl Pts',(-14.5717430258496,-1.80637707957535,
3.73609398277492));
#48164=CARTESIAN_POINT('Ctrl Pts',(-14.5054518486171,-2.74278094677474,
2.82786409718994));
#48165=CARTESIAN_POINT('Ctrl Pts',(-14.4523557397564,-3.49279631452224,
2.10041476096114));
#48166=CARTESIAN_POINT('Ctrl Pts',(-14.3992596308956,-3.9246404616156,1.04492429089517));
#48167=CARTESIAN_POINT('Ctrl Pts',(-14.3461635220349,-3.93434458032143,
-0.00350973384803158));
#48168=CARTESIAN_POINT('Origin',(-54.75,0.,0.));
#48169=CARTESIAN_POINT('',(-12.9128364779652,-3.93866223418523,0.00165032853560287));
#48170=CARTESIAN_POINT('',(-13.0961635220349,-3.93826781928793,0.00198880647917068));
#48171=CARTESIAN_POINT('',(-54.75,-3.933,-4.81653586104654E-16));
#48172=CARTESIAN_POINT('Ctrl Pts',(-12.9128364779652,-3.93866223418523,
0.00165032853560287));
#48173=CARTESIAN_POINT('Ctrl Pts',(-12.9174841720883,-3.93914537757192,
0.0931615357668376));
#48174=CARTESIAN_POINT('Ctrl Pts',(-12.9221318662114,-3.93623360589491,
0.18464145637103));
#48175=CARTESIAN_POINT('Ctrl Pts',(-12.9267795603345,-3.92982887836725,
0.275876169534834));
#48176=CARTESIAN_POINT('Ctrl Pts',(-12.993070737567,-3.83847671180549,1.57717878969641));
#48177=CARTESIAN_POINT('Ctrl Pts',(-13.0593619147995,-3.03651754266122,
2.82859640366949));
#48178=CARTESIAN_POINT('Ctrl Pts',(-13.1256530920319,-1.8923722365596,3.45522647484428));
#48179=CARTESIAN_POINT('Ctrl Pts',(-13.1919442692644,-0.748226930457651,
4.08185654601926));
#48180=CARTESIAN_POINT('Ctrl Pts',(-13.2582354464969,0.738104512601858,
4.08369907439556));
#48181=CARTESIAN_POINT('Ctrl Pts',(-13.3245266237294,1.88379990175547,3.4599076005455));
#48182=CARTESIAN_POINT('Ctrl Pts',(-13.3908178009619,3.02949529090888,2.83611612669555));
#48183=CARTESIAN_POINT('Ctrl Pts',(-13.4571089781944,3.83455462615653,1.58669065061949));
#48184=CARTESIAN_POINT('Ctrl Pts',(-13.5234001554269,3.92913282238253,0.285618518732132));
#48185=CARTESIAN_POINT('Ctrl Pts',(-13.5896913326594,4.02371101860855,-1.01545361315538));
#48186=CARTESIAN_POINT('Ctrl Pts',(-13.6559825098918,3.40780807581275,-2.3681724008542));
#48187=CARTESIAN_POINT('Ctrl Pts',(-13.7222736871243,2.36437043822387,-3.15109744454523));
#48188=CARTESIAN_POINT('Ctrl Pts',(-13.7885648643568,1.32093280063517,-3.93402248823613));
#48189=CARTESIAN_POINT('Ctrl Pts',(-13.8548560415893,-0.150039531746455,
-4.14715378791947));
#48190=CARTESIAN_POINT('Ctrl Pts',(-13.9211472188218,-1.37278035927145,
-3.69257860571241));
#48191=CARTESIAN_POINT('Ctrl Pts',(-13.9874383960543,-2.59552118679665,
-3.23800342350527));
#48192=CARTESIAN_POINT('Ctrl Pts',(-14.0537295732867,-3.57003050946513,
-2.11572175940747));
#48193=CARTESIAN_POINT('Ctrl Pts',(-14.1200207505192,-3.84861774397631,
-0.841310962080693));
#48194=CARTESIAN_POINT('Ctrl Pts',(-14.1342926596679,-3.90859513262605,
-0.566941492765959));
#48195=CARTESIAN_POINT('Ctrl Pts',(-14.1485645688166,-3.93631631387865,
-0.28552079033751));
#48196=CARTESIAN_POINT('Ctrl Pts',(-14.1628364779652,-3.93369446688928,
-0.00358851098580137));
#48197=CARTESIAN_POINT('Ctrl Pts',(-14.3461635220349,-3.93434458032143,
-0.00350973384803158));
#48198=CARTESIAN_POINT('Ctrl Pts',(-14.3329684536631,-3.93675617907242,
-0.264059121299957));
#48199=CARTESIAN_POINT('Ctrl Pts',(-14.3197733852914,-3.91309697321702,
-0.524172712108927));
#48200=CARTESIAN_POINT('Ctrl Pts',(-14.3065783169196,-3.86177126764843,
-0.778707487142311));
#48201=CARTESIAN_POINT('Ctrl Pts',(-14.2402871396872,-3.60391421465153,
-2.05747387229453));
#48202=CARTESIAN_POINT('Ctrl Pts',(-14.1739959624547,-2.64775660198649,
-3.19543132900379));
#48203=CARTESIAN_POINT('Ctrl Pts',(-14.1077047852222,-1.4325582185377,-3.66980103338948));
#48204=CARTESIAN_POINT('Ctrl Pts',(-14.0414136079897,-0.217359835088917,
-4.14417073777518));
#48205=CARTESIAN_POINT('Ctrl Pts',(-13.9751224307572,1.25687931914355,-3.95495268983729));
#48206=CARTESIAN_POINT('Ctrl Pts',(-13.9088312535247,2.31289226319796,-3.18907385505658));
#48207=CARTESIAN_POINT('Ctrl Pts',(-13.8425400762923,3.36890520725237,-2.42319502027587));
#48208=CARTESIAN_POINT('Ctrl Pts',(-13.7762488990598,4.00669194112866,-1.08065539865238));
#48209=CARTESIAN_POINT('Ctrl Pts',(-13.7099577218273,3.93325258450909,0.221780929340192));
#48210=CARTESIAN_POINT('Ctrl Pts',(-13.6436665445948,3.85981322788952,1.52421725733269));
#48211=CARTESIAN_POINT('Ctrl Pts',(-13.5773753673623,3.07514778077402,2.78655029169444));
#48212=CARTESIAN_POINT('Ctrl Pts',(-13.5110841901298,1.9397323551336,3.4288629404825));
#48213=CARTESIAN_POINT('Ctrl Pts',(-13.4447930128974,0.804316929493125,
4.07117558927059));
#48214=CARTESIAN_POINT('Ctrl Pts',(-13.3785018356649,-0.681848474672325,
4.0934678524851));
#48215=CARTESIAN_POINT('Ctrl Pts',(-13.3122106584324,-1.83601794493788,
3.48549864151925));
#48216=CARTESIAN_POINT('Ctrl Pts',(-13.2459194811999,-2.99018741520344,
2.87752943055339));
#48217=CARTESIAN_POINT('Ctrl Pts',(-13.1796283039674,-3.81236095156904,
1.63929874540721));
#48218=CARTESIAN_POINT('Ctrl Pts',(-13.1133371267349,-3.92483118735515,
0.339651034049346));
#48219=CARTESIAN_POINT('Ctrl Pts',(-13.1076125918349,-3.93454348719428,
0.227420734453008));
#48220=CARTESIAN_POINT('Ctrl Pts',(-13.1018880569349,-3.93896347092205,
0.114732443021119));
#48221=CARTESIAN_POINT('Ctrl Pts',(-13.0961635220349,-3.93826781928793,
0.00198880647917068));
#48222=CARTESIAN_POINT('Origin',(-54.75,0.,0.));
#48223=CARTESIAN_POINT('',(-11.6628364779652,-3.92862917326101,0.00277744209242731));
#48224=CARTESIAN_POINT('',(-11.8461635220349,-3.92818995496044,0.00253348489050703));
#48225=CARTESIAN_POINT('',(-54.75,-3.933,-4.81653586104654E-16));
#48226=CARTESIAN_POINT('Ctrl Pts',(-11.6628364779652,-3.92862917326101,
0.00277744209242731));
#48227=CARTESIAN_POINT('Ctrl Pts',(-11.6864037753601,-3.93165944827161,
0.469857995963653));
#48228=CARTESIAN_POINT('Ctrl Pts',(-11.7099710727549,-3.8546981368583,0.93597264351165));
#48229=CARTESIAN_POINT('Ctrl Pts',(-11.7335383701498,-3.69332914655501,
1.37075982191401));
#48230=CARTESIAN_POINT('Ctrl Pts',(-11.7998295473823,-3.23942303433508,
2.59374917953944));
#48231=CARTESIAN_POINT('Ctrl Pts',(-11.8661207246148,-2.11767472449869,
3.5688723937627));
#48232=CARTESIAN_POINT('Ctrl Pts',(-11.9324119018472,-0.843416542212277,
3.84815685887272));
#48233=CARTESIAN_POINT('Ctrl Pts',(-11.9987030790797,0.430841640074067,
4.12744132398272));
#48234=CARTESIAN_POINT('Ctrl Pts',(-12.0649942563122,1.85760969481043,3.71088703997956));
#48235=CARTESIAN_POINT('Ctrl Pts',(-12.1312854335447,2.78142891287907,2.78985947258402));
#48236=CARTESIAN_POINT('Ctrl Pts',(-12.1975766107772,3.70524813094765,1.86883190518855));
#48237=CARTESIAN_POINT('Ctrl Pts',(-12.2638677880097,4.12611851234857,0.443331054400757));
#48238=CARTESIAN_POINT('Ctrl Pts',(-12.3301589652421,3.85069177178547,-0.831766525456592));
#48239=CARTESIAN_POINT('Ctrl Pts',(-12.3964501424746,3.57526503122234,-2.10686410531409));
#48240=CARTESIAN_POINT('Ctrl Pts',(-12.4627413197071,2.60354116869499,-3.2315584142411));
#48241=CARTESIAN_POINT('Ctrl Pts',(-12.5290324969396,1.38193112425552,-3.68916373206453));
#48242=CARTESIAN_POINT('Ctrl Pts',(-12.5953236741721,0.160321079816128,
-4.14676904988794));
#48243=CARTESIAN_POINT('Ctrl Pts',(-12.6616148514046,-1.31117514653535,
-3.93728537660784));
#48244=CARTESIAN_POINT('Ctrl Pts',(-12.7279060286371,-2.35655067772163,
-3.15694972679265));
#48245=CARTESIAN_POINT('Ctrl Pts',(-12.7895495117465,-3.32863461995813,
-2.43132364113208));
#48246=CARTESIAN_POINT('Ctrl Pts',(-12.8511929948558,-3.93225418744031,
-1.2120847856676));
#48247=CARTESIAN_POINT('Ctrl Pts',(-12.9128364779652,-3.93866223418523,
0.00165032853560287));
#48248=CARTESIAN_POINT('Ctrl Pts',(-13.0961635220349,-3.93826781928793,
0.00198880647917068));
#48249=CARTESIAN_POINT('Ctrl Pts',(-13.0355968797024,-3.93090769581103,
-1.19085980549745));
#48250=CARTESIAN_POINT('Ctrl Pts',(-12.9750302373699,-3.35090166376052,
-2.38990376733619));
#48251=CARTESIAN_POINT('Ctrl Pts',(-12.9144635950375,-2.40750147608245,
-3.11826864090111));
#48252=CARTESIAN_POINT('Ctrl Pts',(-12.848172417805,-1.37493459381688,-3.91547586692441));
#48253=CARTESIAN_POINT('Ctrl Pts',(-12.7818812405725,0.0929661059210794,
-4.14882558140152));
#48254=CARTESIAN_POINT('Ctrl Pts',(-12.71559006334,1.32184553467154,-3.71111668593637));
#48255=CARTESIAN_POINT('Ctrl Pts',(-12.6492988861076,2.55072496342201,-3.27340779047122));
#48256=CARTESIAN_POINT('Ctrl Pts',(-12.5830077088751,3.540583121185,-2.16464028506394));
#48257=CARTESIAN_POINT('Ctrl Pts',(-12.5167165316426,3.83667815406009,-0.894183099999397));
#48258=CARTESIAN_POINT('Ctrl Pts',(-12.4504253544101,4.13277318693521,0.376274085065291));
#48259=CARTESIAN_POINT('Ctrl Pts',(-12.3841341771776,3.73510509492216,1.80842094978705));
#48260=CARTESIAN_POINT('Ctrl Pts',(-12.3178429999451,2.82636300775224,2.74432775421889));
#48261=CARTESIAN_POINT('Ctrl Pts',(-12.2515518227126,1.91762092058248,3.68023455865058));
#48262=CARTESIAN_POINT('Ctrl Pts',(-12.1852606454802,0.497804838255918,
4.11990130279241));
#48263=CARTESIAN_POINT('Ctrl Pts',(-12.1189694682477,-0.780820273371836,
3.86134463300778));
#48264=CARTESIAN_POINT('Ctrl Pts',(-12.0526782910152,-2.05944538499966,
3.60278796322313));
#48265=CARTESIAN_POINT('Ctrl Pts',(-11.9863871137827,-3.19687952592881,
2.64600787951188));
#48266=CARTESIAN_POINT('Ctrl Pts',(-11.9200959365502,-3.67058428408519,
1.43055013459624));
#48267=CARTESIAN_POINT('Ctrl Pts',(-11.8954517983784,-3.8466868364911,0.978696511562696));
#48268=CARTESIAN_POINT('Ctrl Pts',(-11.8708076602067,-3.93106034832633,
0.491092996637599));
#48269=CARTESIAN_POINT('Ctrl Pts',(-11.8461635220349,-3.92818995496044,
0.00253348489050703));
#48270=CARTESIAN_POINT('Origin',(-54.75,0.,0.));
#48271=CARTESIAN_POINT('',(-10.4128364779653,-3.92852884447977,-0.00272592851332826));
#48272=CARTESIAN_POINT('',(-10.5961635220349,-3.92900062987189,-0.00294957216901129));
#48273=CARTESIAN_POINT('',(-54.75,-3.933,-4.81653586104654E-16));
#48274=CARTESIAN_POINT('Ctrl Pts',(-10.4128364779653,-3.92852884447977,
-0.00272592851332826));
#48275=CARTESIAN_POINT('Ctrl Pts',(-10.4553233786319,-3.92317581591888,
0.839376464306679));
#48276=CARTESIAN_POINT('Ctrl Pts',(-10.4978102792985,-3.6579994874255,1.68455438064328));
#48277=CARTESIAN_POINT('Ctrl Pts',(-10.5402971799651,-3.15823860108501,
2.35482305339129));
#48278=CARTESIAN_POINT('Ctrl Pts',(-10.6065883571976,-2.37847502759617,
3.40062537555125));
#48279=CARTESIAN_POINT('Ctrl Pts',(-10.67287953443,-1.02762641829007,4.02061939832335));
#48280=CARTESIAN_POINT('Ctrl Pts',(-10.7391707116625,0.273725988887863,
3.92997923113772));
#48281=CARTESIAN_POINT('Ctrl Pts',(-10.805461888895,1.57507839606587,3.83933906395208));
#48282=CARTESIAN_POINT('Ctrl Pts',(-10.8717530661275,2.82693460111579,3.03806470680862));
#48283=CARTESIAN_POINT('Ctrl Pts',(-10.93804424336,3.45419057823663,1.89426242199642));
#48284=CARTESIAN_POINT('Ctrl Pts',(-11.0043354205925,4.0814465553575,0.750460137184154));
#48285=CARTESIAN_POINT('Ctrl Pts',(-11.0706265978249,4.0841023045493,-0.735870075296754));
#48286=CARTESIAN_POINT('Ctrl Pts',(-11.1369177750574,3.4609377719068,-1.88190658991227));
#48287=CARTESIAN_POINT('Ctrl Pts',(-11.2032089522899,2.83777323926437,-3.02794310452766));
#48288=CARTESIAN_POINT('Ctrl Pts',(-11.2695001295224,1.58878842478775,-3.83368592127761));
#48289=CARTESIAN_POINT('Ctrl Pts',(-11.3357913067549,0.287768234500619,
-3.92897596294236));
#48290=CARTESIAN_POINT('Ctrl Pts',(-11.4020824839874,-1.01325195578666,
-4.02426600460712));
#48291=CARTESIAN_POINT('Ctrl Pts',(-11.4683736612199,-2.36630752188455,
-3.40910327118653));
#48292=CARTESIAN_POINT('Ctrl Pts',(-11.5346648384523,-3.1498033476316,-2.36609415396244));
#48293=CARTESIAN_POINT('Ctrl Pts',(-11.57738871829,-3.65475714254024,-1.69388711142402));
#48294=CARTESIAN_POINT('Ctrl Pts',(-11.6201125981276,-3.92313575145455,
-0.843967652339101));
#48295=CARTESIAN_POINT('Ctrl Pts',(-11.6628364779652,-3.92862917326101,
0.00277744209242731));
#48296=CARTESIAN_POINT('Ctrl Pts',(-11.8461635220349,-3.92818995496044,
0.00253348489050703));
#48297=CARTESIAN_POINT('Ctrl Pts',(-11.8045164829742,-3.92333917122454,
-0.823101273662933));
#48298=CARTESIAN_POINT('Ctrl Pts',(-11.7628694439135,-3.66932966957637,
-1.65146625092852));
#48299=CARTESIAN_POINT('Ctrl Pts',(-11.7212224048528,-3.18780791787102,
-2.31463676479168));
#48300=CARTESIAN_POINT('Ctrl Pts',(-11.6549312276203,-2.4213514181168,-3.37023051314387));
#48301=CARTESIAN_POINT('Ctrl Pts',(-11.5886400503878,-1.07846304322473,
-4.00728260372794));
#48302=CARTESIAN_POINT('Ctrl Pts',(-11.5223488731553,0.22393290872183,-3.9331306521088));
#48303=CARTESIAN_POINT('Ctrl Pts',(-11.4560576959228,1.52632886066824,-3.85897870048967));
#48304=CARTESIAN_POINT('Ctrl Pts',(-11.3897665186903,2.78823238966908,-3.07362270666749));
#48305=CARTESIAN_POINT('Ctrl Pts',(-11.3234753414579,3.42992371898552,-1.93785602047907));
#48306=CARTESIAN_POINT('Ctrl Pts',(-11.2571841642254,4.071615048302,-0.802089334290585));
#48307=CARTESIAN_POINT('Ctrl Pts',(-11.1908929869929,4.09309417793392,0.684088044264345));
#48308=CARTESIAN_POINT('Ctrl Pts',(-11.1246018097604,3.48449357367713,1.83792470171366));
#48309=CARTESIAN_POINT('Ctrl Pts',(-11.0583106325279,2.87589296942037,2.99176135916291));
#48310=CARTESIAN_POINT('Ctrl Pts',(-10.9920194552954,1.63721263127506,3.81325729550672));
#48311=CARTESIAN_POINT('Ctrl Pts',(-10.925728278063,0.337503578259211,3.92501643421129));
#48312=CARTESIAN_POINT('Ctrl Pts',(-10.8594371008305,-0.962205474756632,
4.03677557291586));
#48313=CARTESIAN_POINT('Ctrl Pts',(-10.793145923598,-2.32294324264293,3.43879791398117));
#48314=CARTESIAN_POINT('Ctrl Pts',(-10.7268547463655,-3.11958539785007,
2.40579500782736));
#48315=CARTESIAN_POINT('Ctrl Pts',(-10.683291004922,-3.64310473060778,1.72694944507178));
#48316=CARTESIAN_POINT('Ctrl Pts',(-10.6397272634784,-3.92301603181814,
0.860235652593407));
#48317=CARTESIAN_POINT('Ctrl Pts',(-10.5961635220349,-3.92900062987189,
-0.00294957216901129));
#48318=CARTESIAN_POINT('Origin',(-54.75,0.,0.));
#48319=CARTESIAN_POINT('',(-9.16283647796523,-3.93858084194566,-0.00172678509975766));
#48320=CARTESIAN_POINT('',(-9.34616352203489,-3.93892425866043,-0.00137129965302642));
#48321=CARTESIAN_POINT('',(-54.75,-3.933,-4.81653586104654E-16));
#48322=CARTESIAN_POINT('Ctrl Pts',(-9.16283647796523,-3.93858084194566,
-0.00172678509975766));
#48323=CARTESIAN_POINT('Ctrl Pts',(-9.22424298190359,-3.93194753706968,
1.20740853644141));
#48324=CARTESIAN_POINT('Ctrl Pts',(-9.28564948584196,-3.33357479351524,
2.42221595869824));
#48325=CARTESIAN_POINT('Ctrl Pts',(-9.34705598978033,-2.36781716140013,
3.1485083078095));
#48326=CARTESIAN_POINT('Ctrl Pts',(-9.41334716701282,-1.32523687677053,
3.93257468106957));
#48327=CARTESIAN_POINT('Ctrl Pts',(-9.4796383442453,0.145501352595422,4.14731548813625));
#48328=CARTESIAN_POINT('Ctrl Pts',(-9.54592952147779,1.36873887421348,3.69407858178237));
#48329=CARTESIAN_POINT('Ctrl Pts',(-9.61222069871027,2.59197639583146,3.24084167542852));
#48330=CARTESIAN_POINT('Ctrl Pts',(-9.67851187594275,3.56771320970172,2.11962705565427));
#48331=CARTESIAN_POINT('Ctrl Pts',(-9.74480305317524,3.84769482180553,0.845521869863438));
#48332=CARTESIAN_POINT('Ctrl Pts',(-9.81109423040773,4.12767643390936,-0.428583315927544));
#48333=CARTESIAN_POINT('Ctrl Pts',(-9.87738540764022,3.71190284424656,-1.85557906773504));
#48334=CARTESIAN_POINT('Ctrl Pts',(-9.94367658487271,2.79138086675646,-2.77990207217312));
#48335=CARTESIAN_POINT('Ctrl Pts',(-10.0099677621052,1.87085888926651,-3.70422507661104));
#48336=CARTESIAN_POINT('Ctrl Pts',(-10.0762589393377,0.445588523949287,
-4.12587533367967));
#48337=CARTESIAN_POINT('Ctrl Pts',(-10.1425501165701,-0.829659560134056,
-3.85114628240017));
#48338=CARTESIAN_POINT('Ctrl Pts',(-10.2088412938026,-2.10490764421762,
-3.57641723112061));
#48339=CARTESIAN_POINT('Ctrl Pts',(-10.2751324710351,-3.23013344706731,
-2.60530887149283));
#48340=CARTESIAN_POINT('Ctrl Pts',(-10.3414236482676,-3.68840707965641,
-1.38394938090485));
#48341=CARTESIAN_POINT('Ctrl Pts',(-10.3652279248335,-3.85296702184515,
-0.945375496504573));
#48342=CARTESIAN_POINT('Ctrl Pts',(-10.3890322013994,-3.93152800352243,
-0.474533425435142));
#48343=CARTESIAN_POINT('Ctrl Pts',(-10.4128364779653,-3.92852884447977,
-0.00272592851332826));
#48344=CARTESIAN_POINT('Ctrl Pts',(-10.5961635220349,-3.92900062987189,
-0.00294957216901129));
#48345=CARTESIAN_POINT('Ctrl Pts',(-10.5734360862459,-3.93212282653091,
-0.453277898425794));
#48346=CARTESIAN_POINT('Ctrl Pts',(-10.550708650457,-3.86068862727375,-0.902645831670076));
#48347=CARTESIAN_POINT('Ctrl Pts',(-10.527981214668,-3.71039290505572,-1.32387581150145));
#48348=CARTESIAN_POINT('Ctrl Pts',(-10.4616900374356,-3.27201171452627,
-2.5525155713031));
#48349=CARTESIAN_POINT('Ctrl Pts',(-10.3953988602031,-2.16270279093953,
-3.54176693753334));
#48350=CARTESIAN_POINT('Ctrl Pts',(-10.3291076829706,-0.892083792648041,
-3.83716681694465));
#48351=CARTESIAN_POINT('Ctrl Pts',(-10.2628165057381,0.378535205643446,
-4.13256669635596));
#48352=CARTESIAN_POINT('Ctrl Pts',(-10.1965253285056,1.81046427863968,-3.73411508894833));
#48353=CARTESIAN_POINT('Ctrl Pts',(-10.1302341512731,2.74587374013584,-2.82486107222972));
#48354=CARTESIAN_POINT('Ctrl Pts',(-10.0639429740407,3.68128320163195,-1.91560705551115));
#48355=CARTESIAN_POINT('Ctrl Pts',(-9.99765179680817,4.12017305162805,-0.49555062948166));
#48356=CARTESIAN_POINT('Ctrl Pts',(-9.93136061957568,3.86091684245572,0.782932825859423));
#48357=CARTESIAN_POINT('Ctrl Pts',(-9.86506944234319,3.60166063328335,2.06141628120065));
#48358=CARTESIAN_POINT('Ctrl Pts',(-9.79877826511069,2.64425836494236,3.19832676585343));
#48359=CARTESIAN_POINT('Ctrl Pts',(-9.73248708787821,1.42854162241256,3.67136643597467));
#48360=CARTESIAN_POINT('Ctrl Pts',(-9.66619591064573,0.212824879882835,
4.14440610609588));
#48361=CARTESIAN_POINT('Ctrl Pts',(-9.59990473341325,-1.26120633683568,
3.95357496168562));
#48362=CARTESIAN_POINT('Ctrl Pts',(-9.53361355618077,-2.31638057348854,
3.18654102640015));
#48363=CARTESIAN_POINT('Ctrl Pts',(-9.47113021146548,-3.31094453080447,
2.46356629902905));
#48364=CARTESIAN_POINT('Ctrl Pts',(-9.40864686675018,-3.93338864221481,
1.22868296333715));
#48365=CARTESIAN_POINT('Ctrl Pts',(-9.34616352203489,-3.93892425866043,
-0.00137129965302642));
#48366=CARTESIAN_POINT('Origin',(-54.75,0.,0.));
#48367=CARTESIAN_POINT('',(-7.91283647796524,-3.933837855893,0.00357440632912626));
#48368=CARTESIAN_POINT('',(-8.09616352203487,-3.93318629788295,0.00362380460979597));
#48369=CARTESIAN_POINT('',(-54.75,-3.933,-4.81653586104654E-16));
#48370=CARTESIAN_POINT('Ctrl Pts',(-7.91283647796524,-3.933837855893,0.00357440632912626));
#48371=CARTESIAN_POINT('Ctrl Pts',(-7.92687140794288,-3.93641540935061,
0.28079939536921));
#48372=CARTESIAN_POINT('Ctrl Pts',(-7.94090633792052,-3.90961655860019,
0.557529618388759));
#48373=CARTESIAN_POINT('Ctrl Pts',(-7.95494126789816,-3.85159964015645,
0.827552346449105));
#48374=CARTESIAN_POINT('Ctrl Pts',(-8.02123244513065,-3.57756836040193,
2.10295055300727));
#48375=CARTESIAN_POINT('Ctrl Pts',(-8.08752362236314,-2.60707579437936,
3.22870751293816));
#48376=CARTESIAN_POINT('Ctrl Pts',(-8.15381479959562,-1.38596722326251,
3.68764932310658));
#48377=CARTESIAN_POINT('Ctrl Pts',(-8.2201059768281,-0.164858652145793,
4.14659113327494));
#48378=CARTESIAN_POINT('Ctrl Pts',(-8.28639715406057,1.30686592406514,3.93871779368097));
#48379=CARTESIAN_POINT('Ctrl Pts',(-8.35268833129305,2.35309472413324,3.15952652994444));
#48380=CARTESIAN_POINT('Ctrl Pts',(-8.41897950852553,3.39932352420134,2.3803352662079));
#48381=CARTESIAN_POINT('Ctrl Pts',(-8.48527068575802,4.0200565481266,1.0298260783288));
#48382=CARTESIAN_POINT('Ctrl Pts',(-8.5515618629905,3.93012840745075,-0.271575726299527));
#48383=CARTESIAN_POINT('Ctrl Pts',(-8.617853040223,3.84020026677489,-1.572977530928));
#48384=CARTESIAN_POINT('Ctrl Pts',(-8.68414421745548,3.03961096149769,-2.82527195230569));
#48385=CARTESIAN_POINT('Ctrl Pts',(-8.75043539468797,1.89615204037761,-3.45315364760073));
#48386=CARTESIAN_POINT('Ctrl Pts',(-8.81672657192046,0.752693119257527,
-4.08103534289578));
#48387=CARTESIAN_POINT('Ctrl Pts',(-8.88301774915295,-0.733635417705434,
-4.08450431210817));
#48388=CARTESIAN_POINT('Ctrl Pts',(-8.94930892638544,-1.88001271471163,
-3.46196690722038));
#48389=CARTESIAN_POINT('Ctrl Pts',(-9.01560010361792,-3.0263900117177,-2.83942950233266));
#48390=CARTESIAN_POINT('Ctrl Pts',(-9.08189128085039,-3.83281606876708,
-1.59088572334489));
#48391=CARTESIAN_POINT('Ctrl Pts',(-9.14818245808288,-3.92881792734507,
-0.289917864124349));
#48392=CARTESIAN_POINT('Ctrl Pts',(-9.15306713137699,-3.93589183573467,
-0.19405589238482));
#48393=CARTESIAN_POINT('Ctrl Pts',(-9.15795180467111,-3.93910849822148,
-0.0979092842701217));
#48394=CARTESIAN_POINT('Ctrl Pts',(-9.16283647796523,-3.93858084194566,
-0.00172678509975766));
#48395=CARTESIAN_POINT('Ctrl Pts',(-9.34616352203489,-3.93892425866043,
-0.00137129965302642));
#48396=CARTESIAN_POINT('Ctrl Pts',(-9.34235568951769,-3.93926160776363,
-0.0763327256438075));
#48397=CARTESIAN_POINT('Ctrl Pts',(-9.33854785700049,-3.9373078365908,-0.151276217068159));
#48398=CARTESIAN_POINT('Ctrl Pts',(-9.3347400244833,-3.93300754230767,-0.226084821068116));
#48399=CARTESIAN_POINT('Ctrl Pts',(-9.26844884725081,-3.85814301788671,
-1.52844000709018));
#48400=CARTESIAN_POINT('Ctrl Pts',(-9.20215767001835,-3.07209671245766,
-2.78991365297364));
#48401=CARTESIAN_POINT('Ctrl Pts',(-9.13586649278587,-1.93597910571819,
-3.43098347072513));
#48402=CARTESIAN_POINT('Ctrl Pts',(-9.06957531555338,-0.799861498978523,
-4.07205328847674));
#48403=CARTESIAN_POINT('Ctrl Pts',(-9.00328413832087,0.686327409071799,
-4.09271927809607));
#48404=CARTESIAN_POINT('Ctrl Pts',(-8.93699296108838,1.83983090829858,-3.48348746273554));
#48405=CARTESIAN_POINT('Ctrl Pts',(-8.8707017838559,2.99333440752502,-2.87425564737518));
#48406=CARTESIAN_POINT('Ctrl Pts',(-8.80441060662344,3.8141524979283,-1.63512602703546));
#48407=CARTESIAN_POINT('Ctrl Pts',(-8.73811942939096,3.92520050609562,-0.335356021435604));
#48408=CARTESIAN_POINT('Ctrl Pts',(-8.67182825215848,4.03624851426296,0.964413984164396));
#48409=CARTESIAN_POINT('Ctrl Pts',(-8.60553707492599,3.43752644019418,2.32482437502443));
#48410=CARTESIAN_POINT('Ctrl Pts',(-8.53924589769351,2.40408781938623,3.12090122093686));
#48411=CARTESIAN_POINT('Ctrl Pts',(-8.47295472046101,1.3706491985781,3.91697806684944));
#48412=CARTESIAN_POINT('Ctrl Pts',(-8.40666354322852,-0.0975059689694893,
4.14872136781416));
#48413=CARTESIAN_POINT('Ctrl Pts',(-8.34037236599602,-1.32590569202342,
3.70966801345165));
#48414=CARTESIAN_POINT('Ctrl Pts',(-8.27408118876355,-2.554305415077,3.27061465908927));
#48415=CARTESIAN_POINT('Ctrl Pts',(-8.20779001153107,-3.54294969363718,
2.16076464940022));
#48416=CARTESIAN_POINT('Ctrl Pts',(-8.14149883429859,-3.83765433115549,
0.889984218247712));
#48417=CARTESIAN_POINT('Ctrl Pts',(-8.12638706354402,-3.90483535144222,
0.600296459533917));
#48418=CARTESIAN_POINT('Ctrl Pts',(-8.11127529278945,-3.9359551075444,0.3022457912809));
#48419=CARTESIAN_POINT('Ctrl Pts',(-8.09616352203487,-3.93318629788295,
0.00362380460979597));
#48420=CARTESIAN_POINT('Origin',(-54.75,0.,0.));
#48421=CARTESIAN_POINT('',(-6.66283647796524,-3.92647855971048,6.27931888395146E-5));
#48422=CARTESIAN_POINT('',(-6.84616352203489,-3.92649740926382,-0.000290818540083879));
#48423=CARTESIAN_POINT('',(-54.75,-3.933,-4.81653586104654E-16));
#48424=CARTESIAN_POINT('Ctrl Pts',(-6.66283647796524,-3.92647903110527,
6.27886499063313E-5));
#48425=CARTESIAN_POINT('Ctrl Pts',(-6.69579101121463,-3.92657178318442,
0.65408414937199));
#48426=CARTESIAN_POINT('Ctrl Pts',(-6.72874554446403,-3.77215766733763,
1.30806432167412));
#48427=CARTESIAN_POINT('Ctrl Pts',(-6.76170007771342,-3.46299500617961,
1.87811827672048));
#48428=CARTESIAN_POINT('Ctrl Pts',(-6.82799125494591,-2.84108491540716,
3.02483601294439));
#48429=CARTESIAN_POINT('Ctrl Pts',(-6.89428243217839,-1.59298254566306,
3.83194506888531));
#48430=CARTESIAN_POINT('Ctrl Pts',(-6.96057360941088,-0.292067406959177,
3.92865871563777));
#48431=CARTESIAN_POINT('Ctrl Pts',(-7.02686478664336,1.00884773174456,4.02537236239023));
#48432=CARTESIAN_POINT('Ctrl Pts',(-7.09315596387586,2.36257563940807,3.41169059995439));
#48433=CARTESIAN_POINT('Ctrl Pts',(-7.15944714110833,3.14721232546681,2.36953946002056));
#48434=CARTESIAN_POINT('Ctrl Pts',(-7.22573831834082,3.93184901152565,1.32738832008662));
#48435=CARTESIAN_POINT('Ctrl Pts',(-7.2920294955733,4.14739447597958,-0.143232197345431));
#48436=CARTESIAN_POINT('Ctrl Pts',(-7.35832067280579,3.6948269111705,-1.36671751677449));
#48437=CARTESIAN_POINT('Ctrl Pts',(-7.42461185003827,3.24225934636147,-2.59020283620341));
#48438=CARTESIAN_POINT('Ctrl Pts',(-7.49090302727077,2.12157875228958,-3.5665529576294));
#48439=CARTESIAN_POINT('Ctrl Pts',(-7.55719420450325,0.847626944403404,
-3.84723163291313));
#48440=CARTESIAN_POINT('Ctrl Pts',(-7.62348538173574,-0.426324863482916,
-4.12791030819688));
#48441=CARTESIAN_POINT('Ctrl Pts',(-7.68977655896822,-1.85354788518356,
-3.71291753733821));
#48442=CARTESIAN_POINT('Ctrl Pts',(-7.7560677362007,-2.77837439929059,-2.79290142531614));
#48443=CARTESIAN_POINT('Ctrl Pts',(-7.80832398345555,-3.50739996508378,
-2.06766782055368));
#48444=CARTESIAN_POINT('Ctrl Pts',(-7.8605802307104,-3.92424085248734,-1.0286172466098));
#48445=CARTESIAN_POINT('Ctrl Pts',(-7.91283647796524,-3.933837855893,0.00357440632912626));
#48446=CARTESIAN_POINT('Ctrl Pts',(-8.09616352203487,-3.93318629788295,
0.00362380460979597));
#48447=CARTESIAN_POINT('Ctrl Pts',(-8.04498411555696,-3.92380910195901,
-1.00772663785624));
#48448=CARTESIAN_POINT('Ctrl Pts',(-7.99380470907904,-3.52573331557938,
-2.02563004763744));
#48449=CARTESIAN_POINT('Ctrl Pts',(-7.94262530260113,-2.82335829107196,
-2.74741890406279));
#48450=CARTESIAN_POINT('Ctrl Pts',(-7.87633412536865,-1.91359261699404,
-3.68233074260415));
#48451=CARTESIAN_POINT('Ctrl Pts',(-7.81004294813616,-0.493296272362007,
-4.12044356707083));
#48452=CARTESIAN_POINT('Ctrl Pts',(-7.74375177090368,0.785045143972438,
-3.86048789612034));
#48453=CARTESIAN_POINT('Ctrl Pts',(-7.67746059367119,2.0633865603071,-3.60053222516981));
#48454=CARTESIAN_POINT('Ctrl Pts',(-7.61116941643871,3.19977304834405,-2.64250805880205));
#48455=CARTESIAN_POINT('Ctrl Pts',(-7.54487823920622,3.67214748882358,-1.42653268258857));
#48456=CARTESIAN_POINT('Ctrl Pts',(-7.47858706197375,4.14452192930298,-0.210557306375435));
#48457=CARTESIAN_POINT('Ctrl Pts',(-7.41229588474128,3.95288432222515,1.26336927968317));
#48458=CARTESIAN_POINT('Ctrl Pts',(-7.34600470750881,3.18527318102397,2.31812368876547));
#48459=CARTESIAN_POINT('Ctrl Pts',(-7.27971353027631,2.41766203982253,3.37287809784814));
#48460=CARTESIAN_POINT('Ctrl Pts',(-7.21342235304382,1.07407736449723,4.00846032995424));
#48461=CARTESIAN_POINT('Ctrl Pts',(-7.14713117581133,-0.228236665734775,
3.93288325514251));
#48462=CARTESIAN_POINT('Ctrl Pts',(-7.08083999857884,-1.53055069596648,
3.85730618033079));
#48463=CARTESIAN_POINT('Ctrl Pts',(-7.01454882134635,-2.79159408110498,
3.07056979860157));
#48464=CARTESIAN_POINT('Ctrl Pts',(-6.94825764411387,-3.43204219538415,
1.93410161141309));
#48465=CARTESIAN_POINT('Ctrl Pts',(-6.91422627008754,-3.76082394631091,
1.35068198361555));
#48466=CARTESIAN_POINT('Ctrl Pts',(-6.88019489606122,-3.9260536565938,0.675093831262958));
#48467=CARTESIAN_POINT('Ctrl Pts',(-6.84616352203489,-3.92649740926382,
-0.000290818540083879));
#48468=CARTESIAN_POINT('Origin',(-54.75,0.,0.));
#48469=CARTESIAN_POINT('',(-5.41283647796527,-3.93360662039214,-0.00359624771770317));
#48470=CARTESIAN_POINT('',(-5.59616352203489,-3.93425725830108,-0.00352254436509695));
#48471=CARTESIAN_POINT('',(-54.75,-3.933,-4.81653586104654E-16));
#48472=CARTESIAN_POINT('Ctrl Pts',(-5.41283647796527,-3.93360662039214,
-0.00359624771770317));
#48473=CARTESIAN_POINT('Ctrl Pts',(-5.46471061448641,-3.92407744450487,
1.02120223617962));
#48474=CARTESIAN_POINT('Ctrl Pts',(-5.51658475100756,-3.51395559821539,
2.05275735647589));
#48475=CARTESIAN_POINT('Ctrl Pts',(-5.56845888752871,-2.79442114786394,
2.776845894706));
#48476=CARTESIAN_POINT('Ctrl Pts',(-5.63475006476119,-1.87491117676923,
3.70217564164551));
#48477=CARTESIAN_POINT('Ctrl Pts',(-5.70104124199368,-0.450103062199543,
4.1253852711142));
#48478=CARTESIAN_POINT('Ctrl Pts',(-5.76733241922616,0.825444885062228,
3.85205184490948));
#48479=CARTESIAN_POINT('Ctrl Pts',(-5.83362359645865,2.10099283232414,3.57871841870473));
#48480=CARTESIAN_POINT('Ctrl Pts',(-5.89991477369114,3.22728061227828,2.60884193682636));
#48481=CARTESIAN_POINT('Ctrl Pts',(-5.96620595092363,3.68689046262614,1.38798465072928));
#48482=CARTESIAN_POINT('Ctrl Pts',(-6.03249712815611,4.14650031297395,0.167127364632348));
#48483=CARTESIAN_POINT('Ctrl Pts',(-6.09878830538858,3.93943223371586,-1.30471072568299));
#48484=CARTESIAN_POINT('Ctrl Pts',(-6.16507948262105,3.16081351299333,-2.35136569046795));
#48485=CARTESIAN_POINT('Ctrl Pts',(-6.23137065985354,2.38219479227071,-3.39802065525303));
#48486=CARTESIAN_POINT('Ctrl Pts',(-6.29766183708603,1.03202543008335,-4.0194924945073));
#48487=CARTESIAN_POINT('Ctrl Pts',(-6.36395301431851,-0.269425382418601,
-3.93027640726029));
#48488=CARTESIAN_POINT('Ctrl Pts',(-6.43024419155099,-1.57087619492055,
-3.84106032001328));
#48489=CARTESIAN_POINT('Ctrl Pts',(-6.49653536878348,-2.82360845773726,
-3.041156306265));
#48490=CARTESIAN_POINT('Ctrl Pts',(-6.56282654601597,-3.4521156832451,-1.89804109113744));
#48491=CARTESIAN_POINT('Ctrl Pts',(-6.59616318999905,-3.76818069358685,
-1.32318895320192));
#48492=CARTESIAN_POINT('Ctrl Pts',(-6.62949983398215,-3.92638520355753,
-0.661542007713824));
#48493=CARTESIAN_POINT('Ctrl Pts',(-6.66283647796524,-3.92647903110527,
6.27886499063313E-5));
#48494=CARTESIAN_POINT('Ctrl Pts',(-6.84616352203489,-3.92649740926382,
-0.000290818540083879));
#48495=CARTESIAN_POINT('Ctrl Pts',(-6.81390371882873,-3.92691806150654,
-0.640516977914417));
#48496=CARTESIAN_POINT('Ctrl Pts',(-6.78164391562257,-3.77926271887843,
-1.28056027072101));
#48497=CARTESIAN_POINT('Ctrl Pts',(-6.74938411241641,-3.48248030899597,
-1.84173656412097));
#48498=CARTESIAN_POINT('Ctrl Pts',(-6.68309293518393,-2.87261746490879,
-2.99490655981828));
#48499=CARTESIAN_POINT('Ctrl Pts',(-6.61680175795143,-1.63303893331471,
-3.81504655856512));
#48500=CARTESIAN_POINT('Ctrl Pts',(-6.55051058071895,-0.333208364222228,
-3.92538340295274));
#48501=CARTESIAN_POINT('Ctrl Pts',(-6.48421940348646,0.966622204870406,
-4.03572024734038));
#48502=CARTESIAN_POINT('Ctrl Pts',(-6.41792822625399,2.32670481146146,-3.43625393736864));
#48503=CARTESIAN_POINT('Ctrl Pts',(-6.3516370490215,3.12221610976888,-2.40237991127052));
#48504=CARTESIAN_POINT('Ctrl Pts',(-6.28534587178902,3.9177274080762,-1.36850588517251));
#48505=CARTESIAN_POINT('Ctrl Pts',(-6.21905469455653,4.14866739810001,0.0997758570517888));
#48506=CARTESIAN_POINT('Ctrl Pts',(-6.15276351732404,3.70894201133942,1.32793517562964));
#48507=CARTESIAN_POINT('Ctrl Pts',(-6.08647234009155,3.26921662457878,2.55609449420764));
#48508=CARTESIAN_POINT('Ctrl Pts',(-6.02018116285907,2.15882586103359,3.54413138913913));
#48509=CARTESIAN_POINT('Ctrl Pts',(-5.95388998562658,0.887884377429989,
3.83814069654488));
#48510=CARTESIAN_POINT('Ctrl Pts',(-5.8875988083941,-0.38305710617347,4.1321500039506));
#48511=CARTESIAN_POINT('Ctrl Pts',(-5.82130763116161,-1.81454930983531,
3.73213172383073));
#48512=CARTESIAN_POINT('Ctrl Pts',(-5.75501645392913,-2.74896324554502,
2.82185466473268));
#48513=CARTESIAN_POINT('Ctrl Pts',(-5.70206547663104,-3.49533905545499,
2.09475851252179));
#48514=CARTESIAN_POINT('Ctrl Pts',(-5.64911449933297,-3.92456737898498,
1.04210540159905));
#48515=CARTESIAN_POINT('Ctrl Pts',(-5.59616352203489,-3.93425725830108,
-0.00352254436509695));
#48516=CARTESIAN_POINT('Origin',(-54.75,0.,0.));
#48517=CARTESIAN_POINT('',(-4.16283647796528,-3.938710497775,0.00160298884803723));
#48518=CARTESIAN_POINT('',(-4.34616352203491,-3.93832454869238,0.00194456996648914));
#48519=CARTESIAN_POINT('',(-54.75,-3.933,-4.81653586104654E-16));
#48520=CARTESIAN_POINT('Ctrl Pts',(-4.16283647796528,-3.938710497775,0.00160298884803723));
#48521=CARTESIAN_POINT('Ctrl Pts',(-4.1673390405257,-3.93916707483314,0.0902537325677592));
#48522=CARTESIAN_POINT('Ctrl Pts',(-4.17184160308612,-3.93643450601992,
0.178875823251529));
#48523=CARTESIAN_POINT('Ctrl Pts',(-4.17634416564655,-3.93042322572512,
0.267274956415375));
#48524=CARTESIAN_POINT('Ctrl Pts',(-4.24263534287903,-3.84191921449391,
1.56877438593398));
#48525=CARTESIAN_POINT('Ctrl Pts',(-4.30892652011151,-3.04270074100715,
2.82194411801858));
#48526=CARTESIAN_POINT('Ctrl Pts',(-4.37521769734399,-1.89992957625108,
3.45107668626067));
#48527=CARTESIAN_POINT('Ctrl Pts',(-4.44150887457647,-0.757158411495012,
4.08020925450276));
#48528=CARTESIAN_POINT('Ctrl Pts',(-4.50780005180894,0.729165444530365,
4.08530465890234));
#48529=CARTESIAN_POINT('Ctrl Pts',(-4.57409122904142,1.87622327785216,3.46402206806303));
#48530=CARTESIAN_POINT('Ctrl Pts',(-4.64038240627392,3.02328111117421,2.84273947722358));
#48531=CARTESIAN_POINT('Ctrl Pts',(-4.70667358350641,3.83107292179253,1.59507889114495));
#48532=CARTESIAN_POINT('Ctrl Pts',(-4.77296476073891,3.92849832715561,0.294216862580042));
#48533=CARTESIAN_POINT('Ctrl Pts',(-4.83925593797138,4.02592373251865,-1.00664516598442));
#48534=CARTESIAN_POINT('Ctrl Pts',(-4.90554711520386,3.412982732627,-2.36070863703513));
#48535=CARTESIAN_POINT('Ctrl Pts',(-4.97183829243634,2.37126104968588,-3.14591540110713));
#48536=CARTESIAN_POINT('Ctrl Pts',(-5.03812946966882,1.32953936674452,-3.93112216517931));
#48537=CARTESIAN_POINT('Ctrl Pts',(-5.10442064690131,-0.140962999246524,
-4.14747222227252));
#48538=CARTESIAN_POINT('Ctrl Pts',(-5.1707118241338,-1.36469575040221,-3.6955741344339));
#48539=CARTESIAN_POINT('Ctrl Pts',(-5.23700300136628,-2.58842850155775,
-3.24367604659533));
#48540=CARTESIAN_POINT('Ctrl Pts',(-5.30329417859877,-3.56539163787799,
-2.12352981382508));
#48541=CARTESIAN_POINT('Ctrl Pts',(-5.36958535583125,-3.84676729222827,
-0.84973176523474));
#48542=CARTESIAN_POINT('Ctrl Pts',(-5.38400239654259,-3.90796102016165,
-0.572705483741063));
#48543=CARTESIAN_POINT('Ctrl Pts',(-5.39841943725393,-3.93625500214701,
-0.288411811967996));
#48544=CARTESIAN_POINT('Ctrl Pts',(-5.41283647796527,-3.93360662039214,
-0.00359624771770317));
#48545=CARTESIAN_POINT('Ctrl Pts',(-5.59616352203489,-3.93425725830108,
-0.00352254436509695));
#48546=CARTESIAN_POINT('Ctrl Pts',(-5.5828233221005,-3.93669847721738,-0.266952731453627));
#48547=CARTESIAN_POINT('Ctrl Pts',(-5.5694831221661,-3.91251108716881,-0.529937022884259));
#48548=CARTESIAN_POINT('Ctrl Pts',(-5.5561429222317,-3.8600577941153,-0.787157227085798));
#48549=CARTESIAN_POINT('Ctrl Pts',(-5.48985174499922,-3.59940273921825,
-2.06535622173015));
#48550=CARTESIAN_POINT('Ctrl Pts',(-5.42356056776673,-2.64075696166643,
-3.20121837294244));
#48551=CARTESIAN_POINT('Ctrl Pts',(-5.35726939053424,-1.42452331575331,
-3.67292744238449));
#48552=CARTESIAN_POINT('Ctrl Pts',(-5.29097821330175,-0.208289669840187,
-4.14463651182654));
#48553=CARTESIAN_POINT('Ctrl Pts',(-5.22468703606926,1.26553184443423,-3.95219249949835));
#48554=CARTESIAN_POINT('Ctrl Pts',(-5.15839585883677,2.31986611015527,-3.18400438214645));
#48555=CARTESIAN_POINT('Ctrl Pts',(-5.09210468160428,3.3742003758762,-2.41581626479464));
#48556=CARTESIAN_POINT('Ctrl Pts',(-5.02581350437181,4.0090473930439,-1.07188404241932));
#48557=CARTESIAN_POINT('Ctrl Pts',(-4.95952232713933,3.93275779055114,0.230388442126491));
#48558=CARTESIAN_POINT('Ctrl Pts',(-4.89323114990684,3.85646818805839,1.5326609266723));
#48559=CARTESIAN_POINT('Ctrl Pts',(-4.82693997267436,3.06904196590517,2.79327367338859));
#48560=CARTESIAN_POINT('Ctrl Pts',(-4.76064879544188,1.93222353831344,3.43309989255341));
#48561=CARTESIAN_POINT('Ctrl Pts',(-4.69435761820939,0.795405110721587,
4.0729261117183));
#48562=CARTESIAN_POINT('Ctrl Pts',(-4.6280664409769,-0.690805522308857,
4.09196580333158));
#48563=CARTESIAN_POINT('Ctrl Pts',(-4.56177526374441,-1.84364166896585,
3.48147211293344));
#48564=CARTESIAN_POINT('Ctrl Pts',(-4.49548408651194,-2.99647781562258,
2.87097842253544));
#48565=CARTESIAN_POINT('Ctrl Pts',(-4.42919290927946,-3.81593947590601,
1.6309513501263));
#48566=CARTESIAN_POINT('Ctrl Pts',(-4.36290173204699,-3.9255651240589,0.331060606933602));
#48567=CARTESIAN_POINT('Ctrl Pts',(-4.35732232870963,-3.9347917773286,0.221655176926881));
#48568=CARTESIAN_POINT('Ctrl Pts',(-4.35174292537227,-3.9389901201714,0.111825686834663));
#48569=CARTESIAN_POINT('Ctrl Pts',(-4.34616352203491,-3.93832454869238,
0.00194456996648914));
#48570=CARTESIAN_POINT('Origin',(-54.75,0.,0.));
#48571=CARTESIAN_POINT('',(-2.91283647796527,-3.92869173988258,0.0028084021417174));
#48572=CARTESIAN_POINT('',(-3.09616352203495,-3.9282466370004,0.0025678202255927));
#48573=CARTESIAN_POINT('',(-54.75,-3.933,-4.81653586104654E-16));
#48574=CARTESIAN_POINT('Ctrl Pts',(-2.91283647796527,-3.92869173988258,
0.0028084021417174));
#48575=CARTESIAN_POINT('Ctrl Pts',(-2.93625864379745,-3.93173980158221,
0.466994022202747));
#48576=CARTESIAN_POINT('Ctrl Pts',(-2.95968080962962,-3.85574928228062,
0.930213895198008));
#48577=CARTESIAN_POINT('Ctrl Pts',(-2.9831029754618,-3.69632003395113,1.36267350892606));
#48578=CARTESIAN_POINT('Ctrl Pts',(-3.04939415269429,-3.24509137163283,
2.5866532683107));
#48579=CARTESIAN_POINT('Ctrl Pts',(-3.11568532992677,-2.12548025594738,
3.56422925579285));
#48580=CARTESIAN_POINT('Ctrl Pts',(-3.18197650715925,-0.851836446862079,
3.8463018352547));
#48581=CARTESIAN_POINT('Ctrl Pts',(-3.24826768439174,0.421807362223362,
4.12837441471658));
#48582=CARTESIAN_POINT('Ctrl Pts',(-3.31455886162423,1.84948386470868,3.714943586158));
#48583=CARTESIAN_POINT('Ctrl Pts',(-3.38085003885672,2.77531661985273,2.79594001521562));
#48584=CARTESIAN_POINT('Ctrl Pts',(-3.4471412160892,3.70114937499666,1.87693644427334));
#48585=CARTESIAN_POINT('Ctrl Pts',(-3.51343239332168,4.12513838279943,0.452360130947363));
#48586=CARTESIAN_POINT('Ctrl Pts',(-3.57972357055417,3.85250286423086,-0.823337166685192));
#48587=CARTESIAN_POINT('Ctrl Pts',(-3.64601474778666,3.57986734566225,-2.09903446431789));
#48588=CARTESIAN_POINT('Ctrl Pts',(-3.71230592501914,2.61060730072214,-3.22585274625714));
#48589=CARTESIAN_POINT('Ctrl Pts',(-3.77859710225163,1.39000167980377,-3.68613050369547));
#48590=CARTESIAN_POINT('Ctrl Pts',(-3.84488827948411,0.169396058885551,
-4.14640826113375));
#48591=CARTESIAN_POINT('Ctrl Pts',(-3.9111794567166,-1.30255513801086,-3.94014549407127));
#48592=CARTESIAN_POINT('Ctrl Pts',(-3.97747063394908,-2.3496359619713,-3.16209954706376));
#48593=CARTESIAN_POINT('Ctrl Pts',(-4.03925924862115,-3.32559801700176,
-2.43689925309078));
#48594=CARTESIAN_POINT('Ctrl Pts',(-4.10104786329321,-3.93244489601268,
-1.21495015629594));
#48595=CARTESIAN_POINT('Ctrl Pts',(-4.16283647796528,-3.938710497775,0.00160298884803723));
#48596=CARTESIAN_POINT('Ctrl Pts',(-4.34616352203491,-3.93832454869238,
0.00194456996648914));
#48597=CARTESIAN_POINT('Ctrl Pts',(-4.28545174813977,-3.93108219270887,
-1.19371688687386));
#48598=CARTESIAN_POINT('Ctrl Pts',(-4.22473997424464,-3.34792768095492,
-2.39549121615994));
#48599=CARTESIAN_POINT('Ctrl Pts',(-4.1640282003495,-2.4006712852553,-3.12353006333101));
#48600=CARTESIAN_POINT('Ctrl Pts',(-4.09773702311702,-1.36636216227721,
-3.91847557642554));
#48601=CARTESIAN_POINT('Ctrl Pts',(-4.03144584588453,0.102045719700945,
-4.1486121886383));
#48602=CARTESIAN_POINT('Ctrl Pts',(-3.96515466865205,1.32996426409882,-3.70821490010836));
#48603=CARTESIAN_POINT('Ctrl Pts',(-3.89886349141955,2.55788280849698,-3.26781761157831));
#48604=CARTESIAN_POINT('Ctrl Pts',(-3.83257231418708,3.54531201531465,-2.15688642230563));
#48605=CARTESIAN_POINT('Ctrl Pts',(-3.76628113695459,3.83862590846361,-0.885784268610713));
#48606=CARTESIAN_POINT('Ctrl Pts',(-3.69998995972212,4.13193980161248,0.385317885083766));
#48607=CARTESIAN_POINT('Ctrl Pts',(-3.63369878248965,3.73113838109276,1.8165910032001));
#48608=CARTESIAN_POINT('Ctrl Pts',(-3.56740760525718,2.82035020216559,2.75050675993973));
#48609=CARTESIAN_POINT('Ctrl Pts',(-3.5011164280247,1.90956202323822,3.68442251667957));
#48610=CARTESIAN_POINT('Ctrl Pts',(-3.4348252507922,0.488787085902983,4.12098091204254));
#48611=CARTESIAN_POINT('Ctrl Pts',(-3.36853407355971,-0.789269090623166,
3.85962654446236));
#48612=CARTESIAN_POINT('Ctrl Pts',(-3.30224289632722,-2.06732526714932,
3.59827217688217));
#48613=CARTESIAN_POINT('Ctrl Pts',(-3.23595171909473,-3.20266268286653,
2.63900504635881));
#48614=CARTESIAN_POINT('Ctrl Pts',(-3.16966054186224,-3.67370626610708,
1.42251350760468));
#48615=CARTESIAN_POINT('Ctrl Pts',(-3.14516153525315,-3.84778825319431,
0.972938835799878));
#48616=CARTESIAN_POINT('Ctrl Pts',(-3.12066252864405,-3.93114132743054,
0.488232585502865));
#48617=CARTESIAN_POINT('Ctrl Pts',(-3.09616352203495,-3.9282466370004,0.0025678202255927));
#48618=CARTESIAN_POINT('Origin',(-54.75,0.,0.));
#48619=CARTESIAN_POINT('',(-1.66283647796526,-3.92848774701504,-0.00268787972552448));
#48620=CARTESIAN_POINT('',(-1.84616352203493,-3.92893748603655,-0.00291966682171161));
#48621=CARTESIAN_POINT('',(-54.75,-3.933,-4.81653586104654E-16));
#48622=CARTESIAN_POINT('Ctrl Pts',(-1.66283647796526,-3.92848774701504,
-0.00268787972552448));
#48623=CARTESIAN_POINT('Ctrl Pts',(-1.7051782470692,-3.923213871108,0.836568195474228));
#48624=CARTESIAN_POINT('Ctrl Pts',(-1.74752001617314,-3.65997084863724,
1.67883665840762));
#48625=CARTESIAN_POINT('Ctrl Pts',(-1.78986178527708,-3.16337477926387,
2.34790251287165));
#48626=CARTESIAN_POINT('Ctrl Pts',(-1.85615296250957,-2.38589337627915,
3.39540629169586));
#48627=CARTESIAN_POINT('Ctrl Pts',(-1.92244413974206,-1.03642394411599,
4.01836100213633));
#48628=CARTESIAN_POINT('Ctrl Pts',(-1.98873531697455,0.265119230997025,
3.9305704655395));
#48629=CARTESIAN_POINT('Ctrl Pts',(-2.05502649420703,1.56666240610989,3.84277992894269));
#48630=CARTESIAN_POINT('Ctrl Pts',(-2.12131767143951,2.82027932417245,3.04424414530877));
#48631=CARTESIAN_POINT('Ctrl Pts',(-2.187608848672,3.45003942039896,1.90181664633624));
#48632=CARTESIAN_POINT('Ctrl Pts',(-2.25390002590448,4.07979951662547,0.759389147363717));
#48633=CARTESIAN_POINT('Ctrl Pts',(-2.32019120313698,4.08570279101577,-0.726930066947709));
#48634=CARTESIAN_POINT('Ctrl Pts',(-2.38648238036946,3.46504662903402,-1.87432726913705));
#48635=CARTESIAN_POINT('Ctrl Pts',(-2.45277355760195,2.84439046705227,-3.02172447132639));
#48636=CARTESIAN_POINT('Ctrl Pts',(-2.51906473483443,1.59717486869864,-3.83019966139392));
#48637=CARTESIAN_POINT('Ctrl Pts',(-2.58535591206691,0.296367005435699,
-3.92833700002301));
#48638=CARTESIAN_POINT('Ctrl Pts',(-2.65164708929939,-1.00444085782724,
-4.0264743386521));
#48639=CARTESIAN_POINT('Ctrl Pts',(-2.71793826653186,-2.35884098599932,
-3.41427382584272));
#48640=CARTESIAN_POINT('Ctrl Pts',(-2.78422944376434,-3.14461794560989,
-2.37298180379444));
#48641=CARTESIAN_POINT('Ctrl Pts',(-2.82709845516465,-3.6527622092351,-1.69960170363885));
#48642=CARTESIAN_POINT('Ctrl Pts',(-2.86996746656496,-3.92311294786624,
-0.84677906901001));
#48643=CARTESIAN_POINT('Ctrl Pts',(-2.91283647796527,-3.92869173988258,
0.0028084021417174));
#48644=CARTESIAN_POINT('Ctrl Pts',(-3.09616352203495,-3.9282466370004,0.0025678202255927));
#48645=CARTESIAN_POINT('Ctrl Pts',(-3.05437135141156,-3.92330866550267,
-0.825914128454525));
#48646=CARTESIAN_POINT('Ctrl Pts',(-3.01257918078818,-3.66738974622449,
-1.65718535520051));
#48647=CARTESIAN_POINT('Ctrl Pts',(-2.97078701016479,-3.18273468739347,
-2.32160780899296));
#48648=CARTESIAN_POINT('Ctrl Pts',(-2.9044958329323,-2.41396977467525,-3.37552163985192));
#48649=CARTESIAN_POINT('Ctrl Pts',(-2.83820465569982,-1.06969019847474,
-4.00963335458485));
#48650=CARTESIAN_POINT('Ctrl Pts',(-2.77191347846733,0.232540257688125,
-3.93263120170715));
#48651=CARTESIAN_POINT('Ctrl Pts',(-2.70562230123485,1.53477071385084,-3.85562904882945));
#48652=CARTESIAN_POINT('Ctrl Pts',(-2.63933112400237,2.79495204997593,-3.0675130283413));
#48653=CARTESIAN_POINT('Ctrl Pts',(-2.57303994676988,3.43415635782225,-1.93034478664988));
#48654=CARTESIAN_POINT('Ctrl Pts',(-2.50674876953739,4.07336066566865,-0.793176544958324));
#48655=CARTESIAN_POINT('Ctrl Pts',(-2.4404575923049,4.09158794523613,0.693043917936572));
#48656=CARTESIAN_POINT('Ctrl Pts',(-2.37416641507241,3.480463260221,1.84554603281607));
#48657=CARTESIAN_POINT('Ctrl Pts',(-2.30787523783993,2.86933857520593,2.99804814769544));
#48658=CARTESIAN_POINT('Ctrl Pts',(-2.24158406060745,1.6288619256084,3.81683191455948));
#48659=CARTESIAN_POINT('Ctrl Pts',(-2.17529288337497,0.328912022552463,
3.92574602707322));
#48660=CARTESIAN_POINT('Ctrl Pts',(-2.10900170614248,-0.971037880503623,
4.03466013958697));
#48661=CARTESIAN_POINT('Ctrl Pts',(-2.04271052890999,-2.33046103701813,
3.43370459775025));
#48662=CARTESIAN_POINT('Ctrl Pts',(-1.9764193516775,-3.12484170726232,2.39896126641609));
#48663=CARTESIAN_POINT('Ctrl Pts',(-1.93300074179664,-3.64513574725602,
1.72123733835161));
#48664=CARTESIAN_POINT('Ctrl Pts',(-1.88958213191578,-3.92303600768351,
0.85742570116635));
#48665=CARTESIAN_POINT('Ctrl Pts',(-1.84616352203493,-3.92893748603655,
-0.00291966682171161));
#48666=CARTESIAN_POINT('Origin',(-54.75,0.,0.));
#48667=CARTESIAN_POINT('',(-0.412836477965312,-3.93946807025562,-0.00149173430430305));
#48668=CARTESIAN_POINT('',(-0.596163522034903,-3.93901438905508,-0.00135576060872734));
#48669=CARTESIAN_POINT('',(-54.75,-3.933,-4.81653586104654E-16));
#48670=CARTESIAN_POINT('Ctrl Pts',(-0.412836477965312,-3.93946807025562,
-0.00149173430430305));
#48671=CARTESIAN_POINT('Ctrl Pts',(-0.474097850340994,-3.9331312283141,
1.20496832338296));
#48672=CARTESIAN_POINT('Ctrl Pts',(-0.535359222716679,-3.33651390232707,
2.41661565923732));
#48673=CARTESIAN_POINT('Ctrl Pts',(-0.596620595092361,-2.37426143690827,
3.14318560345314));
#48674=CARTESIAN_POINT('Ctrl Pts',(-0.662911772324848,-1.33300417717378,
3.92940985988084));
#48675=CARTESIAN_POINT('Ctrl Pts',(-0.72920294955734,0.136393222589551,
4.1476331777127));
#48676=CARTESIAN_POINT('Ctrl Pts',(-0.795494126789824,1.36041507745367,
3.69713690330391));
#48677=CARTESIAN_POINT('Ctrl Pts',(-0.861785304022308,2.58443693231779,
3.24664062889511));
#48678=CARTESIAN_POINT('Ctrl Pts',(-0.928076481254795,3.56308324228286,
2.12742476224559));
#48679=CARTESIAN_POINT('Ctrl Pts',(-0.994367658487279,3.84596040873201,
0.853902561958117));
#48680=CARTESIAN_POINT('Ctrl Pts',(-1.06065883571976,4.12883757518116,-0.419619638329351));
#48681=CARTESIAN_POINT('Ctrl Pts',(-1.12695001295223,3.71594559811471,-1.84744817225453));
#48682=CARTESIAN_POINT('Ctrl Pts',(-1.19324119018472,2.79739171077215,-2.77376620717791));
#48683=CARTESIAN_POINT('Ctrl Pts',(-1.2595323674172,1.8788378234297,-3.7000842421012));
#48684=CARTESIAN_POINT('Ctrl Pts',(-1.32582354464969,0.454622025811202,
-4.12489177802249));
#48685=CARTESIAN_POINT('Ctrl Pts',(-1.39211472188217,-0.821194066006917,
-3.85296348705388));
#48686=CARTESIAN_POINT('Ctrl Pts',(-1.45840589911466,-2.09701015782518,
-3.58103519608524));
#48687=CARTESIAN_POINT('Ctrl Pts',(-1.52469707634715,-3.22442654384318,
-2.61237107822653));
#48688=CARTESIAN_POINT('Ctrl Pts',(-1.59098825357964,-3.68538804994898,
-1.39201259569326));
#48689=CARTESIAN_POINT('Ctrl Pts',(-1.61493766170818,-3.85192235665705,
-0.951126423785145));
#48690=CARTESIAN_POINT('Ctrl Pts',(-1.63888706983672,-3.93147076376634,
-0.477389024592041));
#48691=CARTESIAN_POINT('Ctrl Pts',(-1.66283647796526,-3.92848774701504,
-0.00268787972552448));
#48692=CARTESIAN_POINT('Ctrl Pts',(-1.84616352203493,-3.92893748603655,
-0.00291966682171161));
#48693=CARTESIAN_POINT('Ctrl Pts',(-1.82329095468331,-3.9320463363999,-0.456142545881115));
#48694=CARTESIAN_POINT('Ctrl Pts',(-1.80041838733169,-3.85967291538721,
-0.908403501985509));
#48695=CARTESIAN_POINT('Ctrl Pts',(-1.77754581998007,-3.70748927430689,
-1.33199168146346));
#48696=CARTESIAN_POINT('Ctrl Pts',(-1.71125464274758,-3.26641798713338,
-2.55967017717775));
#48697=CARTESIAN_POINT('Ctrl Pts',(-1.64496346551509,-2.15493722881242,
-3.54649604777468));
#48698=CARTESIAN_POINT('Ctrl Pts',(-1.5786722882826,-0.883678993796144,
-3.83911237490377));
#48699=CARTESIAN_POINT('Ctrl Pts',(-1.51238111105012,0.387579241219839,
-4.13172870203281));
#48700=CARTESIAN_POINT('Ctrl Pts',(-1.44608993381766,1.8186149529309,-3.7301354856943));
#48701=CARTESIAN_POINT('Ctrl Pts',(-1.37979875658518,2.75204019720566,-2.81884035677723));
#48702=CARTESIAN_POINT('Ctrl Pts',(-1.31350757935269,3.68546544148063,-1.90754522785995));
#48703=CARTESIAN_POINT('Ctrl Pts',(-1.24721640212018,4.12128021831895,-0.486548186363495));
#48704=CARTESIAN_POINT('Ctrl Pts',(-1.18092522488769,3.85921161225801,0.791372148289516));
#48705=CARTESIAN_POINT('Ctrl Pts',(-1.1146340476552,3.59714300619707,2.06929248294253));
#48706=CARTESIAN_POINT('Ctrl Pts',(-1.04834287042271,2.63719101723718,3.20413611075232));
#48707=CARTESIAN_POINT('Ctrl Pts',(-0.982051693190223,1.42047028231716,
3.67450017059044));
#48708=CARTESIAN_POINT('Ctrl Pts',(-0.915760515957748,0.20374954739741,
4.14486423042845));
#48709=CARTESIAN_POINT('Ctrl Pts',(-0.849469338725274,-1.26973993348217,
3.95074872229507));
#48710=CARTESIAN_POINT('Ctrl Pts',(-0.783178161492798,-2.32328652660156,
3.1814334930799));
#48711=CARTESIAN_POINT('Ctrl Pts',(-0.720839948340164,-3.31400979974224,
2.45799277679574));
#48712=CARTESIAN_POINT('Ctrl Pts',(-0.658501735187536,-3.93337961985426,
1.22590574495181));
#48713=CARTESIAN_POINT('Ctrl Pts',(-0.596163522034903,-3.93901438905508,
-0.00135576060872734));
#48714=CARTESIAN_POINT('Origin',(-111.877773449273,0.,0.));
#48715=CARTESIAN_POINT('',(-0.00277344927343423,-3.22805001866674,-0.00122234597570187));
#48716=CARTESIAN_POINT('',(0.,-3.22275,5.46201577318104E-12));
#48717=CARTESIAN_POINT('',(-111.877773449273,-3.22275,5.46201577318104E-12));
#48718=CARTESIAN_POINT('',(0.,-3.22243683749934,-0.0449265047300178));
#48719=CARTESIAN_POINT('Ctrl Pts',(-0.00277344927343414,-3.22805001866674,
-0.00122234597570214));
#48720=CARTESIAN_POINT('Ctrl Pts',(-0.00184896618229052,-3.22812837747028,
-0.0161409391011512));
#48721=CARTESIAN_POINT('Ctrl Pts',(-0.000924483091146902,-3.22809658599603,
-0.0310585642458751));
#48722=CARTESIAN_POINT('Ctrl Pts',(-3.28431943100171E-15,-3.22795401163284,
-0.0459738408030352));
#48723=CARTESIAN_POINT('Origin',(0.,0.,0.));
#48724=CARTESIAN_POINT('Origin',(-111.877773449273,0.,0.));
#48725=CARTESIAN_POINT('',(-1.25277344927345,-3.21905260276956,-0.00220248267844716));
#48726=CARTESIAN_POINT('',(-1.00622655072714,-3.22767826654644,-0.0011109274034582));
#48727=CARTESIAN_POINT('',(-111.877773449273,-3.22275,5.46201577318104E-12));
#48728=CARTESIAN_POINT('Ctrl Pts',(-1.25277344927345,-3.21905260276956,
-0.00220248267844716));
#48729=CARTESIAN_POINT('Ctrl Pts',(-1.22882404114487,-3.22149692446714,
-0.391178611491322));
#48730=CARTESIAN_POINT('Ctrl Pts',(-1.20487463301629,-3.15631395243283,
-0.779365034896385));
#48731=CARTESIAN_POINT('Ctrl Pts',(-1.18092522488771,-3.01985363284375,
-1.14063274669891));
#48732=CARTESIAN_POINT('Ctrl Pts',(-1.11463404765522,-2.64213593800486,
-2.14060993957577));
#48733=CARTESIAN_POINT('Ctrl Pts',(-1.04834287042274,-1.71831667585426,
-2.93434558306168));
#48734=CARTESIAN_POINT('Ctrl Pts',(-0.982051693190246,-0.672896815720211,
-3.15716706786221));
#48735=CARTESIAN_POINT('Ctrl Pts',(-0.91576051595777,0.372523044413605,
-3.37998855266269));
#48736=CARTESIAN_POINT('Ctrl Pts',(-0.849469338725299,1.53954350253069,
-3.03189587877802));
#48737=CARTESIAN_POINT('Ctrl Pts',(-0.783178161492821,2.29221818863138,
-2.27285915183992));
#48738=CARTESIAN_POINT('Ctrl Pts',(-0.716886984260322,3.04489287473232,
-1.51382242490155));
#48739=CARTESIAN_POINT('Ctrl Pts',(-0.650595807027827,3.38322178881643,
-0.343841644909505));
#48740=CARTESIAN_POINT('Ctrl Pts',(-0.584304629795333,3.15142865681201,
0.69969857145897));
#48741=CARTESIAN_POINT('Ctrl Pts',(-0.518013452562862,2.91963552480766,
1.74323878782709));
#48742=CARTESIAN_POINT('Ctrl Pts',(-0.451722275330373,2.11772034671489,
2.66033844057194));
#48743=CARTESIAN_POINT('Ctrl Pts',(-0.385431098097901,1.11474134016462,
3.02948079204712));
#48744=CARTESIAN_POINT('Ctrl Pts',(-0.319139920865414,0.111762333614127,
3.39862314352239));
#48745=CARTESIAN_POINT('Ctrl Pts',(-0.252848743632928,-1.09228050139405,
3.21980819372804));
#48746=CARTESIAN_POINT('Ctrl Pts',(-0.186557566400438,-1.94549988451387,
2.57556608276912));
#48747=CARTESIAN_POINT('Ctrl Pts',(-0.125296194024769,-2.73398173880538,
1.98020547058501));
#48748=CARTESIAN_POINT('Ctrl Pts',(-0.0640348216491032,-3.22285753014165,
0.987366301598871));
#48749=CARTESIAN_POINT('Ctrl Pts',(-0.00277344927343423,-3.22805001866674,
-0.00122234597570187));
#48750=CARTESIAN_POINT('',(0.,-1.09131022003071,3.03235215074973));
#48751=CARTESIAN_POINT('Origin',(0.,0.,0.));
#48752=CARTESIAN_POINT('Ctrl Pts',(-1.00622655072714,-3.22767826654644,
-0.00111092740345839));
#48753=CARTESIAN_POINT('Ctrl Pts',(-1.00227358664718,-3.22797105053401,
-0.0648797357467673));
#48754=CARTESIAN_POINT('Ctrl Pts',(-0.932029445334739,-3.19723962854479,
-1.19776843518848));
#48755=CARTESIAN_POINT('Ctrl Pts',(-0.795494126789802,-1.86525717936383,
-3.32418745080932));
#48756=CARTESIAN_POINT('Ctrl Pts',(-0.596620595092344,1.78624879507146,
-3.36601485692819));
#48757=CARTESIAN_POINT('Ctrl Pts',(-0.397747063394925,3.80117096935424,
-0.317409156202402));
#48758=CARTESIAN_POINT('Ctrl Pts',(-0.198873531697423,2.31445171887122,
3.02736545452069));
#48759=CARTESIAN_POINT('Ctrl Pts',(-0.0662911772324812,-0.0808825703380203,
3.39599395944883));
#48760=CARTESIAN_POINT('Ctrl Pts',(0.,-1.09131022003071,3.03235215074973));
#48761=CARTESIAN_POINT('Origin',(-111.877773449273,0.,0.));
#48762=CARTESIAN_POINT('',(-2.50277344927344,-3.21921975710822,0.0023012402776184));
#48763=CARTESIAN_POINT('',(-2.25622655072717,-3.2194211246184,-0.00239241195666928));
#48764=CARTESIAN_POINT('',(-111.877773449273,-3.22275,5.46201577318104E-12));
#48765=CARTESIAN_POINT('Ctrl Pts',(-2.50277344927344,-3.21921975710822,
0.0023012402776184));
#48766=CARTESIAN_POINT('Ctrl Pts',(-2.45990443787309,-3.21464842429137,
-0.693861491137611));
#48767=CARTESIAN_POINT('Ctrl Pts',(-2.41703542647275,-2.99311960585182,
-1.39267515647013));
#48768=CARTESIAN_POINT('Ctrl Pts',(-2.37416641507242,-2.57673976206881,
-1.94445133693756));
#48769=CARTESIAN_POINT('Ctrl Pts',(-2.30787523783994,-1.93286417178559,
-2.79769920473741));
#48770=CARTESIAN_POINT('Ctrl Pts',(-2.24158406060747,-0.823051557225173,
-3.29934405667177));
#48771=CARTESIAN_POINT('Ctrl Pts',(-2.17529288337499,0.242846876878725,
-3.21892907877561));
#48772=CARTESIAN_POINT('Ctrl Pts',(-2.10900170614251,1.30874531098262,-3.13851410087944));
#48773=CARTESIAN_POINT('Ctrl Pts',(-2.04271052891002,2.33072956463,-2.47603929315276));
#48774=CARTESIAN_POINT('Ctrl Pts',(-1.97641935167754,2.8393030825623,-1.53584749723235));
#48775=CARTESIAN_POINT('Ctrl Pts',(-1.91012817444505,3.34787660049467,-0.595655701311836));
#48776=CARTESIAN_POINT('Ctrl Pts',(-1.84383699721256,3.34303938271184,0.622253082802464));
#48777=CARTESIAN_POINT('Ctrl Pts',(-1.77754581998007,2.82700598578506,1.55837264098061));
#48778=CARTESIAN_POINT('Ctrl Pts',(-1.71125464274759,2.31097258885834,2.49449219915864));
#48779=CARTESIAN_POINT('Ctrl Pts',(-1.64496346551511,1.28374301278778,3.14882253140059));
#48780=CARTESIAN_POINT('Ctrl Pts',(-1.57867228828262,0.217242054843513,
3.22075920870002));
#48781=CARTESIAN_POINT('Ctrl Pts',(-1.51238111105013,-0.849258903100873,
3.29269588599945));
#48782=CARTESIAN_POINT('Ctrl Pts',(-1.44608993381765,-1.95503124291897,
2.78223890835625));
#48783=CARTESIAN_POINT('Ctrl Pts',(-1.37979875658516,-2.59210934906441,
1.92390104840077));
#48784=CARTESIAN_POINT('Ctrl Pts',(-1.33745698748126,-2.99902645625288,
1.3756600154815));
#48785=CARTESIAN_POINT('Ctrl Pts',(-1.29511521837735,-3.21473112207246,
0.685494572075572));
#48786=CARTESIAN_POINT('Ctrl Pts',(-1.25277344927345,-3.21905260276956,
-0.00220248267844716));
#48787=CARTESIAN_POINT('Ctrl Pts',(-2.25622655072717,-3.2194211246184,-0.00239241195666928));
#48788=CARTESIAN_POINT('Ctrl Pts',(-2.23335398337544,-3.22196855597136,
-0.373768977808676));
#48789=CARTESIAN_POINT('Ctrl Pts',(-2.2104814160237,-3.1626648583949,-0.744357331811508));
#48790=CARTESIAN_POINT('Ctrl Pts',(-2.18760884867197,-3.03796365593016,
-1.09145084958913));
#48791=CARTESIAN_POINT('Ctrl Pts',(-2.12131767143949,-2.67654425833608,
-2.09742615395299));
#48792=CARTESIAN_POINT('Ctrl Pts',(-2.055026494207,-1.76578285129882,-2.90604376759822));
#48793=CARTESIAN_POINT('Ctrl Pts',(-1.98873531697452,-0.724097756740481,
-3.14581729118237));
#48794=CARTESIAN_POINT('Ctrl Pts',(-1.92244413974204,0.317587337817736,
-3.38559081476649));
#48795=CARTESIAN_POINT('Ctrl Pts',(-1.85615296250958,1.49019611989687,-3.05652024828963));
#48796=CARTESIAN_POINT('Ctrl Pts',(-1.78986178527711,2.25505658417029,-2.30979348075427));
#48797=CARTESIAN_POINT('Ctrl Pts',(-1.72357060804462,3.0199170484438,-1.56306671321882));
#48798=CARTESIAN_POINT('Ctrl Pts',(-1.65727943081212,3.37702919491142,-0.398683744624477));
#48799=CARTESIAN_POINT('Ctrl Pts',(-1.59098825357964,3.16228686076928,0.648460358732475));
#48800=CARTESIAN_POINT('Ctrl Pts',(-1.52469707634714,2.94754452662709,1.69560446208966));
#48801=CARTESIAN_POINT('Ctrl Pts',(-1.45840589911467,2.16094771187536,2.62550970020934));
#48802=CARTESIAN_POINT('Ctrl Pts',(-1.39211472188217,1.16395133545451,3.01093196663321));
#48803=CARTESIAN_POINT('Ctrl Pts',(-1.32582354464969,0.166954959034,3.39635423305696));
#48804=CARTESIAN_POINT('Ctrl Pts',(-1.2595323674172,-1.04044097905563,3.23729352778482));
#48805=CARTESIAN_POINT('Ctrl Pts',(-1.19324119018472,-1.90373039755963,
2.6069068878275));
#48806=CARTESIAN_POINT('Ctrl Pts',(-1.13090297703219,-2.71554159219717,
2.01411040463404));
#48807=CARTESIAN_POINT('Ctrl Pts',(-1.06856476387967,-3.22306106531334,
1.0045226899468));
#48808=CARTESIAN_POINT('Ctrl Pts',(-1.00622655072714,-3.22767826654644,
-0.0011109274034582));
#48809=CARTESIAN_POINT('Origin',(-111.877773449273,0.,0.));
#48810=CARTESIAN_POINT('',(-3.75277344927344,-3.22742925418368,0.00131350936171883));
#48811=CARTESIAN_POINT('',(-3.50622655072716,-3.21885503417064,0.00210410441258302));
#48812=CARTESIAN_POINT('',(-111.877773449273,-3.22275,5.46201577318104E-12));
#48813=CARTESIAN_POINT('Ctrl Pts',(-3.75277344927344,-3.22742925418368,
0.00131350936171883));
#48814=CARTESIAN_POINT('Ctrl Pts',(-3.69098483460135,-3.2222951407648,-0.995545541875145));
#48815=CARTESIAN_POINT('Ctrl Pts',(-3.62919621992925,-2.72503712415365,
-1.99682610421916));
#48816=CARTESIAN_POINT('Ctrl Pts',(-3.56740760525716,-1.92532145854212,
-2.59106440765253));
#48817=CARTESIAN_POINT('Ctrl Pts',(-3.50111642802467,-1.06733017315741,
-3.22860510831862));
#48818=CARTESIAN_POINT('Ctrl Pts',(-3.43482525079217,0.138805275558225,
-3.39761943136768));
#48819=CARTESIAN_POINT('Ctrl Pts',(-3.36853407355969,1.13898497675701,-3.02046200884451));
#48820=CARTESIAN_POINT('Ctrl Pts',(-3.3022428963272,2.1391646779558,-2.64330458632134));
#48821=CARTESIAN_POINT('Ctrl Pts',(-3.23595171909473,2.93338863163767,-1.7199754182263));
#48822=CARTESIAN_POINT('Ctrl Pts',(-3.16966054186224,3.15678962768858,-0.674652899552124));
#48823=CARTESIAN_POINT('Ctrl Pts',(-3.10336936462976,3.38019062373947,0.370669619121929));
#48824=CARTESIAN_POINT('Ctrl Pts',(-3.03707818739727,3.03276866215923,1.53798548837486));
#48825=CARTESIAN_POINT('Ctrl Pts',(-2.97078701016479,2.27412957961686,2.29102865091111));
#48826=CARTESIAN_POINT('Ctrl Pts',(-2.90449583293231,1.51549049707441,3.04407181344744));
#48827=CARTESIAN_POINT('Ctrl Pts',(-2.83820465569982,0.34563429356962,3.38284226926708));
#48828=CARTESIAN_POINT('Ctrl Pts',(-2.77191347846733,-0.698005570587585,
3.15170842602795));
#48829=CARTESIAN_POINT('Ctrl Pts',(-2.70562230123485,-1.74164543474467,
2.92057458278884));
#48830=CARTESIAN_POINT('Ctrl Pts',(-2.63933112400237,-2.65906895955433,
2.11953644049109));
#48831=CARTESIAN_POINT('Ctrl Pts',(-2.57303994676988,-3.02881143895618,
1.11659192750956));
#48832=CARTESIAN_POINT('Ctrl Pts',(-2.54961778093773,-3.15944978374479,
0.762229044178745));
#48833=CARTESIAN_POINT('Ctrl Pts',(-2.52619561510558,-3.22171737745944,
0.38266081491523));
#48834=CARTESIAN_POINT('Ctrl Pts',(-2.50277344927344,-3.21921975710822,
0.0023012402776184));
#48835=CARTESIAN_POINT('Ctrl Pts',(-3.50622655072716,-3.21885503417064,
0.00210410441258302));
#48836=CARTESIAN_POINT('Ctrl Pts',(-3.46443438010368,-3.21480879780153,
-0.67676449465048));
#48837=CARTESIAN_POINT('Ctrl Pts',(-3.4226422094802,-3.00510559487675,-1.35791866347924));
#48838=CARTESIAN_POINT('Ctrl Pts',(-3.38085003885672,-2.60797310292387,
-1.90235483509507));
#48839=CARTESIAN_POINT('Ctrl Pts',(-3.31455886162423,-1.97803739927232,
-2.76594517285287));
#48840=CARTESIAN_POINT('Ctrl Pts',(-3.24826768439174,-0.876517693144756,
-3.28554434108499));
#48841=CARTESIAN_POINT('Ctrl Pts',(-3.18197650715925,0.190546431594337,
-3.22244780200914));
#48842=CARTESIAN_POINT('Ctrl Pts',(-3.11568532992677,1.25761055633331,-3.1593512629333));
#48843=CARTESIAN_POINT('Ctrl Pts',(-3.04939415269428,2.29021909968395,-2.5135590165496));
#48844=CARTESIAN_POINT('Ctrl Pts',(-2.9831029754618,2.81399120319597,-1.5817489603812));
#48845=CARTESIAN_POINT('Ctrl Pts',(-2.91681179822931,3.33776330670811,-0.6499389042126));
#48846=CARTESIAN_POINT('Ctrl Pts',(-2.85052062099683,3.35269897038154,0.567888961740592));
#48847=CARTESIAN_POINT('Ctrl Pts',(-2.78422944376434,2.85193566536462,1.5122637877586));
#48848=CARTESIAN_POINT('Ctrl Pts',(-2.71793826653186,2.35117236034781,2.45663861377639));
#48849=CARTESIAN_POINT('Ctrl Pts',(-2.65164708929937,1.33471008664077,3.12756039985888));
#48850=CARTESIAN_POINT('Ctrl Pts',(-2.58535591206689,0.269514675994107,
3.21680600273325));
#48851=CARTESIAN_POINT('Ctrl Pts',(-2.5190647348344,-0.795680734652675,
3.30605160560764));
#48852=CARTESIAN_POINT('Ctrl Pts',(-2.45277355760191,-1.90960928223922,
2.8136210252738));
#48853=CARTESIAN_POINT('Ctrl Pts',(-2.38648238036942,-2.5605348619571,1.96573923756561));
#48854=CARTESIAN_POINT('Ctrl Pts',(-2.34306377048867,-2.98687038633703,
1.41040366950969));
#48855=CARTESIAN_POINT('Ctrl Pts',(-2.29964516060792,-3.21458537852958,
0.702585476341522));
#48856=CARTESIAN_POINT('Ctrl Pts',(-2.25622655072717,-3.2194211246184,-0.00239241195666928));
#48857=CARTESIAN_POINT('Origin',(-111.877773449273,0.,0.));
#48858=CARTESIAN_POINT('',(-5.00277344927341,-3.22324707243039,-0.00294681091381338));
#48859=CARTESIAN_POINT('',(-4.75622655072715,-3.22711300261848,0.00159340525895835));
#48860=CARTESIAN_POINT('',(-111.877773449273,-3.22275,5.46201577318104E-12));
#48861=CARTESIAN_POINT('Ctrl Pts',(-5.00277344927341,-3.22324707243039,
-0.00294681091381289));
#48862=CARTESIAN_POINT('Ctrl Pts',(-4.98835640856205,-3.22541718997454,
-0.23632829062118));
#48863=CARTESIAN_POINT('Ctrl Pts',(-4.90764819061821,-3.09562804344372,
-1.54043009724623));
#48864=CARTESIAN_POINT('Ctrl Pts',(-4.76064879544187,-1.32045512479611,
-3.57577123082234));
#48865=CARTESIAN_POINT('Ctrl Pts',(-4.56177526374442,2.29438965018289,-3.04393130214526));
#48866=CARTESIAN_POINT('Ctrl Pts',(-4.36290173204696,3.80114449946005,0.284678958212554));
#48867=CARTESIAN_POINT('Ctrl Pts',(-4.1640282003495,1.81539998560147,3.35172560488281));
#48868=CARTESIAN_POINT('Ctrl Pts',(-3.96515466865207,-1.83833777717959,
3.33919988823347));
#48869=CARTESIAN_POINT('Ctrl Pts',(-3.82806975162671,-3.19259801208126,
1.21572803160912));
#48870=CARTESIAN_POINT('Ctrl Pts',(-3.75727601183384,-3.22780337920628,
0.0739550512688685));
#48871=CARTESIAN_POINT('Ctrl Pts',(-3.75277344927344,-3.22742925418368,
0.00131350936171882));
#48872=CARTESIAN_POINT('Ctrl Pts',(-4.75622655072715,-3.22711300261848,
0.00159340525895835));
#48873=CARTESIAN_POINT('Ctrl Pts',(-4.69551477683191,-3.22117852442416,
-0.978146732050712));
#48874=CARTESIAN_POINT('Ctrl Pts',(-4.56851182570419,-2.22157632985661,
-3.03814323849845));
#48875=CARTESIAN_POINT('Ctrl Pts',(-4.37521769734396,1.28684956643968,-3.58800221152922));
#48876=CARTESIAN_POINT('Ctrl Pts',(-4.17634416564651,3.71418555139234,-0.857068961927461));
#48877=CARTESIAN_POINT('Ctrl Pts',(-3.97747063394909,2.72892027452058,2.66134098575405));
#48878=CARTESIAN_POINT('Ctrl Pts',(-3.77859710225162,-0.76368264637654,
3.73450541646114));
#48879=CARTESIAN_POINT('Ctrl Pts',(-3.62151574117766,-2.96811382736398,
1.87194161459359));
#48880=CARTESIAN_POINT('Ctrl Pts',(-3.53072555733616,-3.22122698016124,
0.400063962610161));
#48881=CARTESIAN_POINT('Ctrl Pts',(-3.50622655072716,-3.21885503417064,
0.00210410441258326));
#48882=CARTESIAN_POINT('Origin',(-111.877773449273,0.,0.));
#48883=CARTESIAN_POINT('',(-6.25277344927341,-3.21740618512558,5.14541539371783E-5));
#48884=CARTESIAN_POINT('',(-6.00622655072713,-3.22378021337137,-0.00288641744942336));
#48885=CARTESIAN_POINT('',(-111.877773449273,-3.22275,5.46201577318104E-12));
#48886=CARTESIAN_POINT('Ctrl Pts',(-6.25277344927341,-3.21740663551856,
5.14498172248315E-5));
#48887=CARTESIAN_POINT('Ctrl Pts',(-6.21943680529028,-3.2173297520383,-0.542075897623197));
#48888=CARTESIAN_POINT('Ctrl Pts',(-6.11980898407466,-2.82991131366294,
-2.16234719346006));
#48889=CARTESIAN_POINT('Ctrl Pts',(-5.9538899856266,-0.260691166334333,
-3.80286493939216));
#48890=CARTESIAN_POINT('Ctrl Pts',(-5.75501645392915,3.05834644769266,-2.27513925674164));
#48891=CARTESIAN_POINT('Ctrl Pts',(-5.5561429222317,3.56736906587033,1.34298904651157));
#48892=CARTESIAN_POINT('Ctrl Pts',(-5.35726939053425,0.798685661716399,
3.72717625625544));
#48893=CARTESIAN_POINT('Ctrl Pts',(-5.17281289954814,-2.44992198009203,
2.76224489299424));
#48894=CARTESIAN_POINT('Ctrl Pts',(-5.05464758579454,-3.21543874504854,
0.83678604288195));
#48895=CARTESIAN_POINT('Ctrl Pts',(-5.00277344927341,-3.22324707243039,
-0.00294681091381289));
#48896=CARTESIAN_POINT('Ctrl Pts',(-6.00622655072713,-3.22378021337137,
-0.0028864174494234));
#48897=CARTESIAN_POINT('Ctrl Pts',(-5.99288635079263,-3.22578057906275,
-0.218744448328217));
#48898=CARTESIAN_POINT('Ctrl Pts',(-5.91325497362564,-3.10747272775033,
-1.50508027811392));
#48899=CARTESIAN_POINT('Ctrl Pts',(-5.76733241922618,-1.3783432033079,-3.55385869799583));
#48900=CARTESIAN_POINT('Ctrl Pts',(-5.5684588875287,2.24466082806341,-3.08078551666176));
#48901=CARTESIAN_POINT('Ctrl Pts',(-5.36958535583126,3.80526588113653,0.222919723353213));
#48902=CARTESIAN_POINT('Ctrl Pts',(-5.17071182413379,1.86958483045521,3.32180586330821));
#48903=CARTESIAN_POINT('Ctrl Pts',(-4.97183829243635,-1.78387460325836,
3.36860995647996));
#48904=CARTESIAN_POINT('Ctrl Pts',(-4.83367653463412,-3.18334407284146,
1.25090254757947));
#48905=CARTESIAN_POINT('Ctrl Pts',(-4.76180595406439,-3.22765838031572,
0.0916313837435054));
#48906=CARTESIAN_POINT('Ctrl Pts',(-4.75622655072715,-3.22711300261848,
0.00159340525895835));
#48907=CARTESIAN_POINT('Origin',(-111.877773449273,0.,0.));
#48908=CARTESIAN_POINT('',(-7.50277344927341,-3.22343654972774,0.00292891380799201));
#48909=CARTESIAN_POINT('',(-7.25622655072713,-3.21742169481438,-0.000238300387980783));
#48910=CARTESIAN_POINT('',(-111.877773449273,-3.22275,5.46201577318104E-12));
#48911=CARTESIAN_POINT('Ctrl Pts',(-7.50277344927341,-3.22343654972774,
0.00292891380799198));
#48912=CARTESIAN_POINT('Ctrl Pts',(-7.45051720201854,-3.21557264361966,
-0.842861996314261));
#48913=CARTESIAN_POINT('Ctrl Pts',(-7.33196977753116,-2.4407061395756,-2.77435554718224));
#48914=CARTESIAN_POINT('Ctrl Pts',(-7.14713117581134,0.820148624304898,
-3.72251230562602));
#48915=CARTESIAN_POINT('Ctrl Pts',(-6.94825764411385,3.57504823112902,-1.32241134923795));
#48916=CARTESIAN_POINT('Ctrl Pts',(-6.74938411241644,3.04518618264129,2.29272387010146));
#48917=CARTESIAN_POINT('Ctrl Pts',(-6.55051058071893,-0.282599183050784,
3.80129969000349));
#48918=CARTESIAN_POINT('Ctrl Pts',(-6.38497369300464,-2.83642887895705,
2.14981730773864));
#48919=CARTESIAN_POINT('Ctrl Pts',(-6.28572798252277,-3.21748263774626,
0.535964834069746));
#48920=CARTESIAN_POINT('Ctrl Pts',(-6.25277344927341,-3.21740663551856,
5.14498172248315E-5));
#48921=CARTESIAN_POINT('Ctrl Pts',(-7.25622655072713,-3.21742169481438,
-0.000238300387980818));
#48922=CARTESIAN_POINT('Ctrl Pts',(-7.22396674752086,-3.21776638258936,
-0.524847721982282));
#48923=CARTESIAN_POINT('Ctrl Pts',(-7.12541576708212,-2.84815011952815,
-2.12702754070791));
#48924=CARTESIAN_POINT('Ctrl Pts',(-6.96057360941086,-0.322406435201958,
-3.79813055621078));
#48925=CARTESIAN_POINT('Ctrl Pts',(-6.76170007771344,3.02100029278552,-2.32449970155028));
#48926=CARTESIAN_POINT('Ctrl Pts',(-6.56282654601595,3.58870574881201,1.28488625173232));
#48927=CARTESIAN_POINT('Ctrl Pts',(-6.36395301431852,0.85910099426281,3.71371607868986));
#48928=CARTESIAN_POINT('Ctrl Pts',(-6.17841968255555,-2.42380063763367,
2.79633723357069));
#48929=CARTESIAN_POINT('Ctrl Pts',(-6.0591775280251,-3.21584020356402,0.853914361307076));
#48930=CARTESIAN_POINT('Ctrl Pts',(-6.00622655072713,-3.22378021337137,
-0.0028864174494234));
#48931=CARTESIAN_POINT('Origin',(-111.877773449273,0.,0.));
#48932=CARTESIAN_POINT('',(-8.75277344927343,-3.22732301255539,-0.00141494957263923));
#48933=CARTESIAN_POINT('',(-8.50622655072714,-3.22290265484426,0.00296939138868677));
#48934=CARTESIAN_POINT('',(-111.877773449273,-3.22275,5.46201577318104E-12));
#48935=CARTESIAN_POINT('Ctrl Pts',(-8.75277344927343,-3.22732301255539,
-0.00141494957263976));
#48936=CARTESIAN_POINT('Ctrl Pts',(-8.74788877597928,-3.2277553807891,-0.0802281072649062));
#48937=CARTESIAN_POINT('Ctrl Pts',(-8.67671292545264,-3.18934882974505,
-1.22820668054782));
#48938=CARTESIAN_POINT('Ctrl Pts',(-8.53924589769349,-1.81906657383958,
-3.34973706899915));
#48939=CARTESIAN_POINT('Ctrl Pts',(-8.34037236599607,1.83468269579965,-3.34120951710917));
#48940=CARTESIAN_POINT('Ctrl Pts',(-8.14149883429859,3.80272173743456,-0.262771800485379));
#48941=CARTESIAN_POINT('Ctrl Pts',(-7.94262530260113,2.27681223869029,3.05710118596646));
#48942=CARTESIAN_POINT('Ctrl Pts',(-7.74375177090369,-1.34103701987869,
3.5681033256903));
#48943=CARTESIAN_POINT('Ctrl Pts',(-7.59713448646112,-3.09986887883355,
1.52788449672985));
#48944=CARTESIAN_POINT('Ctrl Pts',(-7.51680837925102,-3.22554862966795,
0.23009058007471));
#48945=CARTESIAN_POINT('Ctrl Pts',(-7.50277344927341,-3.22343654972774,
0.00292891380799198));
#48946=CARTESIAN_POINT('Ctrl Pts',(-8.50622655072714,-3.22290265484426,
0.00296939138868704));
#48947=CARTESIAN_POINT('Ctrl Pts',(-8.45504714424911,-3.21521886177093,
-0.825743966980133));
#48948=CARTESIAN_POINT('Ctrl Pts',(-8.33757656053859,-2.46652837635199,
-2.74018996961731));
#48949=CARTESIAN_POINT('Ctrl Pts',(-8.1538147995956,0.759595596975361,-3.73533882807744));
#48950=CARTESIAN_POINT('Ctrl Pts',(-7.95494126789815,3.55310402895249,-1.38028743054838));
#48951=CARTESIAN_POINT('Ctrl Pts',(-7.7560677362007,3.08201318363674,2.24297489227504));
#48952=CARTESIAN_POINT('Ctrl Pts',(-7.55719420450326,-0.220837703017022,
3.80538727863702));
#48953=CARTESIAN_POINT('Ctrl Pts',(-7.39058047601204,-2.81793219209313,
2.18511889975105));
#48954=CARTESIAN_POINT('Ctrl Pts',(-7.29025792475335,-3.21705807825673,
0.553180433440147));
#48955=CARTESIAN_POINT('Ctrl Pts',(-7.25622655072713,-3.21742169481438,
-0.000238300387980818));
#48956=CARTESIAN_POINT('Origin',(-111.877773449273,0.,0.));
#48957=CARTESIAN_POINT('',(-10.0027734492734,-3.21908627855254,-0.00223366033731866));
#48958=CARTESIAN_POINT('',(-9.75622655072715,-3.22760441255983,-0.00112366029274946));
#48959=CARTESIAN_POINT('',(-111.877773449273,-3.22275,5.46201577318104E-12));
#48960=CARTESIAN_POINT('Ctrl Pts',(-10.0027734492734,-3.21908627855254,
-0.00223366033731895));
#48961=CARTESIAN_POINT('Ctrl Pts',(-9.97896917270751,-3.22154382744801,
-0.388838697384529));
#48962=CARTESIAN_POINT('Ctrl Pts',(-9.88887371890911,-2.97789885064663,
-1.84908401298488));
#48963=CARTESIAN_POINT('Ctrl Pts',(-9.73248708787821,-0.80276370563772,
-3.72630005023728));
#48964=CARTESIAN_POINT('Ctrl Pts',(-9.53361355618079,2.70089004709043,-2.68978337139171));
#48965=CARTESIAN_POINT('Ctrl Pts',(-9.33474002448332,3.72296047888839,0.818111791946939));
#48966=CARTESIAN_POINT('Ctrl Pts',(-9.13586649278587,1.32436717843105,3.5743241610383));
#48967=CARTESIAN_POINT('Ctrl Pts',(-8.94187763438256,-2.20225640776817,
3.05940588394578));
#48968=CARTESIAN_POINT('Ctrl Pts',(-8.81417995321176,-3.22188759854761,
0.989365843077845));
#48969=CARTESIAN_POINT('Ctrl Pts',(-8.75277344927343,-3.22732301255539,
-0.00141494957263976));
#48970=CARTESIAN_POINT('Ctrl Pts',(-9.75622655072715,-3.22760441255983,
-0.00112366029274946));
#48971=CARTESIAN_POINT('Ctrl Pts',(-9.75241871820984,-3.22788084068667,
-0.0625480019197435));
#48972=CARTESIAN_POINT('Ctrl Pts',(-9.74861088569253,-3.22627989584886,
-0.123957647735919));
#48973=CARTESIAN_POINT('Ctrl Pts',(-9.74480305317522,-3.22275618026246,
-0.185256765088582));
#48974=CARTESIAN_POINT('Ctrl Pts',(-9.67851187594274,-3.1614112410109,-1.25242309505367));
#48975=CARTESIAN_POINT('Ctrl Pts',(-9.61222069871026,-2.51731494535359,
-2.28609057338361));
#48976=CARTESIAN_POINT('Ctrl Pts',(-9.54592952147779,-1.58636579276803,
-2.81139129933321));
#48977=CARTESIAN_POINT('Ctrl Pts',(-9.4796383442453,-0.65541664018237,-3.33669202528286));
#48978=CARTESIAN_POINT('Ctrl Pts',(-9.41334716701282,0.562385369331491,
-3.353625998852));
#48979=CARTESIAN_POINT('Ctrl Pts',(-9.34705598978033,1.50758074236322,-2.85441373519793));
#48980=CARTESIAN_POINT('Ctrl Pts',(-9.28076481254784,2.45277611539483,-2.35520147154391));
#48981=CARTESIAN_POINT('Ctrl Pts',(-9.21447363531536,3.12536485194425,-1.33984297066688));
#48982=CARTESIAN_POINT('Ctrl Pts',(-9.14818245808287,3.21635899593677,-0.274794970273445));
#48983=CARTESIAN_POINT('Ctrl Pts',(-9.0818912808504,3.30735313992928,0.790253030119865));
#48984=CARTESIAN_POINT('Ctrl Pts',(-9.01560010361792,2.8167526913648,1.90499053002971));
#48985=CARTESIAN_POINT('Ctrl Pts',(-8.94930892638544,1.96993999998221,2.55730597756723));
#48986=CARTESIAN_POINT('Ctrl Pts',(-8.88301774915295,1.12312730859944,3.20962142510489));
#48987=CARTESIAN_POINT('Ctrl Pts',(-8.81672657192045,-0.0798976256015836,
3.3995148202703));
#48988=CARTESIAN_POINT('Ctrl Pts',(-8.75043539468796,-1.08646391277993,
3.03974894237302));
#48989=CARTESIAN_POINT('Ctrl Pts',(-8.68414421745548,-2.09303019995817,
2.67998306447579));
#48990=CARTESIAN_POINT('Ctrl Pts',(-8.617853040223,-2.90313784011365,1.77055791351603));
#48991=CARTESIAN_POINT('Ctrl Pts',(-8.55156186299052,-3.14462255167314,
0.729264337493415));
#48992=CARTESIAN_POINT('Ctrl Pts',(-8.53645009223606,-3.19967153034788,
0.491890519952649));
#48993=CARTESIAN_POINT('Ctrl Pts',(-8.5213383214816,-3.22517145253926,0.247664028443626));
#48994=CARTESIAN_POINT('Ctrl Pts',(-8.50622655072714,-3.22290265484426,
0.00296939138868677));
#48995=CARTESIAN_POINT('Origin',(-111.877773449273,0.,0.));
#48996=CARTESIAN_POINT('',(-11.2527734492734,-3.21916848922627,0.00227587122066043));
#48997=CARTESIAN_POINT('',(-11.0062265507271,-3.21947286547661,-0.00241691677691058));
#48998=CARTESIAN_POINT('',(-111.877773449273,-3.22275,5.46201577318104E-12));
#48999=CARTESIAN_POINT('Ctrl Pts',(-11.2527734492734,-3.21916848922627,
0.00227587122066008));
#49000=CARTESIAN_POINT('Ctrl Pts',(-11.2100495694357,-3.21466710984026,
-0.691557780719506));
#49001=CARTESIAN_POINT('Ctrl Pts',(-11.1010345123656,-2.65353338684402,
-2.4685938576754));
#49002=CARTESIAN_POINT('Ctrl Pts',(-10.925728278063,0.278439380911714,-3.80160665280418));
#49003=CARTESIAN_POINT('Ctrl Pts',(-10.7268547463655,3.34874129613322,-1.82089905350606));
#49004=CARTESIAN_POINT('Ctrl Pts',(-10.5279812146681,3.34221283258897,1.83285433495541));
#49005=CARTESIAN_POINT('Ctrl Pts',(-10.3291076829706,0.264852355988142,
3.80257739711041));
#49006=CARTESIAN_POINT('Ctrl Pts',(-10.154038427839,-2.65838111784463,2.46091167050225));
#49007=CARTESIAN_POINT('Ctrl Pts',(-10.04526034994,-3.21469993916871,0.687795703115145));
#49008=CARTESIAN_POINT('Ctrl Pts',(-10.0027734492734,-3.21908627855254,
-0.00223366033731895));
#49009=CARTESIAN_POINT('Ctrl Pts',(-11.0062265507271,-3.21947286547661,
-0.00241691677691058));
#49010=CARTESIAN_POINT('Ctrl Pts',(-10.9834991149381,-3.22203123295323,
-0.371421649411236));
#49011=CARTESIAN_POINT('Ctrl Pts',(-10.960771679149,-3.1634971455758,-0.73963942385066));
#49012=CARTESIAN_POINT('Ctrl Pts',(-10.93804424336,-3.04034292773192,-1.08480060297804));
#49013=CARTESIAN_POINT('Ctrl Pts',(-10.8717530661275,-2.68112782939031,
-2.09156357930684));
#49014=CARTESIAN_POINT('Ctrl Pts',(-10.805461888895,-1.77214605123412,-2.90216867478603));
#49015=CARTESIAN_POINT('Ctrl Pts',(-10.7391707116625,-0.730984755342044,
-3.14422307635583));
#49016=CARTESIAN_POINT('Ctrl Pts',(-10.67287953443,0.310176540550037,-3.38627747792563));
#49017=CARTESIAN_POINT('Ctrl Pts',(-10.6065883571975,1.48351735417808,-3.05978118558606));
#49018=CARTESIAN_POINT('Ctrl Pts',(-10.540297179965,2.25000371116705,-2.31472693123087));
#49019=CARTESIAN_POINT('Ctrl Pts',(-10.4740060027326,3.01649006815602,-1.56967267687569));
#49020=CARTESIAN_POINT('Ctrl Pts',(-10.4077148255001,3.37612196850593,-0.40606046050502));
#49021=CARTESIAN_POINT('Ctrl Pts',(-10.3414236482676,3.16368414798498,0.641545071074154));
#49022=CARTESIAN_POINT('Ctrl Pts',(-10.2751324710351,2.95124632746403,1.68915060265333));
#49023=CARTESIAN_POINT('Ctrl Pts',(-10.2088412938026,2.16673878607194,2.62074944944104));
#49024=CARTESIAN_POINT('Ctrl Pts',(-10.1425501165701,1.17056509372838,3.00836414480955));
#49025=CARTESIAN_POINT('Ctrl Pts',(-10.0762589393376,0.174391401384763,
3.39597884017807));
#49026=CARTESIAN_POINT('Ctrl Pts',(-10.0099677621052,-1.03344844191028,
3.23960938412756));
#49027=CARTESIAN_POINT('Ctrl Pts',(-9.94367658487268,-1.89807157213503,
2.61109206530215));
#49028=CARTESIAN_POINT('Ctrl Pts',(-9.88119324015751,-2.71302987201674,
2.01867741932453));
#49029=CARTESIAN_POINT('Ctrl Pts',(-9.81870989544233,-3.22306845834968,
1.00679837785737));
#49030=CARTESIAN_POINT('Ctrl Pts',(-9.75622655072715,-3.22760441255983,
-0.00112366029274946));
#49031=CARTESIAN_POINT('Origin',(-111.877773449273,0.,0.));
#49032=CARTESIAN_POINT('',(-12.5027734492734,-3.2273897063871,0.00135230010112807));
#49033=CARTESIAN_POINT('',(-12.2562265507271,-3.21880858818939,0.00207596960425688));
#49034=CARTESIAN_POINT('',(-111.877773449273,-3.22275,5.46201577318104E-12));
#49035=CARTESIAN_POINT('Ctrl Pts',(-12.5027734492734,-3.2273897063871,0.00135230010112817));
#49036=CARTESIAN_POINT('Ctrl Pts',(-12.441129966164,-3.22213887174583,-0.993197620900722));
#49037=CARTESIAN_POINT('Ctrl Pts',(-12.3131953058221,-2.19561978059315,
-3.06664260054507));
#49038=CARTESIAN_POINT('Ctrl Pts',(-12.1189694682477,1.33713176289026,-3.56956864062838));
#49039=CARTESIAN_POINT('Ctrl Pts',(-11.9200959365502,3.72586027392076,-0.804802367483259));
#49040=CARTESIAN_POINT('Ctrl Pts',(-11.7212224048527,2.69126071506615,2.6994179733841));
#49041=CARTESIAN_POINT('Ctrl Pts',(-11.5223488731553,-0.816074714683047,
3.72340753766527));
#49042=CARTESIAN_POINT('Ctrl Pts',(-11.3661992212955,-2.98120175167232,
1.84128690775568));
#49043=CARTESIAN_POINT('Ctrl Pts',(-11.2763407466682,-3.22165153493936,
0.385007591278511));
#49044=CARTESIAN_POINT('Ctrl Pts',(-11.2527734492734,-3.21916848922627,
0.00227587122066008));
#49045=CARTESIAN_POINT('Ctrl Pts',(-12.2562265507271,-3.21880858818939,
0.00207596960425688));
#49046=CARTESIAN_POINT('Ctrl Pts',(-12.2145795116663,-3.21483379457629,
-0.674459605817695));
#49047=CARTESIAN_POINT('Ctrl Pts',(-12.106641295373,-2.67539305780387,-2.43366078039877));
#49048=CARTESIAN_POINT('Ctrl Pts',(-11.9324119018472,0.216673464944433,
-3.80562665550321));
#49049=CARTESIAN_POINT('Ctrl Pts',(-11.7335383701498,3.31873265494329,-1.87503471874537));
#49050=CARTESIAN_POINT('Ctrl Pts',(-11.5346648384523,3.37153346731751,1.77834296755299));
#49051=CARTESIAN_POINT('Ctrl Pts',(-11.3357913067549,0.326562407243348,
3.79777548384086));
#49052=CARTESIAN_POINT('Ctrl Pts',(-11.1596452108464,-2.63618345387206,
2.49579366496414));
#49053=CARTESIAN_POINT('Ctrl Pts',(-11.0497902921705,-3.21456901005255,
0.704887986120656));
#49054=CARTESIAN_POINT('Ctrl Pts',(-11.0062265507271,-3.21947286547661,
-0.00241691677691072));
#49055=CARTESIAN_POINT('Origin',(-111.877773449273,0.,0.));
#49056=CARTESIAN_POINT('',(-13.7527734492734,-3.22331905496246,-0.00294047133718037));
#49057=CARTESIAN_POINT('',(-13.5062265507271,-3.22706651782617,0.00162965321757597));
#49058=CARTESIAN_POINT('',(-111.877773449273,-3.22275,5.46201577318104E-12));
#49059=CARTESIAN_POINT('Ctrl Pts',(-13.7527734492734,-3.22331905496246,
-0.0029404713371806));
#49060=CARTESIAN_POINT('Ctrl Pts',(-13.7385015401247,-3.22546742958381,
-0.233959350890419));
#49061=CARTESIAN_POINT('Ctrl Pts',(-13.6579384537435,-3.09724369363227,
-1.53566484139185));
#49062=CARTESIAN_POINT('Ctrl Pts',(-13.5110841901299,-1.32827764686602,
-3.57287281110364));
#49063=CARTESIAN_POINT('Ctrl Pts',(-13.3122106584324,2.28772241734737,-3.04894535415999));
#49064=CARTESIAN_POINT('Ctrl Pts',(-13.113337126735,3.80175842718431,0.276359354501727));
#49065=CARTESIAN_POINT('Ctrl Pts',(-12.9144635950375,1.82273098807798,3.34774452080618));
#49066=CARTESIAN_POINT('Ctrl Pts',(-12.7155900633401,-1.83102542543786,
3.3432151475619));
#49067=CARTESIAN_POINT('Ctrl Pts',(-12.578360014752,-3.19136838569029,1.22046724841446));
#49068=CARTESIAN_POINT('Ctrl Pts',(-12.5074211433965,-3.2277856001957,0.076337742028997));
#49069=CARTESIAN_POINT('Ctrl Pts',(-12.5027734492734,-3.2273897063871,0.00135230010112817));
#49070=CARTESIAN_POINT('Ctrl Pts',(-13.5062265507271,-3.22706651782617,
0.00162965321757594));
#49071=CARTESIAN_POINT('Ctrl Pts',(-13.4456599083945,-3.22103553945658,
-0.975805603394261));
#49072=CARTESIAN_POINT('Ctrl Pts',(-13.3188020888295,-2.22558674433784,
-3.03369259275898));
#49073=CARTESIAN_POINT('Ctrl Pts',(-13.125653092032,1.27899402439183,-3.59080992494138));
#49074=CARTESIAN_POINT('Ctrl Pts',(-12.9267795603345,3.71230094882514,-0.865195525207697));
#49075=CARTESIAN_POINT('Ctrl Pts',(-12.727906028637,2.7347381391122,2.65536229956906));
#49076=CARTESIAN_POINT('Ctrl Pts',(-12.5290324969396,-0.755507687979863,
3.73616779131918));
#49077=CARTESIAN_POINT('Ctrl Pts',(-12.3718060043029,-2.96605047436436,
1.87671656148758));
#49078=CARTESIAN_POINT('Ctrl Pts',(-12.2808706888988,-3.22116062485788,
0.402407819712684));
#49079=CARTESIAN_POINT('Ctrl Pts',(-12.2562265507271,-3.21880858818939,
0.00207596960425688));
#49080=CARTESIAN_POINT('Origin',(-111.877773449273,0.,0.));
#49081=CARTESIAN_POINT('',(-15.0027734492734,-3.21740572002881,1.23680267080692E-5));
#49082=CARTESIAN_POINT('',(-14.7562265507271,-3.22385176614053,-0.00287592034953293));
#49083=CARTESIAN_POINT('',(-111.877773449273,-3.22275,5.46201577318104E-12));
#49084=CARTESIAN_POINT('Ctrl Pts',(-15.0027734492734,-3.21740594292328,
1.23675108736412E-5));
#49085=CARTESIAN_POINT('Ctrl Pts',(-14.9695819368529,-3.21738754235116,
-0.539755110259676));
#49086=CARTESIAN_POINT('Ctrl Pts',(-14.8700992472,-2.83239271434753,-2.15758856500936));
#49087=CARTESIAN_POINT('Ctrl Pts',(-14.7043253803146,-0.269013228516049,
-3.80228530154838));
#49088=CARTESIAN_POINT('Ctrl Pts',(-14.5054518486171,3.05335991141382,-2.28182709311162));
#49089=CARTESIAN_POINT('Ctrl Pts',(-14.3065783169197,3.5702996953566,1.33517853368896));
#49090=CARTESIAN_POINT('Ctrl Pts',(-14.1077047852222,0.806840788407417,
3.72541938225076));
#49091=CARTESIAN_POINT('Ctrl Pts',(-13.9231031626735,-2.44642853613299,
2.76684638869372));
#49092=CARTESIAN_POINT('Ctrl Pts',(-13.8047927173572,-3.21548850656084,
0.839093548266301));
#49093=CARTESIAN_POINT('Ctrl Pts',(-13.7527734492734,-3.22331905496246,
-0.0029404713371806));
#49094=CARTESIAN_POINT('Ctrl Pts',(-14.7562265507271,-3.22385176614053,
-0.00287592034953311));
#49095=CARTESIAN_POINT('Ctrl Pts',(-14.7430314823553,-3.22582786069339,
-0.216373387529147));
#49096=CARTESIAN_POINT('Ctrl Pts',(-14.6635452367509,-3.10904390727391,
-1.50031730597109));
#49097=CARTESIAN_POINT('Ctrl Pts',(-14.5177678139141,-1.38611763102972,
-3.55083364077171));
#49098=CARTESIAN_POINT('Ctrl Pts',(-14.3188942822166,2.23791305875133,-3.08569064764402));
#49099=CARTESIAN_POINT('Ctrl Pts',(-14.1200207505192,3.80574463510616,0.214591248302973));
#49100=CARTESIAN_POINT('Ctrl Pts',(-13.9211472188217,1.87685022649435,3.31770626469487));
#49101=CARTESIAN_POINT('Ctrl Pts',(-13.7222736871243,-1.77649802390547,
3.37250595292984));
#49102=CARTESIAN_POINT('Ctrl Pts',(-13.5839667977594,-3.18207374482736,
1.25564508237175));
#49103=CARTESIAN_POINT('Ctrl Pts',(-13.511951085627,-3.22763654358338,0.0940132165684776));
#49104=CARTESIAN_POINT('Ctrl Pts',(-13.5062265507271,-3.22706651782617,
0.00162965321757594));
#49105=CARTESIAN_POINT('Origin',(-111.877773449273,0.,0.));
#49106=CARTESIAN_POINT('',(-16.2527734492734,-3.22336460159151,0.00293616943835841));
#49107=CARTESIAN_POINT('',(-16.0062265507271,-3.21742729147399,-0.000277243005420702));
#49108=CARTESIAN_POINT('',(-111.877773449273,-3.22275,5.46201577318104E-12));
#49109=CARTESIAN_POINT('Ctrl Pts',(-16.2527734492734,-3.22336460159151,
0.00293616943835843));
#49110=CARTESIAN_POINT('Ctrl Pts',(-16.2006623335812,-3.21552069030317,
-0.840554018209381));
#49111=CARTESIAN_POINT('Ctrl Pts',(-16.0822600406565,-2.44421333433486,
-2.76975741814941));
#49112=CARTESIAN_POINT('Ctrl Pts',(-15.8975665704993,0.811999827878098,
-3.7242983112277));
#49113=CARTESIAN_POINT('Ctrl Pts',(-15.6986930388018,3.57214553169364,-1.33023228493699));
#49114=CARTESIAN_POINT('Ctrl Pts',(-15.4998195071044,3.05019658640061,2.28605389608329));
#49115=CARTESIAN_POINT('Ctrl Pts',(-15.3009459754069,-0.274279245362296,
3.80190906349047));
#49116=CARTESIAN_POINT('Ctrl Pts',(-15.1352639561299,-2.83395933390405,
2.1545767662713));
#49117=CARTESIAN_POINT('Ctrl Pts',(-15.0358731140854,-3.21742429257731,
0.538286199818229));
#49118=CARTESIAN_POINT('Ctrl Pts',(-15.0027734492734,-3.21740594292328,
1.23675108736412E-5));
#49119=CARTESIAN_POINT('Ctrl Pts',(-16.0062265507271,-3.21742729147399,
-0.000277243005420841));
#49120=CARTESIAN_POINT('Ctrl Pts',(-15.9741118790835,-3.21782654169675,
-0.522524268552057));
#49121=CARTESIAN_POINT('Ctrl Pts',(-15.8757060302074,-2.85057785483279,
-2.12226533114537));
#49122=CARTESIAN_POINT('Ctrl Pts',(-15.7110090040988,-0.330717988254753,
-3.79741586394379));
#49123=CARTESIAN_POINT('Ctrl Pts',(-15.5121354724014,3.01590581912008,-2.33110568651127));
#49124=CARTESIAN_POINT('Ctrl Pts',(-15.3132619407039,3.59150916741074,1.27702918208321));
#49125=CARTESIAN_POINT('Ctrl Pts',(-15.1143884090065,0.867226518337144,
3.71182701609064));
#49126=CARTESIAN_POINT('Ctrl Pts',(-14.9287099456809,-2.42024454403094,
2.80092311042059));
#49127=CARTESIAN_POINT('Ctrl Pts',(-14.8093226595878,-3.21590008839693,
0.856224194889351));
#49128=CARTESIAN_POINT('Ctrl Pts',(-14.7562265507271,-3.22385176614053,
-0.00287592034953311));
#49129=CARTESIAN_POINT('Origin',(-111.877773449273,0.,0.));
#49130=CARTESIAN_POINT('',(-17.5027734492734,-3.22736416564808,-0.00137668428022306));
#49131=CARTESIAN_POINT('',(-17.2562265507271,-3.22283081774483,0.00297248829486646));
#49132=CARTESIAN_POINT('',(-111.877773449273,-3.22275,5.46201577318104E-12));
#49133=CARTESIAN_POINT('Ctrl Pts',(-17.5027734492734,-3.22736416564808,
-0.00137668428022343));
#49134=CARTESIAN_POINT('Ctrl Pts',(-17.4980339075419,-3.22777406182281,
-0.0778455910693476));
#49135=CARTESIAN_POINT('Ctrl Pts',(-17.4270031885779,-3.19058738217639,
-1.22346672950067));
#49136=CARTESIAN_POINT('Ctrl Pts',(-17.2896812923814,-1.82639321974484,
-3.34574796396226));
#49137=CARTESIAN_POINT('Ctrl Pts',(-17.0908077606841,1.82736596257257,-3.34521677478736));
#49138=CARTESIAN_POINT('Ctrl Pts',(-16.8919342289865,3.8021375463979,-0.271093544295971));
#49139=CARTESIAN_POINT('Ctrl Pts',(-16.6930606972891,2.28349734576807,3.05211099132349));
#49140=CARTESIAN_POINT('Ctrl Pts',(-16.4941871655916,-1.33322490479584,
3.57102968129913));
#49141=CARTESIAN_POINT('Ctrl Pts',(-16.3474247495864,-3.09826305778849,
1.53264926624996));
#49142=CARTESIAN_POINT('Ctrl Pts',(-16.2669535108137,-3.2254990242249,0.232459997715443));
#49143=CARTESIAN_POINT('Ctrl Pts',(-16.2527734492734,-3.22336460159151,
0.00293616943835843));
#49144=CARTESIAN_POINT('Ctrl Pts',(-17.2562265507271,-3.22283081774483,
0.00297248829486629));
#49145=CARTESIAN_POINT('Ctrl Pts',(-17.2051922758117,-3.21517670414338,
-0.823437962111514));
#49146=CARTESIAN_POINT('Ctrl Pts',(-17.0878668236639,-2.46997325366766,
-2.73557685842927));
#49147=CARTESIAN_POINT('Ctrl Pts',(-16.9042501942836,0.75141887432542,-3.73699228080485));
#49148=CARTESIAN_POINT('Ctrl Pts',(-16.7053766625861,3.55007471849215,-1.38806020208435));
#49149=CARTESIAN_POINT('Ctrl Pts',(-16.5065031308886,3.08691462203722,2.23622444037719));
#49150=CARTESIAN_POINT('Ctrl Pts',(-16.3076295991912,-0.212508967422626,
3.80586147544186));
#49151=CARTESIAN_POINT('Ctrl Pts',(-16.1408707391373,-2.81540856813534,
2.18987439132723));
#49152=CARTESIAN_POINT('Ctrl Pts',(-16.040403056316,-3.2170024084915,0.555499212860509));
#49153=CARTESIAN_POINT('Ctrl Pts',(-16.0062265507271,-3.21742729147399,
-0.000277243005420841));
#49154=CARTESIAN_POINT('Origin',(-111.877773449273,0.,0.));
#49155=CARTESIAN_POINT('',(-18.7527734492734,-3.21913642963925,-0.00225963407795738));
#49156=CARTESIAN_POINT('',(-18.5062265507271,-3.2276379359672,-0.0010831830032082));
#49157=CARTESIAN_POINT('',(-111.877773449273,-3.22275,5.46201577318104E-12));
#49158=CARTESIAN_POINT('Ctrl Pts',(-18.7527734492734,-3.21913642963925,
-0.00225963407795737));
#49159=CARTESIAN_POINT('Ctrl Pts',(-18.7291143042701,-3.22160981599308,
-0.38649256276537));
#49160=CARTESIAN_POINT('Ctrl Pts',(-18.6391639820344,-2.97992372187582,
-1.84430888910775));
#49161=CARTESIAN_POINT('Ctrl Pts',(-18.4829224825662,-0.810916905050859,
-3.72453425337853));
#49162=CARTESIAN_POINT('Ctrl Pts',(-18.2840489508687,2.69499690552984,-2.69568791047329));
#49163=CARTESIAN_POINT('Ctrl Pts',(-18.0851754191713,3.72474202574661,0.809962019556789));
#49164=CARTESIAN_POINT('Ctrl Pts',(-17.8863018874738,1.33218652479678,3.57141718294536));
#49165=CARTESIAN_POINT('Ctrl Pts',(-17.6921678975079,-2.19819478851725,
3.06383880510527));
#49166=CARTESIAN_POINT('Ctrl Pts',(-17.5643250847744,-3.22204091260597,
0.991712214289981));
#49167=CARTESIAN_POINT('Ctrl Pts',(-17.5027734492734,-3.22736416564808,
-0.00137668428022343));
#49168=CARTESIAN_POINT('Ctrl Pts',(-18.5062265507271,-3.2276379359672,-0.00108318300320796));
#49169=CARTESIAN_POINT('Ctrl Pts',(-18.5025638497725,-3.22789541356105,
-0.0601647665002562));
#49170=CARTESIAN_POINT('Ctrl Pts',(-18.4326099715853,-3.19960698219719,
-1.18831160629045));
#49171=CARTESIAN_POINT('Ctrl Pts',(-18.2963649161657,-1.88047955591764,
-3.31565050499345));
#49172=CARTESIAN_POINT('Ctrl Pts',(-18.0974913844683,1.7728065417542,-3.37444789513792));
#49173=CARTESIAN_POINT('Ctrl Pts',(-17.8986178527708,3.79723434880727,-0.332795630568509));
#49174=CARTESIAN_POINT('Ctrl Pts',(-17.6997443210734,2.33275543941922,3.01462994268742));
#49175=CARTESIAN_POINT('Ctrl Pts',(-17.5008707893759,-1.27506395749001,
3.59220733474523));
#49176=CARTESIAN_POINT('Ctrl Pts',(-17.3530315325938,-3.08615971431661,
1.56801179161404));
#49177=CARTESIAN_POINT('Ctrl Pts',(-17.2714834530442,-3.22511904587652,
0.250031225518313));
#49178=CARTESIAN_POINT('Ctrl Pts',(-17.2562265507271,-3.22283081774483,
0.00297248829486629));
#49179=CARTESIAN_POINT('Origin',(-111.877773449273,0.,0.));
#49180=CARTESIAN_POINT('',(-20.0027734492734,-3.21911794458563,0.00225014293279763));
#49181=CARTESIAN_POINT('',(-19.7562265507271,-3.21952745218103,-0.00243989411713524));
#49182=CARTESIAN_POINT('',(-111.877773449273,-3.22275,5.46201577318104E-12));
#49183=CARTESIAN_POINT('Ctrl Pts',(-20.0027734492734,-3.21911794458563,
0.00225014293279763));
#49184=CARTESIAN_POINT('Ctrl Pts',(-19.9601947009984,-3.21468695194116,
-0.689253840355445));
#49185=CARTESIAN_POINT('Ctrl Pts',(-19.9176159527234,-2.99638332267943,
-1.38330928292528));
#49186=CARTESIAN_POINT('Ctrl Pts',(-19.8750372044484,-2.58522570477275,
-1.9331542933282));
#49187=CARTESIAN_POINT('Ctrl Pts',(-19.8087460272159,-1.9450912803623,-2.78921217458851));
#49188=CARTESIAN_POINT('Ctrl Pts',(-19.7424548499834,-0.837486249488049,
-3.29570954814478));
#49189=CARTESIAN_POINT('Ctrl Pts',(-19.6761636727509,0.228754499558577,
-3.21996100059655));
#49190=CARTESIAN_POINT('Ctrl Pts',(-19.6098724955184,1.29499524860508,-3.14421245304832));
#49191=CARTESIAN_POINT('Ctrl Pts',(-19.5435813182859,2.31987171582406,-2.48621798439587));
#49192=CARTESIAN_POINT('Ctrl Pts',(-19.4772901410535,2.83255459999984,-1.54826092905904));
#49193=CARTESIAN_POINT('Ctrl Pts',(-19.410998963821,3.34523748417564,-0.610303873722163));
#49194=CARTESIAN_POINT('Ctrl Pts',(-19.3447077865885,3.34572678530815,0.607615768299051));
#49195=CARTESIAN_POINT('Ctrl Pts',(-19.278416609356,2.83379771795475,1.54598446309963));
#49196=CARTESIAN_POINT('Ctrl Pts',(-19.2121254321235,2.32186865060138,2.48435315790015));
#49197=CARTESIAN_POINT('Ctrl Pts',(-19.145834254891,1.29752121476204,3.14317090548006));
#49198=CARTESIAN_POINT('Ctrl Pts',(-19.0795430776586,0.231341674093708,
3.21977615623486));
#49199=CARTESIAN_POINT('Ctrl Pts',(-19.0132519004261,-0.834837866574687,
3.29638140698965));
#49200=CARTESIAN_POINT('Ctrl Pts',(-18.9469607231936,-1.9428495120721,2.79077416091938));
#49201=CARTESIAN_POINT('Ctrl Pts',(-18.8806695459611,-2.58367157493215,
1.93523090594343));
#49202=CARTESIAN_POINT('Ctrl Pts',(-18.8380375137319,-2.99578594637027,
1.38502876529158));
#49203=CARTESIAN_POINT('Ctrl Pts',(-18.7954054815026,-3.21467957007237,
0.690099730433788));
#49204=CARTESIAN_POINT('Ctrl Pts',(-18.7527734492734,-3.21913642963925,
-0.00225963407795738));
#49205=CARTESIAN_POINT('Ctrl Pts',(-19.7562265507271,-3.21952745218103,
-0.00243989411713538));
#49206=CARTESIAN_POINT('Ctrl Pts',(-19.7336442465007,-3.22209647376765,
-0.369072624276772));
#49207=CARTESIAN_POINT('Ctrl Pts',(-19.6447707650418,-2.99474137424233,
-1.80887857682269));
#49208=CARTESIAN_POINT('Ctrl Pts',(-19.4896061063505,-0.871287725163321,
-3.71087581730611));
#49209=CARTESIAN_POINT('Ctrl Pts',(-19.290732574653,2.65086992728046,-2.7390929630313));
#49210=CARTESIAN_POINT('Ctrl Pts',(-19.0918590429556,3.73740284758043,0.749374129781112));
#49211=CARTESIAN_POINT('Ctrl Pts',(-18.8929855112581,1.39000235761673,3.5493147334813));
#49212=CARTESIAN_POINT('Ctrl Pts',(-18.6977746805153,-2.16778118645096,
3.09663127955505));
#49213=CARTESIAN_POINT('Ctrl Pts',(-18.5688550270049,-3.22323532991824,
1.00915204950376));
#49214=CARTESIAN_POINT('Ctrl Pts',(-18.5062265507271,-3.2276379359672,-0.00108318300320796));
#49215=CARTESIAN_POINT('Origin',(-111.877773449273,0.,0.));
#49216=CARTESIAN_POINT('',(-21.2527734492734,-3.22734916914202,0.00139077110789292));
#49217=CARTESIAN_POINT('',(-21.0062265507271,-3.21876282429886,0.00204748833280491));
#49218=CARTESIAN_POINT('',(-111.877773449273,-3.22275,5.46201577318104E-12));
#49219=CARTESIAN_POINT('Ctrl Pts',(-21.2527734492734,-3.22734916914202,
0.00139077110789292));
#49220=CARTESIAN_POINT('Ctrl Pts',(-21.1912750977266,-3.2219844149411,-0.990850652625185));
#49221=CARTESIAN_POINT('Ctrl Pts',(-21.1297767461798,-2.73000666275173,
-1.98768731231595));
#49222=CARTESIAN_POINT('Ctrl Pts',(-21.0682783946331,-1.93664422845416,
-2.58261235938075));
#49223=CARTESIAN_POINT('Ctrl Pts',(-21.0019872174006,-1.0814517164788,-3.22390242233522));
#49224=CARTESIAN_POINT('Ctrl Pts',(-20.9356960401681,0.123932366897174,
-3.39819443414427));
#49225=CARTESIAN_POINT('Ctrl Pts',(-20.8694048629357,1.12575333627981,-3.02541846564833));
#49226=CARTESIAN_POINT('Ctrl Pts',(-20.8031136857032,2.12757430566257,-2.65264249715234));
#49227=CARTESIAN_POINT('Ctrl Pts',(-20.7368225084707,2.92583216105199,-1.73279854835118));
#49228=CARTESIAN_POINT('Ctrl Pts',(-20.6705313312382,3.15380642416163,-0.688463873669388));
#49229=CARTESIAN_POINT('Ctrl Pts',(-20.6042401540057,3.38178068727125,0.355870801012347));
#49230=CARTESIAN_POINT('Ctrl Pts',(-20.5379489767732,3.03947135810111,1.52469620157494));
#49231=CARTESIAN_POINT('Ctrl Pts',(-20.4716577995407,2.2841356938992,2.28105273904104));
#49232=CARTESIAN_POINT('Ctrl Pts',(-20.4053666223082,1.52880002969724,3.03740927650718));
#49233=CARTESIAN_POINT('Ctrl Pts',(-20.3390754450758,0.360438030463874,
3.3812969508769));
#49234=CARTESIAN_POINT('Ctrl Pts',(-20.2727842678433,-0.684203601870848,
3.15473341149739));
#49235=CARTESIAN_POINT('Ctrl Pts',(-20.2064930906108,-1.72884523420545,
2.9281698721179));
#49236=CARTESIAN_POINT('Ctrl Pts',(-20.1402019133783,-2.64976649964112,
2.13115511898911));
#49237=CARTESIAN_POINT('Ctrl Pts',(-20.0739107361458,-3.02389522338553,
1.12983854794265));
#49238=CARTESIAN_POINT('Ctrl Pts',(-20.0501983071884,-3.15772149036564,
0.771666479710817));
#49239=CARTESIAN_POINT('Ctrl Pts',(-20.0264858782309,-3.22158559811115,
0.387353973877421));
#49240=CARTESIAN_POINT('Ctrl Pts',(-20.0027734492734,-3.21911794458563,
0.00225014293279763));
#49241=CARTESIAN_POINT('Ctrl Pts',(-21.0062265507271,-3.21876282429886,
0.00204748833280501));
#49242=CARTESIAN_POINT('Ctrl Pts',(-20.964724643229,-3.21485961808616,-0.672154526158193));
#49243=CARTESIAN_POINT('Ctrl Pts',(-20.8569315584983,-2.67830623265808,
-2.42894787761703));
#49244=CARTESIAN_POINT('Ctrl Pts',(-20.6828472965351,0.20834421543868,-3.80609173817195));
#49245=CARTESIAN_POINT('Ctrl Pts',(-20.4839737648378,3.31462113615585,-1.88229337650549));
#49246=CARTESIAN_POINT('Ctrl Pts',(-20.2851002331403,3.37541735115235,1.77096000435559));
#49247=CARTESIAN_POINT('Ctrl Pts',(-20.0862267014428,0.334873173258265,
3.79705169695109));
#49248=CARTESIAN_POINT('Ctrl Pts',(-19.9099354739718,-2.63315844852102,
2.50048966296161));
#49249=CARTESIAN_POINT('Ctrl Pts',(-19.7999354237332,-3.21455501725349,
0.707191119696958));
#49250=CARTESIAN_POINT('Ctrl Pts',(-19.7562265507271,-3.21952745218103,
-0.00243989411713538));
#49251=CARTESIAN_POINT('Origin',(-111.877773449273,0.,0.));
#49252=CARTESIAN_POINT('',(-22.5027734492734,-3.22339102037588,-0.00293357075097584));
#49253=CARTESIAN_POINT('',(-22.2562265507271,-3.22701916559281,0.00166552852483643));
#49254=CARTESIAN_POINT('',(-111.877773449273,-3.22275,5.46201577318104E-12));
#49255=CARTESIAN_POINT('Ctrl Pts',(-22.5027734492734,-3.22339102037588,
-0.00293357075097572));
#49256=CARTESIAN_POINT('Ctrl Pts',(-22.4886466716873,-3.22551728192709,
-0.231590117755942));
#49257=CARTESIAN_POINT('Ctrl Pts',(-22.4082287168688,-3.0988533213393,-1.53089988227506));
#49258=CARTESIAN_POINT('Ctrl Pts',(-22.2615195848178,-1.33609380754272,
-3.56995727830645));
#49259=CARTESIAN_POINT('Ctrl Pts',(-22.0626460531204,2.28104422824517,-3.05394480308283));
#49260=CARTESIAN_POINT('Ctrl Pts',(-21.8637725214229,3.80235414351597,0.268038427794315));
#49261=CARTESIAN_POINT('Ctrl Pts',(-21.6648989897255,1.83005326445484,3.34374740085816));
#49262=CARTESIAN_POINT('Ctrl Pts',(-21.466025458028,-1.82370431158557,3.34721439638869));
#49263=CARTESIAN_POINT('Ctrl Pts',(-21.3286502778773,-3.19013329224575,
1.22520691434576));
#49264=CARTESIAN_POINT('Ctrl Pts',(-21.2575662749591,-3.22776726704359,
0.0787203264943862));
#49265=CARTESIAN_POINT('Ctrl Pts',(-21.2527734492734,-3.22734916914202,
0.00139077110789282));
#49266=CARTESIAN_POINT('Ctrl Pts',(-22.2562265507271,-3.22701916559281,
0.00166552852483633));
#49267=CARTESIAN_POINT('Ctrl Pts',(-22.1958050399572,-3.22089431753202,
-0.973465341318993));
#49268=CARTESIAN_POINT('Ctrl Pts',(-22.0690923519548,-2.22958833490889,
-3.02923894111559));
#49269=CARTESIAN_POINT('Ctrl Pts',(-21.8760884867199,1.27113236380313,-3.59360044317391));
#49270=CARTESIAN_POINT('Ctrl Pts',(-21.6772149550225,3.71039855154082,-0.873317937644316));
#49271=CARTESIAN_POINT('Ctrl Pts',(-21.478341423325,2.74054293166321,2.64937088215266));
#49272=CARTESIAN_POINT('Ctrl Pts',(-21.2794678916276,-0.747329160908197,
3.73781229554719));
#49273=CARTESIAN_POINT('Ctrl Pts',(-21.1220962674282,-2.96398036377416,
1.88149141963838));
#49274=CARTESIAN_POINT('Ctrl Pts',(-21.0310158204614,-3.22109422633476,
0.404751281969014));
#49275=CARTESIAN_POINT('Ctrl Pts',(-21.0062265507271,-3.21876282429886,
0.00204748833280501));
#49276=CARTESIAN_POINT('Origin',(-111.877773449273,0.,0.));
#49277=CARTESIAN_POINT('',(-23.7527734492733,-3.21740582208574,-2.67182391447498E-5));
#49278=CARTESIAN_POINT('',(-23.5062265507271,-3.22392320659701,-0.00286486488396187));
#49279=CARTESIAN_POINT('',(-111.877773449273,-3.22275,5.46201577318104E-12));
#49280=CARTESIAN_POINT('Ctrl Pts',(-23.7527734492733,-3.21740609865336,
-2.67168564435302E-5));
#49281=CARTESIAN_POINT('Ctrl Pts',(-23.7197270684156,-3.2174456747296,-0.537433969267299));
#49282=CARTESIAN_POINT('Ctrl Pts',(-23.6203895103253,-2.83486685131597,
-2.15282942535465));
#49283=CARTESIAN_POINT('Ctrl Pts',(-23.4547607750025,-0.277334002226216,
-3.80168745200032));
#49284=CARTESIAN_POINT('Ctrl Pts',(-23.2558872433051,3.04835875056794,-2.28850400028564));
#49285=CARTESIAN_POINT('Ctrl Pts',(-23.0570137116076,3.57321322422885,1.32736162581399));
#49286=CARTESIAN_POINT('Ctrl Pts',(-22.8581401799102,0.814992050687579,
3.7236446646805));
#49287=CARTESIAN_POINT('Ctrl Pts',(-22.6733934257988,-2.44292667337299,
2.77144582727945));
#49288=CARTESIAN_POINT('Ctrl Pts',(-22.5549378489198,-3.21553960793346,
0.841401340527108));
#49289=CARTESIAN_POINT('Ctrl Pts',(-22.5027734492734,-3.22339102037588,
-0.00293357075097572));
#49290=CARTESIAN_POINT('Ctrl Pts',(-23.5062265507271,-3.22392320659701,
-0.00286486488396215));
#49291=CARTESIAN_POINT('Ctrl Pts',(-23.4931766139179,-3.22587472894888,
-0.214002050993878));
#49292=CARTESIAN_POINT('Ctrl Pts',(-23.4138354998762,-3.11060913095701,
-1.49555465574787));
#49293=CARTESIAN_POINT('Ctrl Pts',(-23.2682032086021,-1.39388541978934,
-3.54779157617611));
#49294=CARTESIAN_POINT('Ctrl Pts',(-23.0693296769047,2.23115457073302,-3.09058099925963));
#49295=CARTESIAN_POINT('Ctrl Pts',(-22.8704561452071,3.8062051604974,0.206261745581809));
#49296=CARTESIAN_POINT('Ctrl Pts',(-22.6715826135097,1.8841066336201,3.31359077507109));
#49297=CARTESIAN_POINT('Ctrl Pts',(-22.4727090818123,-1.76911293681183,
3.37638579672));
#49298=CARTESIAN_POINT('Ctrl Pts',(-22.3342570608847,-3.18079789745064,
1.26038805836638));
#49299=CARTESIAN_POINT('Ctrl Pts',(-22.2620962171897,-3.22761416586329,
0.0963949202665974));
#49300=CARTESIAN_POINT('Ctrl Pts',(-22.2562265507271,-3.22701916559281,
0.00166552852483633));
#49301=CARTESIAN_POINT('Origin',(-111.877773449273,0.,0.));
#49302=CARTESIAN_POINT('',(-25.0027734492734,-3.22329262847075,0.00294286404255992));
#49303=CARTESIAN_POINT('',(-24.7562265507271,-3.21743373373988,-0.000316139430206752));
#49304=CARTESIAN_POINT('',(-111.877773449273,-3.22275,5.46201577318104E-12));
#49305=CARTESIAN_POINT('Ctrl Pts',(-25.0027734492734,-3.22329262847075,
0.00294286404255977));
#49306=CARTESIAN_POINT('Ctrl Pts',(-24.9508074651438,-3.21547008177197,
-0.838246332242223));
#49307=CARTESIAN_POINT('Ctrl Pts',(-24.8325503037818,-2.44771210523894,
-2.76515722257126));
#49308=CARTESIAN_POINT('Ctrl Pts',(-24.6480019651872,0.803847142238303,
-3.72606647866122));
#49309=CARTESIAN_POINT('Ctrl Pts',(-24.4491284334898,3.56922572285289,-1.33804684925931));
#49310=CARTESIAN_POINT('Ctrl Pts',(-24.2502549017923,3.05519238071696,2.27937297261687));
#49311=CARTESIAN_POINT('Ctrl Pts',(-24.0513813700949,-0.265957993964293,
3.80250022707872));
#49312=CARTESIAN_POINT('Ctrl Pts',(-23.8855542192552,-2.8314825312375,2.15933571928619));
#49313=CARTESIAN_POINT('Ctrl Pts',(-23.786018245648,-3.21736628495631,0.540607210760987));
#49314=CARTESIAN_POINT('Ctrl Pts',(-23.7527734492733,-3.21740609865336,
-2.67168564435302E-5));
#49315=CARTESIAN_POINT('Ctrl Pts',(-24.7562265507271,-3.21743373373988,
-0.000316139430206856));
#49316=CARTESIAN_POINT('Ctrl Pts',(-24.7242570106461,-3.21788699032318,
-0.520200448775454));
#49317=CARTESIAN_POINT('Ctrl Pts',(-24.6259962933327,-2.85299839799472,
-2.11750267593112));
#49318=CARTESIAN_POINT('Ctrl Pts',(-24.4614443987868,-0.339027957278562,
-3.79668298329881));
#49319=CARTESIAN_POINT('Ctrl Pts',(-24.2625708670894,3.01079690025812,-2.33770050624184));
#49320=CARTESIAN_POINT('Ctrl Pts',(-24.0636973353919,3.59429538385108,1.26916599588641));
#49321=CARTESIAN_POINT('Ctrl Pts',(-23.8648238036945,0.87534788869354,3.70992017505057));
#49322=CARTESIAN_POINT('Ctrl Pts',(-23.6790002088062,-2.41667997468913,
2.80550681899019));
#49323=CARTESIAN_POINT('Ctrl Pts',(-23.5594677911504,-3.21596136952096,
0.858534378066973));
#49324=CARTESIAN_POINT('Ctrl Pts',(-23.5062265507271,-3.22392320659701,
-0.00286486488396215));
#49325=CARTESIAN_POINT('Origin',(-111.877773449273,0.,0.));
#49326=CARTESIAN_POINT('',(-26.2527734492733,-3.22740434264695,-0.00133809533540642));
#49327=CARTESIAN_POINT('',(-26.0062265507271,-3.22275904721707,0.0029750263946704));
#49328=CARTESIAN_POINT('',(-111.877773449273,-3.22275,5.46201577318104E-12));
#49329=CARTESIAN_POINT('Ctrl Pts',(-26.2527734492733,-3.22740434264695,
-0.00133809533540624));
#49330=CARTESIAN_POINT('Ctrl Pts',(-26.2481790391045,-3.2277921929266,-0.075462967587538));
#49331=CARTESIAN_POINT('Ctrl Pts',(-26.1772934517032,-3.19182047039241,
-1.21872722919777));
#49332=CARTESIAN_POINT('Ctrl Pts',(-26.0401166870694,-1.83371111782523,
-3.34174283388943));
#49333=CARTESIAN_POINT('Ctrl Pts',(-25.841243155372,1.82004047686151,-3.34920800997384));
#49334=CARTESIAN_POINT('Ctrl Pts',(-25.6423696236745,3.80153514436882,-0.279413989657449));
#49335=CARTESIAN_POINT('Ctrl Pts',(-25.4434960919771,2.29017151564223,3.04710617806936));
#49336=CARTESIAN_POINT('Ctrl Pts',(-25.2446225602796,-1.32540640400279,
3.57393893284649));
#49337=CARTESIAN_POINT('Ctrl Pts',(-25.0977150127117,-3.09665122005086,
1.53741433471344));
#49338=CARTESIAN_POINT('Ctrl Pts',(-25.0170986423763,-3.22544902931438,
0.234829123385659));
#49339=CARTESIAN_POINT('Ctrl Pts',(-25.0027734492734,-3.22329262847075,
0.00294286404255977));
#49340=CARTESIAN_POINT('Ctrl Pts',(-26.0062265507271,-3.22275904721707,
0.00297502639467036));
#49341=CARTESIAN_POINT('Ctrl Pts',(-25.9553374073744,-3.21513583440698,
-0.82113218938988));
#49342=CARTESIAN_POINT('Ctrl Pts',(-25.8381570867892,-2.47340976517071,
-2.73096178962243));
#49343=CARTESIAN_POINT('Ctrl Pts',(-25.6546855889715,0.74323855262528,-3.73862783456431));
#49344=CARTESIAN_POINT('Ctrl Pts',(-25.4558120572741,3.54702840433774,-1.39582632526716));
#49345=CARTESIAN_POINT('Ctrl Pts',(-25.2569385255766,3.09180127512853,2.22946327769737));
#49346=CARTESIAN_POINT('Ctrl Pts',(-25.0580649938792,-0.204179213979529,
3.80631744341775));
#49347=CARTESIAN_POINT('Ctrl Pts',(-24.8911610022627,-2.81287761522076,
2.19462930958641));
#49348=CARTESIAN_POINT('Ctrl Pts',(-24.7905481878786,-3.21694712968023,
0.55781765232775));
#49349=CARTESIAN_POINT('Ctrl Pts',(-24.7562265507271,-3.21743373373988,
-0.000316139430206856));
#49350=CARTESIAN_POINT('Origin',(-111.877773449273,0.,0.));
#49351=CARTESIAN_POINT('',(-27.5027734492733,-3.21918720133157,-0.00228521908616954));
#49352=CARTESIAN_POINT('',(-27.2562265507271,-3.22767036229815,-0.00104244248707641));
#49353=CARTESIAN_POINT('',(-111.877773449273,-3.22275,5.46201577318104E-12));
#49354=CARTESIAN_POINT('Ctrl Pts',(-27.5027734492733,-3.21918720133157,
-0.00228521908616927));
#49355=CARTESIAN_POINT('Ctrl Pts',(-27.4792594358328,-3.22167572177667,
-0.384146036416285));
#49356=CARTESIAN_POINT('Ctrl Pts',(-27.3894542451597,-2.98194196490443,
-1.83953375038598));
#49357=CARTESIAN_POINT('Ctrl Pts',(-27.2333578772542,-0.819066220437877,
-3.72275061722178));
#49358=CARTESIAN_POINT('Ctrl Pts',(-27.0344843455567,2.68909085581776,-2.70157953809338));
#49359=CARTESIAN_POINT('Ctrl Pts',(-26.8356108138592,3.72650573231153,0.801808367714392));
#49360=CARTESIAN_POINT('Ctrl Pts',(-26.6367372821618,1.33999949042545,3.56849309893504));
#49361=CARTESIAN_POINT('Ctrl Pts',(-26.4424581606331,-2.19412430154369,
3.06826860367683));
#49362=CARTESIAN_POINT('Ctrl Pts',(-26.314470216337,-3.22219603353229,0.994059531111112));
#49363=CARTESIAN_POINT('Ctrl Pts',(-26.2527734492733,-3.22740434264695,
-0.00133809533540624));
#49364=CARTESIAN_POINT('Ctrl Pts',(-27.2562265507271,-3.22767036229815,
-0.00104244248707691));
#49365=CARTESIAN_POINT('Ctrl Pts',(-27.2527089813351,-3.22790942823879,
-0.0577814477878739));
#49366=CARTESIAN_POINT('Ctrl Pts',(-27.1829002347107,-3.20079977205244,
-1.18357548571261));
#49367=CARTESIAN_POINT('Ctrl Pts',(-27.0468003108537,-1.88773145525861,
-3.31152707739417));
#49368=CARTESIAN_POINT('Ctrl Pts',(-26.8479267791563,1.765417213501,-3.37831965535559));
#49369=CARTESIAN_POINT('Ctrl Pts',(-26.6490532474588,3.79649692161308,-0.341105197365262));
#49370=CARTESIAN_POINT('Ctrl Pts',(-26.4501797157614,2.33934746290421,3.00951741634616));
#49371=CARTESIAN_POINT('Ctrl Pts',(-26.2513061840639,-1.26719924803898,
3.5949892485593));
#49372=CARTESIAN_POINT('Ctrl Pts',(-26.1033217957191,-3.08450295152784,
1.57277896528229));
#49373=CARTESIAN_POINT('Ctrl Pts',(-26.0216285846069,-3.22506627768389,
0.252398113950421));
#49374=CARTESIAN_POINT('Ctrl Pts',(-26.0062265507271,-3.22275904721707,
0.00297502639467036));
#49375=CARTESIAN_POINT('Origin',(-111.877773449273,0.,0.));
#49376=CARTESIAN_POINT('',(-28.7527734492734,-3.21906802306727,0.00222402768671319));
#49377=CARTESIAN_POINT('',(-28.506226550727,-3.21958260577835,-0.0024624483620983));
#49378=CARTESIAN_POINT('',(-111.877773449273,-3.22275,5.46201577318104E-12));
#49379=CARTESIAN_POINT('Ctrl Pts',(-28.7527734492734,-3.21906802306727,
0.00222402768671311));
#49380=CARTESIAN_POINT('Ctrl Pts',(-28.710339832561,-3.21470762532615,-0.686949761698418));
#49381=CARTESIAN_POINT('Ctrl Pts',(-28.6016150386162,-2.65946822477964,
-2.45918392203356));
#49382=CARTESIAN_POINT('Ctrl Pts',(-28.4265990674389,0.261796888079818,
-3.80278897927288));
#49383=CARTESIAN_POINT('Ctrl Pts',(-28.2277255357414,3.34073904970577,-1.83553922138932));
#49384=CARTESIAN_POINT('Ctrl Pts',(-28.028852004044,3.35020331301418,1.81820774196901));
#49385=CARTESIAN_POINT('Ctrl Pts',(-27.8299784723465,0.281493893444737,
3.80138169873015));
#49386=CARTESIAN_POINT('Ctrl Pts',(-27.6546189540897,-2.6524404997523,2.47032073267811));
#49387=CARTESIAN_POINT('Ctrl Pts',(-27.5455506130652,-3.21466003513985,
0.692403621248377));
#49388=CARTESIAN_POINT('Ctrl Pts',(-27.5027734492733,-3.21918720133157,
-0.00228521908616927));
#49389=CARTESIAN_POINT('Ctrl Pts',(-28.506226550727,-3.21958260577835,-0.00246244836209827));
#49390=CARTESIAN_POINT('Ctrl Pts',(-28.4837893780633,-3.22216159046997,
-0.366723212734714));
#49391=CARTESIAN_POINT('Ctrl Pts',(-28.3950610281671,-2.99671073763452,
-1.80410351630265));
#49392=CARTESIAN_POINT('Ctrl Pts',(-28.2400415010384,-0.879407004066094,
-3.70896009046836));
#49393=CARTESIAN_POINT('Ctrl Pts',(-28.041167969341,2.64486898995689,-2.74488791345875));
#49394=CARTESIAN_POINT('Ctrl Pts',(-27.8422944376435,3.73903392537052,0.741192914439823));
#49395=CARTESIAN_POINT('Ctrl Pts',(-27.6434209059461,1.3977668128979,3.54626417068001));
#49396=CARTESIAN_POINT('Ctrl Pts',(-27.4480649436406,-2.16364472461151,
3.10103735652865));
#49397=CARTESIAN_POINT('Ctrl Pts',(-27.3190001585676,-3.22340405510307,
1.01150675587474));
#49398=CARTESIAN_POINT('Ctrl Pts',(-27.2562265507271,-3.22767036229815,
-0.00104244248707691));
#49399=CARTESIAN_POINT('Origin',(-111.877773449273,0.,0.));
#49400=CARTESIAN_POINT('',(-30.0027734492733,-3.22730766174399,0.00142891566604214));
#49401=CARTESIAN_POINT('',(-29.7562265507271,-3.21871773150106,0.0020186574082677));
#49402=CARTESIAN_POINT('',(-111.877773449273,-3.22275,5.46201577318104E-12));
#49403=CARTESIAN_POINT('Ctrl Pts',(-30.0027734492733,-3.22730766174399,
0.00142891566604205));
#49404=CARTESIAN_POINT('Ctrl Pts',(-29.9414202292892,-3.22183176265191,
-0.988504625625889));
#49405=CARTESIAN_POINT('Ctrl Pts',(-29.8137758320727,-2.20374537616861,
-3.05777759031298));
#49406=CARTESIAN_POINT('Ctrl Pts',(-29.6198402576236,1.32149477066622,-3.57538714023941));
#49407=CARTESIAN_POINT('Ctrl Pts',(-29.4209667259261,3.72230192179151,-0.821102937831022));
#49408=CARTESIAN_POINT('Ctrl Pts',(-29.2220931942287,2.70305042427431,2.68761232980465));
#49409=CARTESIAN_POINT('Ctrl Pts',(-29.0232196625312,-0.799769353165428,
3.72694387041513));
#49410=CARTESIAN_POINT('Ctrl Pts',(-28.8667797475461,-2.97715376913023,
1.85083715862348));
#49411=CARTESIAN_POINT('Ctrl Pts',(-28.7766310097935,-3.22151958060727,
0.389699964527589));
#49412=CARTESIAN_POINT('Ctrl Pts',(-28.7527734492734,-3.21906802306727,
0.00222402768671311));
#49413=CARTESIAN_POINT('Ctrl Pts',(-29.7562265507271,-3.21871773150106,
0.00201865740826774));
#49414=CARTESIAN_POINT('Ctrl Pts',(-29.7148697747916,-3.21488621482395,
-0.669849273457447));
#49415=CARTESIAN_POINT('Ctrl Pts',(-29.6072218216236,-2.68121160462978,
-2.42423387462879));
#49416=CARTESIAN_POINT('Ctrl Pts',(-29.4332826912232,0.200013968032432,
-3.80653859090899));
#49417=CARTESIAN_POINT('Ctrl Pts',(-29.2344091595257,3.31049374141978,-1.88954301869738));
#49418=CARTESIAN_POINT('Ctrl Pts',(-29.0355356278283,3.37928506784462,1.76356855884025));
#49419=CARTESIAN_POINT('Ctrl Pts',(-28.8366620961308,0.343182335340544,
3.79630972342846));
#49420=CARTESIAN_POINT('Ctrl Pts',(-28.6602257370971,-2.63012550325009,
2.50518437947119));
#49421=CARTESIAN_POINT('Ctrl Pts',(-28.5500805552958,-3.21454191691153,
0.709494154389844));
#49422=CARTESIAN_POINT('Ctrl Pts',(-28.506226550727,-3.21958260577835,-0.00246244836209827));
#49423=CARTESIAN_POINT('Origin',(-111.877773449273,0.,0.));
#49424=CARTESIAN_POINT('',(-31.2527734492733,-3.22346295616709,-0.00292610916508903));
#49425=CARTESIAN_POINT('',(-31.0062265507271,-3.22697096224228,0.00170102469852499));
#49426=CARTESIAN_POINT('',(-111.877773449273,-3.22275,5.46201577318104E-12));
#49427=CARTESIAN_POINT('Ctrl Pts',(-31.2527734492733,-3.22346295616709,
-0.00292610916508954));
#49428=CARTESIAN_POINT('Ctrl Pts',(-31.23879180325,-3.22556674346952,-0.229220593505158));
#49429=CARTESIAN_POINT('Ctrl Pts',(-31.1585189799941,-3.10045693566244,
-1.52613522338862));
#49430=CARTESIAN_POINT('Ctrl Pts',(-31.0119549795058,-1.34390356876819,
-3.56702464658427));
#49431=CARTESIAN_POINT('Ctrl Pts',(-30.8130814478083,2.27435511368902,-3.05892962461122));
#49432=CARTESIAN_POINT('Ctrl Pts',(-30.6142079161109,3.80293164781777,0.259716217270925));
#49433=CARTESIAN_POINT('Ctrl Pts',(-30.4153343844134,1.83736677547631,3.33973426545636));
#49434=CARTESIAN_POINT('Ctrl Pts',(-30.216460852716,-1.81637446278761,3.35119761315571));
#49435=CARTESIAN_POINT('Ctrl Pts',(-30.0789405410026,-3.18889273168686,
1.22994703057292));
#49436=CARTESIAN_POINT('Ctrl Pts',(-30.0077114065217,-3.22774838442522,
0.0811028024957301));
#49437=CARTESIAN_POINT('Ctrl Pts',(-30.0027734492733,-3.22730766174399,
0.00142891566604205));
#49438=CARTESIAN_POINT('Ctrl Pts',(-31.0062265507271,-3.22697096224228,
0.00170102469852487));
#49439=CARTESIAN_POINT('Ctrl Pts',(-30.9459501715198,-3.22075485181861,
-0.971125934525062));
#49440=CARTESIAN_POINT('Ctrl Pts',(-30.8193826150801,-2.2335811040131,-3.02478230262524));
#49441=CARTESIAN_POINT('Ctrl Pts',(-30.6265238814079,1.26326461490713,-3.59637374923839));
#49442=CARTESIAN_POINT('Ctrl Pts',(-30.4276503497104,3.70847838266379,-0.881436167174301));
#49443=CARTESIAN_POINT('Ctrl Pts',(-30.228776818013,2.74633459791199,2.64336677511825));
#49444=CARTESIAN_POINT('Ctrl Pts',(-30.0299032863155,-0.739147054374844,
3.73943889687965));
#49445=CARTESIAN_POINT('Ctrl Pts',(-29.8723865305536,-2.96190354995556,
1.88626621384466));
#49446=CARTESIAN_POINT('Ctrl Pts',(-29.7811609520241,-3.22102779006444,
0.407094348824174));
#49447=CARTESIAN_POINT('Ctrl Pts',(-29.7562265507271,-3.21871773150106,
0.00201865740826774));
#49448=CARTESIAN_POINT('Origin',(-111.877773449273,0.,0.));
#49449=CARTESIAN_POINT('',(-32.5027734492733,-3.21740710269033,-6.57967736794519E-5));
#49450=CARTESIAN_POINT('',(-32.256226550727,-3.22399452161269,-0.00285325182603574));
#49451=CARTESIAN_POINT('',(-111.877773449273,-3.22275,5.46201577318104E-12));
#49452=CARTESIAN_POINT('Ctrl Pts',(-32.5027734492733,-3.21740710269033,
-6.57967736795301E-5));
#49453=CARTESIAN_POINT('Ctrl Pts',(-32.4698721999782,-3.21750414203768,
-0.535112472795859));
#49454=CARTESIAN_POINT('Ctrl Pts',(-32.3706797734506,-2.83733373420474,
-2.14806978347254));
#49455=CARTESIAN_POINT('Ctrl Pts',(-32.2051961696905,-0.285653447597213,
-3.80107139361567));
#49456=CARTESIAN_POINT('Ctrl Pts',(-32.0063226379931,3.04334298908304,-2.29516994627558));
#49457=CARTESIAN_POINT('Ctrl Pts',(-31.8074491062956,3.57610963858108,1.31953836031194));
#49458=CARTESIAN_POINT('Ctrl Pts',(-31.6085755745982,0.823139409423143,
3.72185211207294));
#49459=CARTESIAN_POINT('Ctrl Pts',(-31.423683688924,-2.43941638392043,2.77604319386724));
#49460=CARTESIAN_POINT('Ctrl Pts',(-31.3050829804824,-3.21559205689173,
0.843709427971166));
#49461=CARTESIAN_POINT('Ctrl Pts',(-31.2527734492733,-3.22346295616709,
-0.00292610916508954));
#49462=CARTESIAN_POINT('Ctrl Pts',(-32.256226550727,-3.22399452161269,-0.00285325182603602));
#49463=CARTESIAN_POINT('Ctrl Pts',(-32.2433217454805,-3.22592118045966,
-0.211630441180156));
#49464=CARTESIAN_POINT('Ctrl Pts',(-32.1641257630016,-3.11216840772355,
-1.49079233067677));
#49465=CARTESIAN_POINT('Ctrl Pts',(-32.0186386032901,-1.40164653229475,
-3.54473251882192));
#49466=CARTESIAN_POINT('Ctrl Pts',(-31.8197650715926,2.22438539621574,-3.09545654800542));
#49467=CARTESIAN_POINT('Ctrl Pts',(-31.6208915398952,3.8066474554137,0.1979312549345));
#49468=CARTESIAN_POINT('Ctrl Pts',(-31.4220180081977,1.89135401649272,3.30945941443378));
#49469=CARTESIAN_POINT('Ctrl Pts',(-31.2231444765003,-1.7617193762471,3.38024946872905));
#49470=CARTESIAN_POINT('Ctrl Pts',(-31.08454732401,-3.1795165237794,1.26513147465124));
#49471=CARTESIAN_POINT('Ctrl Pts',(-31.0122413487523,-3.22759124914724,
0.0987764919080167));
#49472=CARTESIAN_POINT('Ctrl Pts',(-31.0062265507271,-3.22697096224228,
0.00170102469852487));
#49473=CARTESIAN_POINT('Origin',(-111.877773449273,0.,0.));
#49474=CARTESIAN_POINT('',(-33.7527734492733,-3.22322064294668,0.00294899761280168));
#49475=CARTESIAN_POINT('',(-33.506226550727,-3.21744102079098,-0.000354983176735213));
#49476=CARTESIAN_POINT('',(-111.877773449273,-3.22275,5.46201577318104E-12));
#49477=CARTESIAN_POINT('Ctrl Pts',(-33.7527734492733,-3.22322064294668,
0.00294899761280141));
#49478=CARTESIAN_POINT('Ctrl Pts',(-33.7009525967064,-3.21542081039077,
-0.83593893015554));
#49479=CARTESIAN_POINT('Ctrl Pts',(-33.5828405669071,-2.45120246003302,
-2.76055497526885));
#49480=CARTESIAN_POINT('Ctrl Pts',(-33.3984373598752,0.795690606434006,
-3.72781679945786));
#49481=CARTESIAN_POINT('Ctrl Pts',(-33.1995638281778,3.56628881859093,-1.34585500477608));
#49482=CARTESIAN_POINT('Ctrl Pts',(-33.0006902964803,3.06017354166348,2.27268113170112));
#49483=CARTESIAN_POINT('Ctrl Pts',(-32.8018167647829,-0.257635468714778,
3.8030731779375));
#49484=CARTESIAN_POINT('Ctrl Pts',(-32.6358444823805,-2.82899846132347,
2.16409415778827));
#49485=CARTESIAN_POINT('Ctrl Pts',(-32.5361633772107,-3.21730862202821,
0.542927868763348));
#49486=CARTESIAN_POINT('Ctrl Pts',(-32.5027734492733,-3.21740710269033,
-6.57967736795301E-5));
#49487=CARTESIAN_POINT('Ctrl Pts',(-33.506226550727,-3.21744102079098,-0.000354983176735595));
#49488=CARTESIAN_POINT('Ctrl Pts',(-33.4744021422088,-3.21794772146192,
-0.517876261114896));
#49489=CARTESIAN_POINT('Ctrl Pts',(-33.376286556458,-2.85541175867603,-2.11273958371276));
#49490=CARTESIAN_POINT('Ctrl Pts',(-33.2118797934747,-0.347336302469681,
-3.79593191778697));
#49491=CARTESIAN_POINT('Ctrl Pts',(-33.0130062617774,3.005673560666,-2.34428412915341));
#49492=CARTESIAN_POINT('Ctrl Pts',(-32.8141327300798,3.59706438479482,1.26129673080056));
#49493=CARTESIAN_POINT('Ctrl Pts',(-32.6152591983825,0.883465066420513,
3.70799556470907));
#49494=CARTESIAN_POINT('Ctrl Pts',(-32.4292904719315,-2.41310692203674,
2.81008834410801));
#49495=CARTESIAN_POINT('Ctrl Pts',(-32.309612922713,-3.21602405449369,0.860844919524442));
#49496=CARTESIAN_POINT('Ctrl Pts',(-32.256226550727,-3.22399452161269,-0.00285325182603602));
#49497=CARTESIAN_POINT('Origin',(-111.877773449273,0.,0.));
#49498=CARTESIAN_POINT('',(-35.0027734492733,-3.22744352734777,-0.00129919044773077));
#49499=CARTESIAN_POINT('',(-34.756226550727,-3.22268735527833,0.00297700638213272));
#49500=CARTESIAN_POINT('',(-111.877773449273,-3.22275,5.46201577318104E-12));
#49501=CARTESIAN_POINT('Ctrl Pts',(-35.0027734492733,-3.22744352734777,
-0.0012991904477314));
#49502=CARTESIAN_POINT('Ctrl Pts',(-34.9983241706672,-3.22780977286361,
-0.0730802400329829));
#49503=CARTESIAN_POINT('Ctrl Pts',(-34.9275837148285,-3.19304810227478,
-1.2139881808383));
#49504=CARTESIAN_POINT('Ctrl Pts',(-34.7905520817575,-1.84102023303062,
-3.33772169796395));
#49505=CARTESIAN_POINT('Ctrl Pts',(-34.5916785500599,1.81270627375333,-3.35318320355194));
#49506=CARTESIAN_POINT('Ctrl Pts',(-34.3928050183625,3.80091453423265,-0.287733096717287));
#49507=CARTESIAN_POINT('Ctrl Pts',(-34.193931486665,2.29683471634544,3.04208677017568));
#49508=CARTESIAN_POINT('Ctrl Pts',(-33.9950579549676,-1.3175815549477,3.5768310663979));
#49509=CARTESIAN_POINT('Ctrl Pts',(-33.848005275837,-3.09503335659972,1.54217969858807));
#49510=CARTESIAN_POINT('Ctrl Pts',(-33.7672437739389,-3.22539864859171,
0.237197954771449));
#49511=CARTESIAN_POINT('Ctrl Pts',(-33.7527734492733,-3.22322064294668,
0.00294899761280141));
#49512=CARTESIAN_POINT('Ctrl Pts',(-34.756226550727,-3.22268735527833,0.00297700638213272));
#49513=CARTESIAN_POINT('Ctrl Pts',(-34.705482538937,-3.21509624485328,-0.818826640955584));
#49514=CARTESIAN_POINT('Ctrl Pts',(-34.5884473499145,-2.47683791878395,
-2.72634477769257));
#49515=CARTESIAN_POINT('Ctrl Pts',(-34.4051209836595,0.735054671056124,
-3.74024548152205));
#49516=CARTESIAN_POINT('Ctrl Pts',(-34.206247451962,3.54396510108007,-1.40358576289945));
#49517=CARTESIAN_POINT('Ctrl Pts',(-34.0073739202646,3.09667311950531,2.22269143661931));
#49518=CARTESIAN_POINT('Ctrl Pts',(-33.8085003885672,-0.195848482584929,
3.80675518038088));
#49519=CARTESIAN_POINT('Ctrl Pts',(-33.6414512653879,-2.8103393237568,2.19938364520229));
#49520=CARTESIAN_POINT('Ctrl Pts',(-33.5406933194413,-3.21689224908883,
0.560135754024039));
#49521=CARTESIAN_POINT('Ctrl Pts',(-33.506226550727,-3.21744102079098,-0.000354983176735595));
#49522=CARTESIAN_POINT('Origin',(-111.877773449273,0.,0.));
#49523=CARTESIAN_POINT('',(-36.2527734492733,-3.21923858670683,-0.00231041055963243));
#49524=CARTESIAN_POINT('',(-36.006226550727,-3.22770167512206,-0.00100144746363884));
#49525=CARTESIAN_POINT('',(-111.877773449273,-3.22275,5.46201577318104E-12));
#49526=CARTESIAN_POINT('Ctrl Pts',(-36.2527734492733,-3.21923858670683,
-0.00231041055963242));
#49527=CARTESIAN_POINT('Ctrl Pts',(-36.2294045673954,-3.22174153913682,
-0.381799118952256));
#49528=CARTESIAN_POINT('Ctrl Pts',(-36.139744508285,-2.98395358934763,-1.83475860293934));
#49529=CARTESIAN_POINT('Ctrl Pts',(-35.9837932719421,-0.827211612766053,
-3.72094915030997));
#49530=CARTESIAN_POINT('Ctrl Pts',(-35.7849197402446,2.68317192624198,-2.70745822603308));
#49531=CARTESIAN_POINT('Ctrl Pts',(-35.5860462085473,3.72825159013562,0.793650875472599));
#49532=CARTESIAN_POINT('Ctrl Pts',(-35.3871726768497,1.34780603789606,3.56555192301254));
#49533=CARTESIAN_POINT('Ctrl Pts',(-35.1927484237585,-2.19004494105729,
3.07269526205072));
#49534=CARTESIAN_POINT('Ctrl Pts',(-35.0646153478996,-3.22235296771607,
0.99640780537872));
#49535=CARTESIAN_POINT('Ctrl Pts',(-35.0027734492733,-3.22744352734777,
-0.0012991904477314));
#49536=CARTESIAN_POINT('Ctrl Pts',(-36.006226550727,-3.22770167512206,-0.001001447463639));
#49537=CARTESIAN_POINT('Ctrl Pts',(-36.0028541128977,-3.22792288376692,
-0.0553980490410728));
#49538=CARTESIAN_POINT('Ctrl Pts',(-35.9331904978359,-3.2019871633926,-1.17883982497487));
#49539=CARTESIAN_POINT('Ctrl Pts',(-35.7972357055417,-1.89497431298474,
-3.30738778866578));
#49540=CARTESIAN_POINT('Ctrl Pts',(-35.5983621738442,1.75801942947801,-3.3821752345296));
#49541=CARTESIAN_POINT('Ctrl Pts',(-35.3994886421468,3.79574131044322,-0.34941313038003));
#49542=CARTESIAN_POINT('Ctrl Pts',(-35.2006151104493,2.34592828168183,3.00439047540306));
#49543=CARTESIAN_POINT('Ctrl Pts',(-35.0017415787519,-1.25932846911898,
3.59775394355339));
#49544=CARTESIAN_POINT('Ctrl Pts',(-34.8536120588444,-3.08284009568445,
1.57754640695969));
#49545=CARTESIAN_POINT('Ctrl Pts',(-34.7717737161695,-3.22501315187002,
0.254764691582217));
#49546=CARTESIAN_POINT('Ctrl Pts',(-34.756226550727,-3.22268735527833,0.00297700638213272));
#49547=CARTESIAN_POINT('Origin',(-111.877773449273,0.,0.));
#49548=CARTESIAN_POINT('',(-37.5027734492733,-3.219018731458,0.00219753035672858));
#49549=CARTESIAN_POINT('',(-37.256226550727,-3.21963831861728,-0.00248457511186462));
#49550=CARTESIAN_POINT('',(-111.877773449273,-3.22275,5.46201577318104E-12));
#49551=CARTESIAN_POINT('Ctrl Pts',(-37.5027734492733,-3.219018731458,0.00219753035672829));
#49552=CARTESIAN_POINT('Ctrl Pts',(-37.4604849641236,-3.21472912215605,
-0.684645539904419));
#49553=CARTESIAN_POINT('Ctrl Pts',(-37.3519053017415,-2.66242384752364,
-2.45447718507084));
#49554=CARTESIAN_POINT('Ctrl Pts',(-37.1770344621268,0.253473740852287,
-3.80335282273231));
#49555=CARTESIAN_POINT('Ctrl Pts',(-36.9781609304294,3.33671391532343,-1.84284613540428));
#49556=CARTESIAN_POINT('Ctrl Pts',(-36.7792873987319,3.35417449321223,1.81087136499863));
#49557=CARTESIAN_POINT('Ctrl Pts',(-36.5804138670345,0.289812659703135,
3.80075653702829));
#49558=CARTESIAN_POINT('Ctrl Pts',(-36.404909217215,-2.64945837149216,2.47502346421667));
#49559=CARTESIAN_POINT('Ctrl Pts',(-36.2956957446279,-3.21464134221648,
0.694707380468959));
#49560=CARTESIAN_POINT('Ctrl Pts',(-36.2527734492733,-3.21923858670683,
-0.00231041055963242));
#49561=CARTESIAN_POINT('Ctrl Pts',(-37.256226550727,-3.21963831861728,-0.00248457511186476));
#49562=CARTESIAN_POINT('Ctrl Pts',(-37.233934509626,-3.22222657760521,-0.364373415634379));
#49563=CARTESIAN_POINT('Ctrl Pts',(-37.1453512912924,-2.99867355361791,
-1.7993284911519));
#49564=CARTESIAN_POINT('Ctrl Pts',(-36.9904768957264,-0.887522070897608,
-3.70702659892766));
#49565=CARTESIAN_POINT('Ctrl Pts',(-36.7916033640289,2.63885538457792,-2.75066971677293));
#49566=CARTESIAN_POINT('Ctrl Pts',(-36.5927298323315,3.74064709441386,0.733008149027457));
#49567=CARTESIAN_POINT('Ctrl Pts',(-36.393856300634,1.40552457333426,3.54319662243588));
#49568=CARTESIAN_POINT('Ctrl Pts',(-36.1983552067659,-2.15949934739163,
3.10544016138809));
#49569=CARTESIAN_POINT('Ctrl Pts',(-36.0691452901302,-3.22357464008568,
1.01386250920722));
#49570=CARTESIAN_POINT('Ctrl Pts',(-36.006226550727,-3.22770167512206,-0.001001447463639));
#49571=CARTESIAN_POINT('Origin',(-111.877773449273,0.,0.));
#49572=CARTESIAN_POINT('',(-38.7527734492733,-3.22726520035117,0.00146672624921877));
#49573=CARTESIAN_POINT('',(-38.506226550727,-3.21867331583696,0.00198948205692828));
#49574=CARTESIAN_POINT('',(-111.877773449273,-3.22275,5.46201577318104E-12));
#49575=CARTESIAN_POINT('Ctrl Pts',(-38.7527734492733,-3.22726520035117,
0.00146672624921861));
#49576=CARTESIAN_POINT('Ctrl Pts',(-38.6915653608519,-3.22168090845198,
-0.986159528139468));
#49577=CARTESIAN_POINT('Ctrl Pts',(-38.564066095198,-2.20779488141114,-3.05334042855296));
#49578=CARTESIAN_POINT('Ctrl Pts',(-38.3702756523116,1.31366676153256,-3.57827070959312));
#49579=CARTESIAN_POINT('Ctrl Pts',(-38.1714021206141,3.7204959985358,-0.829247343297895));
#49580=CARTESIAN_POINT('Ctrl Pts',(-37.9725285889167,2.70892587289195,2.68169018469027));
#49581=CARTESIAN_POINT('Ctrl Pts',(-37.7736550572192,-0.791610906928228,
3.7286852647441));
#49582=CARTESIAN_POINT('Ctrl Pts',(-37.6170700106714,-2.97511982063936,
1.85561225222715));
#49583=CARTESIAN_POINT('Ctrl Pts',(-37.5267761413561,-3.22145348812676,
0.392045562660032));
#49584=CARTESIAN_POINT('Ctrl Pts',(-37.5027734492733,-3.219018731458,0.00219753035672829));
#49585=CARTESIAN_POINT('Ctrl Pts',(-38.506226550727,-3.21867331583696,0.00198948205692842));
#49586=CARTESIAN_POINT('Ctrl Pts',(-38.4650149063542,-3.21491357698761,
-0.667543843238478));
#49587=CARTESIAN_POINT('Ctrl Pts',(-38.3575120847489,-2.68410918284495,
-2.419518782989));
#49588=CARTESIAN_POINT('Ctrl Pts',(-38.1837180859111,0.191682762624847,
-3.80696721157406));
#49589=CARTESIAN_POINT('Ctrl Pts',(-37.9848445542137,3.30635049050394,-1.89678361059766));
#49590=CARTESIAN_POINT('Ctrl Pts',(-37.7859710225162,3.38313659886923,1.75616866640966));
#49591=CARTESIAN_POINT('Ctrl Pts',(-37.5870974908188,0.351489853691939,
3.79554956682676));
#49592=CARTESIAN_POINT('Ctrl Pts',(-37.4105160002224,-2.62708460916839,
2.50987780220601));
#49593=CARTESIAN_POINT('Ctrl Pts',(-37.3002256868585,-3.21452971689538,
0.711797095481222));
#49594=CARTESIAN_POINT('Ctrl Pts',(-37.256226550727,-3.21963831861728,-0.00248457511186476));
#49595=CARTESIAN_POINT('Origin',(-111.877773449273,0.,0.));
#49596=CARTESIAN_POINT('',(-40.0027734492733,-3.22353484965401,-0.00291808672030292));
#49597=CARTESIAN_POINT('',(-39.756226550727,-3.22692192365936,0.00173613518965589));
#49598=CARTESIAN_POINT('',(-111.877773449273,-3.22275,5.46201577318104E-12));
#49599=CARTESIAN_POINT('Ctrl Pts',(-40.0027734492733,-3.22353484965401,
-0.00291808672030294));
#49600=CARTESIAN_POINT('Ctrl Pts',(-39.9889369348126,-3.22561581060293,
-0.226850780479683));
#49601=CARTESIAN_POINT('Ctrl Pts',(-39.9088092431194,-3.10205454560406,
-1.52137086821301));
#49602=CARTESIAN_POINT('Ctrl Pts',(-39.7623903741938,-1.35170689313597,
-3.56407492998341));
#49603=CARTESIAN_POINT('Ctrl Pts',(-39.5635168424963,2.2676551057174,-3.06389979486944));
#49604=CARTESIAN_POINT('Ctrl Pts',(-39.3646433107988,3.80349093732365,0.251392762791839));
#49605=CARTESIAN_POINT('Ctrl Pts',(-39.1657697791013,1.84467148611344,3.33570513382216));
#49606=CARTESIAN_POINT('Ctrl Pts',(-38.966896247404,-1.80903591415121,3.35516477878489));
#49607=CARTESIAN_POINT('Ctrl Pts',(-38.8292308041279,-3.18764669610349,
1.23468759585245));
#49608=CARTESIAN_POINT('Ctrl Pts',(-38.7578565380844,-3.22772895362958,
0.0834851668289423));
#49609=CARTESIAN_POINT('Ctrl Pts',(-38.7527734492733,-3.22726520035117,
0.00146672624921861));
#49610=CARTESIAN_POINT('Ctrl Pts',(-39.756226550727,-3.22692192365936,0.00173613518965601));
#49611=CARTESIAN_POINT('Ctrl Pts',(-39.6960953030824,-3.22061713569807,
-0.968787371651353));
#49612=CARTESIAN_POINT('Ctrl Pts',(-39.5696728782054,-2.23756505773814,
-3.02032269454104));
#49613=CARTESIAN_POINT('Ctrl Pts',(-39.3769592760958,1.25539081538779,-3.59912982985154));
#49614=CARTESIAN_POINT('Ctrl Pts',(-39.1780857443985,3.70654045139103,-0.889550174914005));
#49615=CARTESIAN_POINT('Ctrl Pts',(-38.9792122127009,2.75211311011837,2.63735000722356));
#49616=CARTESIAN_POINT('Ctrl Pts',(-38.7803386810035,-0.73096140756941,
3.74104758752567));
#49617=CARTESIAN_POINT('Ctrl Pts',(-38.6226767936788,-2.95982002325488,
1.89104093761493));
#49618=CARTESIAN_POINT('Ctrl Pts',(-38.5313060835867,-3.22096132194424,
0.409437019954045));
#49619=CARTESIAN_POINT('Ctrl Pts',(-38.506226550727,-3.21867331583696,0.00198948205692842));
#49620=CARTESIAN_POINT('Origin',(-111.877773449273,0.,0.));
#49621=CARTESIAN_POINT('',(-41.2527734492733,-3.2174089549063,-0.000104865731855516));
#49622=CARTESIAN_POINT('',(-41.006226550727,-3.22406569797495,-0.00284108206035388));
#49623=CARTESIAN_POINT('',(-111.877773449273,-3.22275,5.46201577318104E-12));
#49624=CARTESIAN_POINT('Ctrl Pts',(-41.2527734492733,-3.21740895490631,
-0.000104865731855551));
#49625=CARTESIAN_POINT('Ctrl Pts',(-41.2200173315409,-3.21756293715421,
-0.532790619038696));
#49626=CARTESIAN_POINT('Ctrl Pts',(-41.1209700365759,-2.83979337265085,
-2.14330964829616));
#49627=CARTESIAN_POINT('Ctrl Pts',(-40.9556315643784,-0.293971524782049,
-3.8004371293451));
#49628=CARTESIAN_POINT('Ctrl Pts',(-40.7567580326811,3.03831265098276,-2.30182489915407));
#49629=CARTESIAN_POINT('Ctrl Pts',(-40.5578845009835,3.57898892454058,1.31170877465366));
#49630=CARTESIAN_POINT('Ctrl Pts',(-40.3590109692861,0.831282825590706,
3.72004173301395));
#49631=CARTESIAN_POINT('Ctrl Pts',(-40.1739739520493,-2.43589766006429,
2.78063847357564));
#49632=CARTESIAN_POINT('Ctrl Pts',(-40.0552281120451,-3.215645861056,0.846017818929096));
#49633=CARTESIAN_POINT('Ctrl Pts',(-40.0027734492733,-3.22353484965401,
-0.00291808672030294));
#49634=CARTESIAN_POINT('Ctrl Pts',(-41.006226550727,-3.22406569797495,-0.00284108206035385));
#49635=CARTESIAN_POINT('Ctrl Pts',(-40.9934668770432,-3.22596721187625,
-0.209258560572843));
#49636=CARTESIAN_POINT('Ctrl Pts',(-40.9144160261268,-3.11372174647206,
-1.48603033395852));
#49637=CARTESIAN_POINT('Ctrl Pts',(-40.7690739979781,-1.40940093137277,
-3.54165648336101));
#49638=CARTESIAN_POINT('Ctrl Pts',(-40.5702004662805,2.21760556762163,-3.10031727052911));
#49639=CARTESIAN_POINT('Ctrl Pts',(-40.3713269345832,3.80707151773659,0.189599816261364));
#49640=CARTESIAN_POINT('Ctrl Pts',(-40.1724534028856,1.89859234039963,3.30531220257079));
#49641=CARTESIAN_POINT('Ctrl Pts',(-39.9735798711882,-1.75431737762409,
3.38409695045128));
#49642=CARTESIAN_POINT('Ctrl Pts',(-39.8348375871353,-3.17822961575262,
1.2698753297387));
#49643=CARTESIAN_POINT('Ctrl Pts',(-39.7623864803149,-3.22756779500628,
0.101157928346097));
#49644=CARTESIAN_POINT('Ctrl Pts',(-39.756226550727,-3.22692192365936,0.00173613518965601));
#49645=CARTESIAN_POINT('Origin',(-111.877773449273,0.,0.));
#49646=CARTESIAN_POINT('',(-42.5027734492733,-3.22314865752612,0.00295457023921248));
#49647=CARTESIAN_POINT('',(-42.256226550727,-3.21744915169808,-0.000393767763913477));
#49648=CARTESIAN_POINT('',(-111.877773449273,-3.22275,5.46201577318104E-12));
#49649=CARTESIAN_POINT('Ctrl Pts',(-42.5027734492733,-3.22314865752612,
0.00295457023921235));
#49650=CARTESIAN_POINT('Ctrl Pts',(-42.4510977282691,-3.21537286851395,
-0.833631803745193));
#49651=CARTESIAN_POINT('Ctrl Pts',(-42.3331308300324,-2.45468440648667,
-2.75595069101997));
#49652=CARTESIAN_POINT('Ctrl Pts',(-42.1488727545632,0.787530259532762,
-3.72954926523403));
#49653=CARTESIAN_POINT('Ctrl Pts',(-41.9499992228658,3.56333483297472,-1.35365671408838));
#49654=CARTESIAN_POINT('Ctrl Pts',(-41.7511256911682,3.06514004538181,2.2659784053879));
#49655=CARTESIAN_POINT('Ctrl Pts',(-41.5522521594708,-0.249311709475826,
3.80362791332241));
#49656=CARTESIAN_POINT('Ctrl Pts',(-41.3861347455058,-2.82650711453577,
2.16885207273882));
#49657=CARTESIAN_POINT('Ctrl Pts',(-41.2863085087734,-3.21725131095449,
0.545248175732359));
#49658=CARTESIAN_POINT('Ctrl Pts',(-41.2527734492733,-3.21740895490631,
-0.000104865731855551));
#49659=CARTESIAN_POINT('Ctrl Pts',(-42.256226550727,-3.21744915169808,-0.000393767763913581));
#49660=CARTESIAN_POINT('Ctrl Pts',(-42.2245472737714,-3.21800872812467,
-0.515551704072911));
#49661=CARTESIAN_POINT('Ctrl Pts',(-42.1265768195833,-2.85781794654228,
-2.10797606309353));
#49662=CARTESIAN_POINT('Ctrl Pts',(-41.9623151881627,-0.355642984033713,
-3.7951626710057));
#49663=CARTESIAN_POINT('Ctrl Pts',(-41.7634416564653,3.00053582488292,-2.35085652371245));
#49664=CARTESIAN_POINT('Ctrl Pts',(-41.5645681247678,3.59981615697931,1.2534214245169));
#49665=CARTESIAN_POINT('Ctrl Pts',(-41.3656945930704,0.891578012639441,
3.70605319428438));
#49666=CARTESIAN_POINT('Ctrl Pts',(-41.1795807350568,-2.40952537855057,
2.81466767056952));
#49667=CARTESIAN_POINT('Ctrl Pts',(-41.0597580542757,-3.21608815084661,
0.863155827992277));
#49668=CARTESIAN_POINT('Ctrl Pts',(-41.006226550727,-3.22406569797495,-0.00284108206035385));
#49669=CARTESIAN_POINT('Origin',(-111.877773449273,0.,0.));
#49670=CARTESIAN_POINT('',(-43.7527734492733,-3.22748170351345,-0.00125997746166298));
#49671=CARTESIAN_POINT('',(-43.506226550727,-3.22261575386789,0.00297842904322623));
#49672=CARTESIAN_POINT('',(-111.877773449273,-3.22275,5.46201577318104E-12));
#49673=CARTESIAN_POINT('Ctrl Pts',(-43.7527734492733,-3.22748170351345,
-0.00125997746166296));
#49674=CARTESIAN_POINT('Ctrl Pts',(-43.7484693022298,-3.22782680043517,
-0.0706974116263659));
#49675=CARTESIAN_POINT('Ctrl Pts',(-43.6778739779538,-3.19427028568405,
-1.20924958558968));
#49676=CARTESIAN_POINT('Ctrl Pts',(-43.5409874764454,-1.84832053035247,
-3.33368457544577));
#49677=CARTESIAN_POINT('Ctrl Pts',(-43.3421139447478,1.80536338837631,-3.35714233648167));
#49678=CARTESIAN_POINT('Ctrl Pts',(-43.1432404130505,3.80027571896185,-0.296050825630079));
#49679=CARTESIAN_POINT('Ctrl Pts',(-42.944366881353,2.30348691596348,3.03705279168351));
#49680=CARTESIAN_POINT('Ctrl Pts',(-42.7454933496556,-1.30975039510868,
3.57970606810114));
#49681=CARTESIAN_POINT('Ctrl Pts',(-42.5982955389623,-3.09340945840058,
1.54694535430405));
#49682=CARTESIAN_POINT('Ctrl Pts',(-42.5173889055015,-3.22534788574663,
0.239566489580112));
#49683=CARTESIAN_POINT('Ctrl Pts',(-42.5027734492733,-3.22314865752612,
0.00295457023921235));
#49684=CARTESIAN_POINT('Ctrl Pts',(-43.506226550727,-3.22261575386789,0.00297842904322623));
#49685=CARTESIAN_POINT('Ctrl Pts',(-43.4556276704997,-3.21505792776503,
-0.816521309002297));
#49686=CARTESIAN_POINT('Ctrl Pts',(-43.3387376130398,-2.48025772245358,
-2.72172583709136));
#49687=CARTESIAN_POINT('Ctrl Pts',(-43.1555563783475,0.726867268816058,
-3.74184521393008));
#49688=CARTESIAN_POINT('Ctrl Pts',(-42.95668284665,3.54088482339137,-1.41133847781607));
#49689=CARTESIAN_POINT('Ctrl Pts',(-42.7578093149525,3.10153013183299,2.21590894957792));
#49690=CARTESIAN_POINT('Ctrl Pts',(-42.5589357832551,-0.187516813140302,
3.80717468423465));
#49691=CARTESIAN_POINT('Ctrl Pts',(-42.3917415285133,-2.80779368415632,
2.20413738880447));
#49692=CARTESIAN_POINT('Ctrl Pts',(-42.2908384510039,-3.21683777399834,
0.562453520176393));
#49693=CARTESIAN_POINT('Ctrl Pts',(-42.256226550727,-3.21744915169808,-0.000393767763913581));
#49694=CARTESIAN_POINT('Origin',(-111.877773449273,0.,0.));
#49695=CARTESIAN_POINT('',(-45.0027734492733,-3.21929057874326,-0.00233520374894584));
#49696=CARTESIAN_POINT('',(-44.756226550727,-3.22773185798094,-0.000960206790133755));
#49697=CARTESIAN_POINT('',(-111.877773449273,-3.22275,5.46201577318104E-12));
#49698=CARTESIAN_POINT('Ctrl Pts',(-45.0027734492733,-3.21929057874326,
-0.0023352037489462));
#49699=CARTESIAN_POINT('Ctrl Pts',(-44.979549698958,-3.22180726243893,-0.379451811020904));
#49700=CARTESIAN_POINT('Ctrl Pts',(-44.8900347714103,-2.98595860481547,
-1.8299834528453));
#49701=CARTESIAN_POINT('Ctrl Pts',(-44.7342286666301,-0.835353043022,-3.7191298612715));
#49702=CARTESIAN_POINT('Ctrl Pts',(-44.5353551349326,2.67724014515226,-2.71332394613555));
#49703=CARTESIAN_POINT('Ctrl Pts',(-44.3364816032351,3.72997959085687,0.785489581903391));
#49704=CARTESIAN_POINT('Ctrl Pts',(-44.1376080715378,1.35560612981737,3.56259366926528));
#49705=CARTESIAN_POINT('Ctrl Pts',(-43.9430386868837,-2.18595670130309,
3.07711876257639));
#49706=CARTESIAN_POINT('Ctrl Pts',(-43.8147604794623,-3.22251172151965,
0.998757048983725));
#49707=CARTESIAN_POINT('Ctrl Pts',(-43.7527734492733,-3.22748170351345,
-0.00125997746166296));
#49708=CARTESIAN_POINT('Ctrl Pts',(-44.756226550727,-3.22773185798094,-0.000960206790134015));
#49709=CARTESIAN_POINT('Ctrl Pts',(-44.7529992444603,-3.2279357792308,-0.0530145735234573));
#49710=CARTESIAN_POINT('Ctrl Pts',(-44.6834807609612,-3.2031691639196,-1.17410462500792));
#49711=CARTESIAN_POINT('Ctrl Pts',(-44.5476711002297,-1.90220809440512,
-3.30323265863413));
#49712=CARTESIAN_POINT('Ctrl Pts',(-44.3487975685321,1.75061322511827,-3.386014614193));
#49713=CARTESIAN_POINT('Ctrl Pts',(-44.1499240368348,3.79496751891687,-0.357719389820383));
#49714=CARTESIAN_POINT('Ctrl Pts',(-43.9510505051372,2.35249786423195,2.99924914441454));
#49715=CARTESIAN_POINT('Ctrl Pts',(-43.7521769734399,-1.2514516584285,3.60050140648546));
#49716=CARTESIAN_POINT('Ctrl Pts',(-43.6039023219698,-3.08117113765723,
1.58231411279105));
#49717=CARTESIAN_POINT('Ctrl Pts',(-43.5219188477322,-3.22495967237728,
0.257130956278012));
#49718=CARTESIAN_POINT('Ctrl Pts',(-43.506226550727,-3.22261575386789,0.00297842904322623));
#49719=CARTESIAN_POINT('Origin',(-111.877773449273,0.,0.));
#49720=CARTESIAN_POINT('',(-46.2527734492733,-3.21897007644484,0.00217065586278493));
#49721=CARTESIAN_POINT('',(-46.006226550727,-3.21969458294954,-0.00250627002517184));
#49722=CARTESIAN_POINT('',(-111.877773449273,-3.22275,5.46201577318104E-12));
#49723=CARTESIAN_POINT('Ctrl Pts',(-46.2527734492733,-3.21897007644484,
0.0021706558627849));
#49724=CARTESIAN_POINT('Ctrl Pts',(-46.2106300956863,-3.21475143459506,
-0.682341170182447));
#49725=CARTESIAN_POINT('Ctrl Pts',(-46.1021955648668,-2.66537161816311,
-2.44976928448922));
#49726=CARTESIAN_POINT('Ctrl Pts',(-45.9274698568148,0.245149379568856,
-3.80389844937855));
#49727=CARTESIAN_POINT('Ctrl Pts',(-45.7285963251173,3.33267279917539,-1.8501442227902));
#49728=CARTESIAN_POINT('Ctrl Pts',(-45.5297227934199,3.35812960801393,1.80352631454818));
#49729=CARTESIAN_POINT('Ctrl Pts',(-45.3308492617224,0.298130037853896,
3.80011317094853));
#49730=CARTESIAN_POINT('Ctrl Pts',(-45.1551994803403,-2.64646835176648,
2.47972498007439));
#49731=CARTESIAN_POINT('Ctrl Pts',(-45.0458408761905,-3.21462349915166,
0.697011013054861));
#49732=CARTESIAN_POINT('Ctrl Pts',(-45.0027734492733,-3.21929057874326,
-0.0023352037489462));
#49733=CARTESIAN_POINT('Ctrl Pts',(-46.006226550727,-3.21969458294954,-0.0025062700251724));
#49734=CARTESIAN_POINT('Ctrl Pts',(-45.9840796411886,-3.22229142974673,
-0.362023233856792));
#49735=CARTESIAN_POINT('Ctrl Pts',(-45.8956415544178,-3.00062983176092,
-1.79455350713736));
#49736=CARTESIAN_POINT('Ctrl Pts',(-45.7409122904144,-0.895632886789359,
-3.7050753519448));
#49737=CARTESIAN_POINT('Ctrl Pts',(-45.5420387587169,2.63282913994673,-2.7564383452809));
#49738=CARTESIAN_POINT('Ctrl Pts',(-45.3431652270195,3.74224234698389,0.724819872746352));
#49739=CARTESIAN_POINT('Ctrl Pts',(-45.144291695322,1.41327560176868,3.54011210344149));
#49740=CARTESIAN_POINT('Ctrl Pts',(-44.9486454698912,-2.15534504929802,
3.10983967618609));
#49741=CARTESIAN_POINT('Ctrl Pts',(-44.8192904216928,-3.22374709101849,
1.01621932179185));
#49742=CARTESIAN_POINT('Ctrl Pts',(-44.756226550727,-3.22773185798094,-0.000960206790134015));
#49743=CARTESIAN_POINT('Origin',(-111.877773449273,0.,0.));
#49744=CARTESIAN_POINT('',(-47.5027734492733,-3.22722180108715,0.00150419546486083));
#49745=CARTESIAN_POINT('',(-47.256226550727,-3.21862958324598,0.00195996754723593));
#49746=CARTESIAN_POINT('',(-111.877773449273,-3.22275,5.46201577318104E-12));
#49747=CARTESIAN_POINT('Ctrl Pts',(-47.5027734492733,-3.22722180108715,
0.00150419546486084));
#49748=CARTESIAN_POINT('Ctrl Pts',(-47.4417104924145,-3.2215318458885,-0.983815348456214));
#49749=CARTESIAN_POINT('Ctrl Pts',(-47.3143563583233,-2.21183553277418,
-3.04890018572942));
#49750=CARTESIAN_POINT('Ctrl Pts',(-47.1207110469995,1.30583246036561,-3.5811371402032));
#49751=CARTESIAN_POINT('Ctrl Pts',(-46.9218375153022,3.71867225532388,-0.837387776942048));
#49752=CARTESIAN_POINT('Ctrl Pts',(-46.7229639836046,2.71478834664286,2.67575519515887));
#49753=CARTESIAN_POINT('Ctrl Pts',(-46.5240904519072,-0.783448669134082,
3.73040879989306));
#49754=CARTESIAN_POINT('Ctrl Pts',(-46.3673602737967,-2.97307922116837,
1.86038731633198));
#49755=CARTESIAN_POINT('Ctrl Pts',(-46.2769212729187,-3.22138732639628,
0.394390767735412));
#49756=CARTESIAN_POINT('Ctrl Pts',(-46.2527734492733,-3.21897007644484,
0.0021706558627849));
#49757=CARTESIAN_POINT('Ctrl Pts',(-47.256226550727,-3.21862958324598,0.00195996754723593));
#49758=CARTESIAN_POINT('Ctrl Pts',(-47.2151600379169,-3.21494169678062,
-0.665238231074718));
#49759=CARTESIAN_POINT('Ctrl Pts',(-47.1078023478743,-2.68699897644198,
-2.41480261420779));
#49760=CARTESIAN_POINT('Ctrl Pts',(-46.934153480599,0.183350639119669,-3.80737759811421));
#49761=CARTESIAN_POINT('Ctrl Pts',(-46.7352799489018,3.30219140325315,-1.90401511752624));
#49762=CARTESIAN_POINT('Ctrl Pts',(-46.5364064172041,3.3869719257786,1.74876036250685));
#49763=CARTESIAN_POINT('Ctrl Pts',(-46.3375328855069,0.3597956885221,3.79477123078697));
#49764=CARTESIAN_POINT('Ctrl Pts',(-46.1608062633476,-2.6240357574013,2.51456991883394));
#49765=CARTESIAN_POINT('Ctrl Pts',(-46.0503708184211,-3.21451842507627,
0.714099948302537));
#49766=CARTESIAN_POINT('Ctrl Pts',(-46.006226550727,-3.21969458294954,-0.0025062700251724));
#49767=CARTESIAN_POINT('Origin',(-111.877773449273,0.,0.));
#49768=CARTESIAN_POINT('',(-48.7527734492733,-3.22360668808134,-0.00290950365520015));
#49769=CARTESIAN_POINT('',(-48.506226550727,-3.22687206568905,0.00177085358160415));
#49770=CARTESIAN_POINT('',(-111.877773449273,-3.22275,5.46201577318104E-12));
#49771=CARTESIAN_POINT('Ctrl Pts',(-48.7527734492733,-3.22360668808134,
-0.00290950365519946));
#49772=CARTESIAN_POINT('Ctrl Pts',(-48.7390820663752,-3.22566447975376,
-0.224480681040578));
#49773=CARTESIAN_POINT('Ctrl Pts',(-48.6590995062447,-3.10364616015319,
-1.51660682019015));
#49774=CARTESIAN_POINT('Ctrl Pts',(-48.5128257688817,-1.35950374327106,
-3.56110814263194));
#49775=CARTESIAN_POINT('Ctrl Pts',(-48.3139522371842,2.26094423642121,-3.06885529005218));
#49776=CARTESIAN_POINT('Ctrl Pts',(-48.1150787054868,3.80403200935488,0.243068104223925));
#49777=CARTESIAN_POINT('Ctrl Pts',(-47.9162051737893,1.85196736137869,3.33166002525401));
#49778=CARTESIAN_POINT('Ctrl Pts',(-47.7173316420919,-1.80168870082603,
3.35911587427456));
#49779=CARTESIAN_POINT('Ctrl Pts',(-47.5795210672532,-3.1863951775648,1.23942860890804));
#49780=CARTESIAN_POINT('Ctrl Pts',(-47.508001669647,-3.22770897598377,0.0858674162971823));
#49781=CARTESIAN_POINT('Ctrl Pts',(-47.5027734492733,-3.22722180108715,
0.00150419546486084));
#49782=CARTESIAN_POINT('Ctrl Pts',(-48.506226550727,-3.22687206568905,0.00177085358160422));
#49783=CARTESIAN_POINT('Ctrl Pts',(-48.4462404346451,-3.22048116252823,
-0.966449641389064));
#49784=CARTESIAN_POINT('Ctrl Pts',(-48.3199631413307,-2.24154020220606,
-3.01586013407486));
#49785=CARTESIAN_POINT('Ctrl Pts',(-48.1273946707838,1.24751100295795,-3.60186867181274));
#49786=CARTESIAN_POINT('Ctrl Pts',(-47.9285211390864,3.7045847670046,-0.897659921999986));
#49787=CARTESIAN_POINT('Ctrl Pts',(-47.7296476073888,2.75787844060516,2.63132060728692));
#49788=CARTESIAN_POINT('Ctrl Pts',(-47.5307740756916,-0.722772259698463,
3.74263835978015));
#49789=CARTESIAN_POINT('Ctrl Pts',(-47.3729670568041,-2.95772977401545,
1.89581558441457));
#49790=CARTESIAN_POINT('Ctrl Pts',(-47.2814512151493,-3.22089482789791,
0.41177929506686));
#49791=CARTESIAN_POINT('Ctrl Pts',(-47.256226550727,-3.21862958324598,0.00195996754723593));
#49792=CARTESIAN_POINT('Origin',(-111.877773449273,0.,0.));
#49793=CARTESIAN_POINT('',(-50.0027734492733,-3.21741165506535,-0.000143917224426878));
#49794=CARTESIAN_POINT('',(-49.756226550727,-3.22413672240192,-0.00282835657440583));
#49795=CARTESIAN_POINT('',(-111.877773449273,-3.22275,5.46201577318104E-12));
#49796=CARTESIAN_POINT('Ctrl Pts',(-50.0027734492733,-3.21741165506535,
-0.000143917224427054));
#49797=CARTESIAN_POINT('Ctrl Pts',(-49.9701624631035,-3.21762205297516,
-0.5304684062323));
#49798=CARTESIAN_POINT('Ctrl Pts',(-49.8712602997012,-2.84224577629495,
-2.13854902871477));
#49799=CARTESIAN_POINT('Ctrl Pts',(-49.7060669590664,-0.302288193939447,
-3.79978466222657));
#49800=CARTESIAN_POINT('Ctrl Pts',(-49.507193427369,3.03326776036106,-2.30846882704571));
#49801=CARTESIAN_POINT('Ctrl Pts',(-49.3083198956714,3.58185106831631,1.3038729063405));
#49802=CARTESIAN_POINT('Ctrl Pts',(-49.1094463639741,0.839422260186034,
3.71821353617451));
#49803=CARTESIAN_POINT('Ctrl Pts',(-48.9242642151746,-2.43237049411793,
2.78523165147994));
#49804=CARTESIAN_POINT('Ctrl Pts',(-48.8053732436077,-3.2157010280353,0.848326521785803));
#49805=CARTESIAN_POINT('Ctrl Pts',(-48.7527734492733,-3.22360668808134,
-0.00290950365519946));
#49806=CARTESIAN_POINT('Ctrl Pts',(-49.756226550727,-3.22413672240192,-0.00282835657440569));
#49807=CARTESIAN_POINT('Ctrl Pts',(-49.7436120086058,-3.22601281988437,
-0.20688641167527));
#49808=CARTESIAN_POINT('Ctrl Pts',(-49.6647062892522,-3.11526915608657,
-1.48126866875651));
#49809=CARTESIAN_POINT('Ctrl Pts',(-49.519509392666,-1.41714857988236,-3.53856348452659));
#49810=CARTESIAN_POINT('Ctrl Pts',(-49.3206358609686,2.21081511742383,-3.10516314354943));
#49811=CARTESIAN_POINT('Ctrl Pts',(-49.1217623292711,3.80747734543496,0.181267469467265));
#49812=CARTESIAN_POINT('Ctrl Pts',(-48.9228887975737,1.90582157067163,3.30114915934591));
#49813=CARTESIAN_POINT('Ctrl Pts',(-48.7240152658761,-1.74690697639595,
3.3879282234585));
#49814=CARTESIAN_POINT('Ctrl Pts',(-48.5851278502606,-3.17693716528882,
1.27461962210879));
#49815=CARTESIAN_POINT('Ctrl Pts',(-48.5125316118776,-3.22754380504923,
0.103539226444708));
#49816=CARTESIAN_POINT('Ctrl Pts',(-48.506226550727,-3.22687206568905,0.00177085358160422));
#49817=CARTESIAN_POINT('Origin',(-111.877773449273,0.,0.));
#49818=CARTESIAN_POINT('',(-51.2527734492733,-3.223076684641,0.0029595821066306));
#49819=CARTESIAN_POINT('',(-51.006226550727,-3.2174581254241,-0.000432486719161296));
#49820=CARTESIAN_POINT('',(-111.877773449273,-3.22275,5.46201577318104E-12));
#49821=CARTESIAN_POINT('Ctrl Pts',(-51.2527734492733,-3.223076684641,0.00295958210663055));
#49822=CARTESIAN_POINT('Ctrl Pts',(-51.2012428598317,-3.21532624848516,
-0.831324944861402));
#49823=CARTESIAN_POINT('Ctrl Pts',(-51.0834210931577,-2.45815795239362,
-2.75134438455826));
#49824=CARTESIAN_POINT('Ctrl Pts',(-50.8993081492511,0.779366140619599,
-3.73126386769187));
#49825=CARTESIAN_POINT('Ctrl Pts',(-50.7004346175537,3.56036378015273,-1.36145193982897));
#49826=CARTESIAN_POINT('Ctrl Pts',(-50.5015610858562,3.07009186808429,2.25926482578078));
#49827=CARTESIAN_POINT('Ctrl Pts',(-50.3026875541588,-0.240986756115434,
3.80416443057663));
#49828=CARTESIAN_POINT('Ctrl Pts',(-50.1364250086311,-2.82400848125359,
2.17360945505402));
#49829=CARTESIAN_POINT('Ctrl Pts',(-50.036453640336,-3.21719435891352,0.547568133616722));
#49830=CARTESIAN_POINT('Ctrl Pts',(-50.0027734492733,-3.21741165506535,
-0.000143917224427054));
#49831=CARTESIAN_POINT('Ctrl Pts',(-51.006226550727,-3.2174581254241,-0.000432486719161573));
#49832=CARTESIAN_POINT('Ctrl Pts',(-50.9746924053341,-3.2180700033416,-0.513226776194044));
#49833=CARTESIAN_POINT('Ctrl Pts',(-50.8768670827086,-2.8602169712618,-2.10321212263254));
#49834=CARTESIAN_POINT('Ctrl Pts',(-50.7127505828507,-0.363947962184506,
-3.79437524663933));
#49835=CARTESIAN_POINT('Ctrl Pts',(-50.5138770511533,2.99538371751683,-2.35741765843947));
#49836=CARTESIAN_POINT('Ctrl Pts',(-50.3150035194558,3.60255068722456,1.24554011475546));
#49837=CARTESIAN_POINT('Ctrl Pts',(-50.1161299877584,0.899686688491969,
3.70409307307982));
#49838=CARTESIAN_POINT('Ctrl Pts',(-49.929870998182,-2.40593533673339,2.8192447831268));
#49839=CARTESIAN_POINT('Ctrl Pts',(-49.8099031858383,-3.21615366609824,
0.865467112255008));
#49840=CARTESIAN_POINT('Ctrl Pts',(-49.756226550727,-3.22413672240192,-0.00282835657440569));
#49841=CARTESIAN_POINT('Origin',(-111.877773449273,0.,0.));
#49842=CARTESIAN_POINT('',(-52.5027734492733,-3.22751885487476,-0.00122046435559179));
#49843=CARTESIAN_POINT('',(-52.256226550727,-3.22254425484652,0.00297929525483548));
#49844=CARTESIAN_POINT('',(-111.877773449273,-3.22275,5.46201577318104E-12));
#49845=CARTESIAN_POINT('Ctrl Pts',(-52.5027734492733,-3.22751885487476,
-0.00122046435559201));
#49846=CARTESIAN_POINT('Ctrl Pts',(-52.4986144337925,-3.22784327448082,
-0.0683144855938748));
#49847=CARTESIAN_POINT('Ctrl Pts',(-52.4281642410792,-3.19548702846004,
-1.20451144458635));
#49848=CARTESIAN_POINT('Ctrl Pts',(-52.2914228711333,-1.8556119748251,-3.32963148567123));
#49849=CARTESIAN_POINT('Ctrl Pts',(-52.0925493394359,1.79801185590047,-3.36108538980027));
#49850=CARTESIAN_POINT('Ctrl Pts',(-51.8936758077384,3.79961870161625,-0.304367136556382));
#49851=CARTESIAN_POINT('Ctrl Pts',(-51.694802276041,2.31012808263415,3.03200426670422));
#49852=CARTESIAN_POINT('Ctrl Pts',(-51.4959287443436,-1.30191296199484,
3.58256392418577));
#49853=CARTESIAN_POINT('Ctrl Pts',(-51.3485858020876,-3.09177951640618,
1.55171129825264));
#49854=CARTESIAN_POINT('Ctrl Pts',(-51.2675340370642,-3.22529674450323,
0.241934725538514));
#49855=CARTESIAN_POINT('Ctrl Pts',(-51.2527734492733,-3.223076684641,0.00295958210663055));
#49856=CARTESIAN_POINT('Ctrl Pts',(-52.256226550727,-3.22254425484652,0.00297929525483558));
#49857=CARTESIAN_POINT('Ctrl Pts',(-52.2057728020623,-3.21502087541627,
-0.814216185777217));
#49858=CARTESIAN_POINT('Ctrl Pts',(-52.0890278761651,-2.48366918414892,
-2.71710498222641));
#49859=CARTESIAN_POINT('Ctrl Pts',(-51.9059917730355,0.718676385120064,
-3.74342702412619));
#49860=CARTESIAN_POINT('Ctrl Pts',(-51.707118241338,3.53778758602515,-1.41908443288405));
#49861=CARTESIAN_POINT('Ctrl Pts',(-51.5082447096405,3.10637228884811,2.2091158490591));
#49862=CARTESIAN_POINT('Ctrl Pts',(-51.3093711779431,-0.179184245551611,
3.80757595296977));
#49863=CARTESIAN_POINT('Ctrl Pts',(-51.1420317916386,-2.80524068683852,
2.20889053097753));
#49864=CARTESIAN_POINT('Ctrl Pts',(-51.0409835825666,-3.21678371170541,
0.564770953054575));
#49865=CARTESIAN_POINT('Ctrl Pts',(-51.006226550727,-3.2174581254241,-0.000432486719161573));
#49866=CARTESIAN_POINT('Origin',(-111.877773449273,0.,0.));
#49867=CARTESIAN_POINT('',(-53.7527734492733,-3.21934317032028,-0.00235959395598513));
#49868=CARTESIAN_POINT('',(-53.506226550727,-3.22776089439009,-0.000918729460922529));
#49869=CARTESIAN_POINT('',(-111.877773449273,-3.22275,5.46201577318104E-12));
#49870=CARTESIAN_POINT('Ctrl Pts',(-53.7527734492733,-3.21934317032028,
-0.00235959395598572));
#49871=CARTESIAN_POINT('Ctrl Pts',(-53.7296948305207,-3.22187288607612,
-0.377104113301222));
#49872=CARTESIAN_POINT('Ctrl Pts',(-53.6403250345356,-2.98795702091302,
-1.82520830613947));
#49873=CARTESIAN_POINT('Ctrl Pts',(-53.484664061318,-0.843490472210508,
-3.71729275882027));
#49874=CARTESIAN_POINT('Ctrl Pts',(-53.2857905296207,2.67129554096001,-2.71917667030568));
#49875=CARTESIAN_POINT('Ctrl Pts',(-53.086916997923,3.73168972619857,0.777324526096578));
#49876=CARTESIAN_POINT('Ctrl Pts',(-52.8880434662258,1.36339972882987,3.55961835186216));
#49877=CARTESIAN_POINT('Ctrl Pts',(-52.6933289500089,-2.18185957656017,
3.08153908756355));
#49878=CARTESIAN_POINT('Ctrl Pts',(-52.5649056110249,-3.22267230127756,
1.00110727387197));
#49879=CARTESIAN_POINT('Ctrl Pts',(-52.5027734492733,-3.22751885487476,
-0.00122046435559201));
#49880=CARTESIAN_POINT('Ctrl Pts',(-53.506226550727,-3.22776089439009,-0.000918729460922746));
#49881=CARTESIAN_POINT('Ctrl Pts',(-53.503144376023,-3.22794811375422,-0.0506310245026929));
#49882=CARTESIAN_POINT('Ctrl Pts',(-53.4337710240866,-3.20434578131378,
-1.16936988671058));
#49883=CARTESIAN_POINT('Ctrl Pts',(-53.2981064949176,-1.90943276487233,
-3.29906170720093));
#49884=CARTESIAN_POINT('Ctrl Pts',(-53.0992329632202,1.74319863589507,-3.38983777595641));
#49885=CARTESIAN_POINT('Ctrl Pts',(-52.9003594315227,3.79417555074013,-0.366023935902194));
#49886=CARTESIAN_POINT('Ctrl Pts',(-52.7014858998253,2.35905617908858,2.99409344800579));
#49887=CARTESIAN_POINT('Ctrl Pts',(-52.5026123681278,-1.24356885369478,
3.60323162419618));
#49888=CARTESIAN_POINT('Ctrl Pts',(-52.3541925850951,-3.07949606830474,
1.58708207888242));
#49889=CARTESIAN_POINT('Ctrl Pts',(-52.2720639792948,-3.22490584318174,
0.259496905924056));
#49890=CARTESIAN_POINT('Ctrl Pts',(-52.256226550727,-3.22254425484652,0.00297929525483558));
#49891=CARTESIAN_POINT('Origin',(-111.877773449273,0.,0.));
#49892=CARTESIAN_POINT('',(-55.0027734492732,-3.2189220646149,0.00214340917629934));
#49893=CARTESIAN_POINT('',(-54.756226550727,-3.21975139093016,-0.00252752881742452));
#49894=CARTESIAN_POINT('',(-111.877773449273,-3.22275,5.46201577318104E-12));
#49895=CARTESIAN_POINT('Ctrl Pts',(-55.0027734492732,-3.2189220646149,0.00214340917629927));
#49896=CARTESIAN_POINT('Ctrl Pts',(-54.9607752272489,-3.21477455481245,
-0.680036647789328));
#49897=CARTESIAN_POINT('Ctrl Pts',(-54.8524858279921,-2.66831154574978,
-2.44506023208848));
#49898=CARTESIAN_POINT('Ctrl Pts',(-54.6779052515027,0.236823844100095,
-3.80442585659819));
#49899=CARTESIAN_POINT('Ctrl Pts',(-54.4790317198054,3.32861572061708,-1.857433448592));
#49900=CARTESIAN_POINT('Ctrl Pts',(-54.2801581881078,3.36206863847578,1.79617262579773));
#49901=CARTESIAN_POINT('Ctrl Pts',(-54.0812846564105,0.306445988059607,
3.7994516035725));
#49902=CARTESIAN_POINT('Ctrl Pts',(-53.9054897434655,-2.64347043160142,
2.48442526820891));
#49903=CARTESIAN_POINT('Ctrl Pts',(-53.7959860077532,-3.21460651379814,
0.699314524015979));
#49904=CARTESIAN_POINT('Ctrl Pts',(-53.7527734492733,-3.21934317032028,
-0.00235959395598572));
#49905=CARTESIAN_POINT('Ctrl Pts',(-54.756226550727,-3.21975139093016,-0.00252752881742448));
#49906=CARTESIAN_POINT('Ctrl Pts',(-54.7342247727513,-3.22235614149659,
-0.359672668312695));
#49907=CARTESIAN_POINT('Ctrl Pts',(-54.6459318175431,-3.00257958162626,
-1.78977856998388));
#49908=CARTESIAN_POINT('Ctrl Pts',(-54.4913476851023,-0.90373941289318,
-3.70310635886562));
#49909=CARTESIAN_POINT('Ctrl Pts',(-54.2924741534049,2.62679028492706,-2.76219377135282));
#49910=CARTESIAN_POINT('Ctrl Pts',(-54.0936006217074,3.74381967543987,0.71662812481567));
#49911=CARTESIAN_POINT('Ctrl Pts',(-53.89472709001,1.42101986107626,3.53701062847065));
#49912=CARTESIAN_POINT('Ctrl Pts',(-53.6989357330165,-2.15118182487284,
3.11423588293571));
#49913=CARTESIAN_POINT('Ctrl Pts',(-53.5694355532555,-3.2239214140241,1.01857720597386));
#49914=CARTESIAN_POINT('Ctrl Pts',(-53.506226550727,-3.22776089439009,-0.000918729460922746));
#49915=CARTESIAN_POINT('Origin',(-111.877773449273,0.,0.));
#49916=CARTESIAN_POINT('',(-56.2527734492733,-3.22717748004024,0.00154131605262783));
#49917=CARTESIAN_POINT('',(-56.006226550727,-3.21858653956579,0.00193011919197975));
#49918=CARTESIAN_POINT('',(-111.877773449273,-3.22275,5.46201577318104E-12));
#49919=CARTESIAN_POINT('Ctrl Pts',(-56.2527734492733,-3.22717748004024,
0.00154131605262783));
#49920=CARTESIAN_POINT('Ctrl Pts',(-56.1918556239772,-3.22138456848205,
-0.981472074920973));
#49921=CARTESIAN_POINT('Ctrl Pts',(-56.0646466214485,-2.2158673361632,-3.04445687931626));
#49922=CARTESIAN_POINT('Ctrl Pts',(-55.8711464416876,1.29799190468937,-3.58398641834039));
#49923=CARTESIAN_POINT('Ctrl Pts',(-55.67227290999,3.71683070089097,-0.845524199773049));
#49924=CARTESIAN_POINT('Ctrl Pts',(-55.4733993782926,2.7206378174474,2.66980738963741));
#49925=CARTESIAN_POINT('Ctrl Pts',(-55.2745258465951,-0.77528267887785,
3.73211446760674));
#49926=CARTESIAN_POINT('Ctrl Pts',(-55.117650536922,-2.97103196108619,1.86516234467601));
#49927=CARTESIAN_POINT('Ctrl Pts',(-55.0270664044814,-3.2213211011693,0.396735579248406));
#49928=CARTESIAN_POINT('Ctrl Pts',(-55.0027734492732,-3.2189220646149,0.00214340917629927));
#49929=CARTESIAN_POINT('Ctrl Pts',(-56.006226550727,-3.21858653956579,0.00193011919197968));
#49930=CARTESIAN_POINT('Ctrl Pts',(-55.9653051694795,-3.21497056641272,
-0.662932432587956));
#49931=CARTESIAN_POINT('Ctrl Pts',(-55.8580926109995,-2.68988099457248,
-2.41008537974996));
#49932=CARTESIAN_POINT('Ctrl Pts',(-55.6845888752871,0.175017637425035,
-3.80776974856381));
#49933=CARTESIAN_POINT('Ctrl Pts',(-55.4857153435897,3.29801649958808,-1.9112375048466));
#49934=CARTESIAN_POINT('Ctrl Pts',(-55.2868418118921,3.39079103020278,1.74134368261521));
#49935=CARTESIAN_POINT('Ctrl Pts',(-55.0879682801948,0.368099800048924,
3.79397471903694));
#49936=CARTESIAN_POINT('Ctrl Pts',(-54.9110965264729,-2.62097893908948,
2.5192607169782));
#49937=CARTESIAN_POINT('Ctrl Pts',(-54.8005159499837,-3.21450804932711,
0.716402718236941));
#49938=CARTESIAN_POINT('Ctrl Pts',(-54.756226550727,-3.21975139093016,-0.00252752881742448));
#49939=CARTESIAN_POINT('Origin',(-111.877773449273,0.,0.));
#49940=CARTESIAN_POINT('',(-57.5027734492733,-3.22367845862114,-0.00290036030699531));
#49941=CARTESIAN_POINT('',(-57.256226550727,-3.22682140413586,0.00180517358502927));
#49942=CARTESIAN_POINT('',(-111.877773449273,-3.22275,5.46201577318104E-12));
#49943=CARTESIAN_POINT('Ctrl Pts',(-57.5027734492733,-3.22367845862114,
-0.0029003603069952));
#49944=CARTESIAN_POINT('Ctrl Pts',(-57.4892271979379,-3.22571274738317,
-0.222110297568779));
#49945=CARTESIAN_POINT('Ctrl Pts',(-57.40938976937,-3.10523178828499,-1.51184308272459));
#49946=CARTESIAN_POINT('Ctrl Pts',(-57.2632611635696,-1.3672940818287,-3.55812429873996));
#49947=CARTESIAN_POINT('Ctrl Pts',(-57.0643876318723,2.25422253794341,-3.073796086424));
#49948=CARTESIAN_POINT('Ctrl Pts',(-56.8655141001747,3.80455486131976,0.234742281439464));
#49949=CARTESIAN_POINT('Ctrl Pts',(-56.6666405684773,1.85925436632751,3.32759895912643));
#49950=CARTESIAN_POINT('Ctrl Pts',(-56.4677670367798,-1.79433285800241,
3.3630508807005));
#49951=CARTESIAN_POINT('Ctrl Pts',(-56.3298113303785,-3.18513816811937,
1.24417006843104));
#49952=CARTESIAN_POINT('Ctrl Pts',(-56.2581468012097,-3.227688452853,0.0882495477107612));
#49953=CARTESIAN_POINT('Ctrl Pts',(-56.2527734492733,-3.22717748004024,
0.00154131605262783));
#49954=CARTESIAN_POINT('Ctrl Pts',(-57.256226550727,-3.22682140413586,0.00180517358502903));
#49955=CARTESIAN_POINT('Ctrl Pts',(-57.1963855662077,-3.22034692564174,
-0.964112732485139));
#49956=CARTESIAN_POINT('Ctrl Pts',(-57.070253404456,-2.24550654357098,-3.01139463839781));
#49957=CARTESIAN_POINT('Ctrl Pts',(-56.8778300654718,1.23962521535938,-3.60459026200378));
#49958=CARTESIAN_POINT('Ctrl Pts',(-56.6789565337743,3.70261133887159,-0.905765369589214));
#49959=CARTESIAN_POINT('Ctrl Pts',(-56.4800830020769,2.76363056175831,2.62527860418717));
#49960=CARTESIAN_POINT('Ctrl Pts',(-56.2812094703794,-0.714579649985331,
3.74421120602382));
#49961=CARTESIAN_POINT('Ctrl Pts',(-56.1232573199295,-2.9556327925769,1.9005901476665));
#49962=CARTESIAN_POINT('Ctrl Pts',(-56.031596346712,-3.22082831387507,0.41412117390532));
#49963=CARTESIAN_POINT('Ctrl Pts',(-56.006226550727,-3.21858653956579,0.00193011919197968));
#49964=CARTESIAN_POINT('Origin',(-111.877773449273,0.,0.));
#49965=CARTESIAN_POINT('',(-58.7527734492733,-3.21741520282347,-0.000182944744591371));
#49966=CARTESIAN_POINT('',(-58.5062265507269,-3.224207581543,-0.00281507645755574));
#49967=CARTESIAN_POINT('',(-111.877773449273,-3.22275,5.46201577318104E-12));
#49968=CARTESIAN_POINT('Ctrl Pts',(-58.7527734492732,-3.21741520282347,
-0.000182944744591441));
#49969=CARTESIAN_POINT('Ctrl Pts',(-58.7203075946661,-3.21768148241439,
-0.528145832653428));
#49970=CARTESIAN_POINT('Ctrl Pts',(-58.6215505628265,-2.84469095478287,
-2.13378793357218));
#49971=CARTESIAN_POINT('Ctrl Pts',(-58.4565023537544,-0.310603415235633,
-3.79911399538513));
#49972=CARTESIAN_POINT('Ctrl Pts',(-58.2576288220569,3.02820834138102,-2.3151016981286));
#49973=CARTESIAN_POINT('Ctrl Pts',(-58.0587552903595,3.58469605619972,1.29603079290335));
#49974=CARTESIAN_POINT('Ctrl Pts',(-57.859881758662,0.84755767422402,3.71636753031121));
#49975=CARTESIAN_POINT('Ctrl Pts',(-57.6745544783,-2.42883487841989,2.78982271261159));
#49976=CARTESIAN_POINT('Ctrl Pts',(-57.5555183751704,-3.21575756542716,
0.85063554497991));
#49977=CARTESIAN_POINT('Ctrl Pts',(-57.5027734492733,-3.22367845862114,
-0.0029003603069952));
#49978=CARTESIAN_POINT('Ctrl Pts',(-58.5062265507269,-3.224207581543,-0.00281507645755581));
#49979=CARTESIAN_POINT('Ctrl Pts',(-58.4937571401684,-3.22605800120511,
-0.204513997007941));
#49980=CARTESIAN_POINT('Ctrl Pts',(-58.4149965523774,-3.11681064543685,
-1.47650733819638));
#49981=CARTESIAN_POINT('Ctrl Pts',(-58.2699447873541,-1.42488944071483,
-3.53545353713309));
#49982=CARTESIAN_POINT('Ctrl Pts',(-58.0710712556564,2.20401407814638,-3.10999414385624));
#49983=CARTESIAN_POINT('Ctrl Pts',(-57.8721977239591,3.80786493656502,0.172934254461413));
#49984=CARTESIAN_POINT('Ctrl Pts',(-57.6733241922616,1.9130416726831,3.29697030469875));
#49985=CARTESIAN_POINT('Ctrl Pts',(-57.4744506605642,-1.73948820805607,
3.39174326940018));
#49986=CARTESIAN_POINT('Ctrl Pts',(-57.3354181133859,-3.1756391642871,1.27936435020756));
#49987=CARTESIAN_POINT('Ctrl Pts',(-57.2626767434402,-3.22751928092282,
0.105920383075324));
#49988=CARTESIAN_POINT('Ctrl Pts',(-57.256226550727,-3.22682140413586,0.00180517358502903));
#49989=CARTESIAN_POINT('Origin',(-111.877773449273,0.,0.));
#49990=CARTESIAN_POINT('',(-60.0027734492732,-3.22300473664784,0.00296403349578234));
#49991=CARTESIAN_POINT('',(-59.756226550727,-3.21746794082411,-0.000471133578089089));
#49992=CARTESIAN_POINT('',(-111.877773449273,-3.22275,5.46201577318104E-12));
#49993=CARTESIAN_POINT('Ctrl Pts',(-60.0027734492732,-3.22300473664784,
0.00296403349578239));
#49994=CARTESIAN_POINT('Ctrl Pts',(-59.9513879913943,-3.21528094263802,
-0.829018345407677));
#49995=CARTESIAN_POINT('Ctrl Pts',(-59.833711356283,-2.46162310557184,-2.74673607057375));
#49996=CARTESIAN_POINT('Ctrl Pts',(-59.6497435439391,0.77119828879821,-3.73296059861904));
#49997=CARTESIAN_POINT('Ctrl Pts',(-59.4508700122417,3.55737567435549,-1.36924064466089));
#49998=CARTESIAN_POINT('Ctrl Pts',(-59.2519964805442,3.07502898605303,2.25254042503595));
#49999=CARTESIAN_POINT('Ctrl Pts',(-59.0531229488468,-0.232660648507626,
3.80468272713029));
#50000=CARTESIAN_POINT('Ctrl Pts',(-58.8867152717565,-2.8215025518602,2.17836629560583));
#50001=CARTESIAN_POINT('Ctrl Pts',(-58.7865987718986,-3.21713777309984,
0.549887744409677));
#50002=CARTESIAN_POINT('Ctrl Pts',(-58.7527734492732,-3.21741520282347,
-0.000182944744591441));
#50003=CARTESIAN_POINT('Ctrl Pts',(-59.7562265507269,-3.21746794082411,
-0.000471133578089228));
#50004=CARTESIAN_POINT('Ctrl Pts',(-59.7248375368967,-3.21813154016163,
-0.510901476063965));
#50005=CARTESIAN_POINT('Ctrl Pts',(-59.6271573458339,-2.86260884250598,
-2.0984477708445));
#50006=CARTESIAN_POINT('Ctrl Pts',(-59.4631859775387,-0.372251197144022,
-3.79356964845936));
#50007=CARTESIAN_POINT('Ctrl Pts',(-59.2643124458413,2.99021726324463,-2.36396750190888));
#50008=CARTESIAN_POINT('Ctrl Pts',(-59.0654389141438,3.60526796243309,1.23765283926516));
#50009=CARTESIAN_POINT('Ctrl Pts',(-58.8665653824463,0.90779105514019,3.70211521048372));
#50010=CARTESIAN_POINT('Ctrl Pts',(-58.6801612613074,-2.40233678911353,
2.82381966648872));
#50011=CARTESIAN_POINT('Ctrl Pts',(-58.5600483174009,-3.21622060775338,
0.867778781152312));
#50012=CARTESIAN_POINT('Ctrl Pts',(-58.5062265507269,-3.224207581543,-0.00281507645755581));
#50013=CARTESIAN_POINT('Origin',(-111.877773449273,0.,0.));
#50014=CARTESIAN_POINT('',(-61.2527734492733,-3.22755496513108,-0.00118065924393767));
#50015=CARTESIAN_POINT('',(-61.006226550727,-3.22247286999595,0.00297960598500319));
#50016=CARTESIAN_POINT('',(-111.877773449273,-3.22275,5.46201577318104E-12));
#50017=CARTESIAN_POINT('Ctrl Pts',(-61.2527734492733,-3.22755496513108,
-0.00118065924393777));
#50018=CARTESIAN_POINT('Ctrl Pts',(-61.2487595653551,-3.22785919387834,
-0.065931465168597));
#50019=CARTESIAN_POINT('Ctrl Pts',(-61.1784545042045,-3.19669833842117,
-1.19977375893129));
#50020=CARTESIAN_POINT('Ctrl Pts',(-61.0418582658212,-1.86289453152446,
-3.32556244805351));
#50021=CARTESIAN_POINT('Ctrl Pts',(-60.8429847341239,1.79065171153737,-3.3650123446216));
#50022=CARTESIAN_POINT('Ctrl Pts',(-60.6441112024263,3.79894348534265,-0.312681989663811));
#50023=CARTESIAN_POINT('Ctrl Pts',(-60.445237670729,2.31675818454863,3.02694121941845));
#50024=CARTESIAN_POINT('Ctrl Pts',(-60.2463641390315,-1.29406929314464,
3.58540462096363));
#50025=CARTESIAN_POINT('Ctrl Pts',(-60.0988760652129,-3.0901435215559,1.55647752678745));
#50026=CARTESIAN_POINT('Ctrl Pts',(-60.0176791686268,-3.22524522861985,
0.244302660394943));
#50027=CARTESIAN_POINT('Ctrl Pts',(-60.0027734492732,-3.22300473664784,
0.00296403349578239));
#50028=CARTESIAN_POINT('Ctrl Pts',(-61.006226550727,-3.22247286999594,0.00297960598500333));
#50029=CARTESIAN_POINT('Ctrl Pts',(-60.9559179336249,-3.21498508007288,
-0.811911263580403));
#50030=CARTESIAN_POINT('Ctrl Pts',(-60.8393181392904,-2.48707231186256,
-2.71248222746116));
#50031=CARTESIAN_POINT('Ctrl Pts',(-60.6564271677235,0.71048205919978,-3.74499090453405));
#50032=CARTESIAN_POINT('Ctrl Pts',(-60.4575536360259,3.53467340381617,-1.42682359100281));
#50033=CARTESIAN_POINT('Ctrl Pts',(-60.2586801043286,3.1111995673583,2.20231216759956));
#50034=CARTESIAN_POINT('Ctrl Pts',(-60.059806572631,-0.170850819729117,
3.80795898466428));
#50035=CARTESIAN_POINT('Ctrl Pts',(-59.8923220547639,-2.80268032222874,
2.21364306226118));
#50036=CARTESIAN_POINT('Ctrl Pts',(-59.7911287141292,-3.21673006952186,
0.567088054971965));
#50037=CARTESIAN_POINT('Ctrl Pts',(-59.7562265507269,-3.21746794082411,
-0.000471133578089228));
#50038=CARTESIAN_POINT('Origin',(-111.877773449273,0.,0.));
#50039=CARTESIAN_POINT('',(-62.5027734492733,-3.21939635421877,-0.002383576536604));
#50040=CARTESIAN_POINT('',(-62.256226550727,-3.22778876783897,-0.000877024610755894));
#50041=CARTESIAN_POINT('',(-111.877773449273,-3.22275,5.46201577318104E-12));
#50042=CARTESIAN_POINT('Ctrl Pts',(-62.5027734492733,-3.21939635421877,
-0.00238357653660443));
#50043=CARTESIAN_POINT('Ctrl Pts',(-62.4798399620833,-3.22193840446921,
-0.37475602650426));
#50044=CARTESIAN_POINT('Ctrl Pts',(-62.3906152976609,-2.98994884724002,
-1.82043316881518));
#50045=CARTESIAN_POINT('Ctrl Pts',(-62.2350994560059,-0.851623861356168,
-3.71543785175534));
#50046=CARTESIAN_POINT('Ctrl Pts',(-62.0362259243087,2.66533814213779,-2.72501637051098));
#50047=CARTESIAN_POINT('Ctrl Pts',(-61.837352392611,3.73338198796987,0.76915574716017));
#50048=CARTESIAN_POINT('Ctrl Pts',(-61.6384788609137,1.37118679760446,3.5566259850542));
#50049=CARTESIAN_POINT('Ctrl Pts',(-61.4436192131343,-2.17775356114322,
3.08595621928119));
#50050=CARTESIAN_POINT('Ctrl Pts',(-61.3150507425876,-3.22283471329673,
1.00345849204261));
#50051=CARTESIAN_POINT('Ctrl Pts',(-61.2527734492733,-3.22755496513108,
-0.00118065924393777));
#50052=CARTESIAN_POINT('Ctrl Pts',(-62.256226550727,-3.22778876783897,-0.00087702461075625));
#50053=CARTESIAN_POINT('Ctrl Pts',(-62.2532895075857,-3.22795988649932,
-0.0482474052521493));
#50054=CARTESIAN_POINT('Ctrl Pts',(-62.1840612872119,-3.20551702323328,
-1.16463561095075));
#50055=CARTESIAN_POINT('Ctrl Pts',(-62.0485418896055,-1.91664828978265,
-3.29487495434361));
#50056=CARTESIAN_POINT('Ctrl Pts',(-61.8496683579083,1.73577569732174,-3.39364470150818));
#50057=CARTESIAN_POINT('Ctrl Pts',(-61.6507948262106,3.79336540970629,-0.374326728849534));
#50058=CARTESIAN_POINT('Ctrl Pts',(-61.4519212945133,2.36560319483962,2.9889234108709));
#50059=CARTESIAN_POINT('Ctrl Pts',(-61.2530477628157,-1.23568009267388,
3.6059445836087));
#50060=CARTESIAN_POINT('Ctrl Pts',(-61.1044828482204,-3.07781487847321,
1.59185030130126));
#50061=CARTESIAN_POINT('Ctrl Pts',(-61.0222091108574,-3.224851668293,0.261862538429334));
#50062=CARTESIAN_POINT('Ctrl Pts',(-61.006226550727,-3.22247286999594,0.00297960598500333));
#50063=CARTESIAN_POINT('Origin',(-111.877773449273,0.,0.));
#50064=CARTESIAN_POINT('',(-63.7527734492732,-3.21887470245503,0.0021157953170018));
#50065=CARTESIAN_POINT('',(-63.506226550727,-3.21980873461777,-0.00254834726308467));
#50066=CARTESIAN_POINT('',(-111.877773449273,-3.22275,5.46201577318104E-12));
#50067=CARTESIAN_POINT('Ctrl Pts',(-63.7527734492732,-3.21887470245503,
0.00211579531700205));
#50068=CARTESIAN_POINT('Ctrl Pts',(-63.7109203588115,-3.21479847498223,
-0.677731968031492));
#50069=CARTESIAN_POINT('Ctrl Pts',(-63.6027760911173,-2.67124363934922,
-2.4403500396236));
#50070=CARTESIAN_POINT('Ctrl Pts',(-63.4283406461908,0.228497174322965,
-3.80493504186522));
#50071=CARTESIAN_POINT('Ctrl Pts',(-63.2294671144933,3.32454269908083,-1.8647137778962));
#50072=CARTESIAN_POINT('Ctrl Pts',(-63.0305935827958,3.36599156573087,1.78881033396948));
#50073=CARTESIAN_POINT('Ctrl Pts',(-62.8317200510984,0.314760470489306,
3.79877183806881));
#50074=CARTESIAN_POINT('Ctrl Pts',(-62.6557800065908,-2.64046460203817,
2.48912431653265));
#50075=CARTESIAN_POINT('Ctrl Pts',(-62.5461311393158,-3.21459039401224,
0.701617918411942));
#50076=CARTESIAN_POINT('Ctrl Pts',(-62.5027734492733,-3.21939635421877,
-0.00238357653660443));
#50077=CARTESIAN_POINT('Ctrl Pts',(-63.506226550727,-3.21980873461777,-0.00254834726308481));
#50078=CARTESIAN_POINT('Ctrl Pts',(-63.4843699043139,-3.22242070748555,
-0.35732171994346));
#50079=CARTESIAN_POINT('Ctrl Pts',(-63.3962220806684,-3.00452281277026,
-1.78500368537475));
#50080=CARTESIAN_POINT('Ctrl Pts',(-63.2417830797903,-0.911841610381489,
-3.70111962912095));
#50081=CARTESIAN_POINT('Ctrl Pts',(-63.0429095480929,2.62073884844303,-2.7679359674221));
#50082=CARTESIAN_POINT('Ctrl Pts',(-62.8440360163953,3.74537907222691,0.708432944471117));
#50083=CARTESIAN_POINT('Ctrl Pts',(-62.6451624846981,1.42875731416466,3.53389221237837));
#50084=CARTESIAN_POINT('Ctrl Pts',(-62.4492259961417,-2.14700966869485,
3.11862876361037));
#50085=CARTESIAN_POINT('Ctrl Pts',(-62.3195806848181,-3.22409761519604,
1.02093617415114));
#50086=CARTESIAN_POINT('Ctrl Pts',(-62.256226550727,-3.22778876783897,-0.00087702461075625));
#50087=CARTESIAN_POINT('Origin',(-111.877773449273,0.,0.));
#50088=CARTESIAN_POINT('',(-65.0027734492732,-3.22713225326276,0.00157808088591664));
#50089=CARTESIAN_POINT('',(-64.756226550727,-3.21854419053207,0.00189994234605001));
#50090=CARTESIAN_POINT('',(-111.877773449273,-3.22275,5.46201577318104E-12));
#50091=CARTESIAN_POINT('Ctrl Pts',(-65.0027734492732,-3.22713225326276,
0.00157808088591662));
#50092=CARTESIAN_POINT('Ctrl Pts',(-64.9420007555398,-3.2212390697275,-0.979129695932009));
#50093=CARTESIAN_POINT('Ctrl Pts',(-64.8149368845739,-2.219890297518,-3.04001052674665));
#50094=CARTESIAN_POINT('Ctrl Pts',(-64.6215818363755,1.29014513205747,-3.5868185303575));
#50095=CARTESIAN_POINT('Ctrl Pts',(-64.422708304678,3.71497134405747,-0.853656572820322));
#50096=CARTESIAN_POINT('Ctrl Pts',(-64.2238347729806,2.72647425728869,2.66384679661379));
#50097=CARTESIAN_POINT('Ctrl Pts',(-64.024961241283,-0.767112975271716,
3.73380225971558));
#50098=CARTESIAN_POINT('Ctrl Pts',(-63.8679408000473,-2.96897803075723,
1.86993733095529));
#50099=CARTESIAN_POINT('Ctrl Pts',(-63.777211536044,-3.22125481822615,0.399079996726682));
#50100=CARTESIAN_POINT('Ctrl Pts',(-63.7527734492732,-3.21887470245503,
0.00211579531700205));
#50101=CARTESIAN_POINT('Ctrl Pts',(-64.756226550727,-3.21854419053207,0.00189994234605008));
#50102=CARTESIAN_POINT('Ctrl Pts',(-64.7154503010421,-3.2150001780999,-0.660626443449188));
#50103=CARTESIAN_POINT('Ctrl Pts',(-64.6083828741248,-2.69275524640072,
-2.40536709103522));
#50104=CARTESIAN_POINT('Ctrl Pts',(-64.435024269975,0.16668379745318,-3.80814366104459));
#50105=CARTESIAN_POINT('Ctrl Pts',(-64.2361507382776,3.2938257995051,-1.91845073796596));
#50106=CARTESIAN_POINT('Ctrl Pts',(-64.0372772065801,3.39459389384955,1.73391866225805));
#50107=CARTESIAN_POINT('Ctrl Pts',(-63.8384036748827,0.376402148498568,
3.79316003539174));
#50108=CARTESIAN_POINT('Ctrl Pts',(-63.6613867895983,-2.6179141453899,2.52395018421684));
#50109=CARTESIAN_POINT('Ctrl Pts',(-63.5506610815464,-3.21449859752266,
0.71870541071796));
#50110=CARTESIAN_POINT('Ctrl Pts',(-63.506226550727,-3.21980873461777,-0.00254834726308481));
#50111=CARTESIAN_POINT('Origin',(-111.877773449273,0.,0.));
#50112=CARTESIAN_POINT('',(-66.2527734492732,-3.22375014837333,-0.00289065711299991));
#50113=CARTESIAN_POINT('',(-66.0062265507269,-3.22676995476309,0.00183908904011605));
#50114=CARTESIAN_POINT('',(-111.877773449273,-3.22275,5.46201577318104E-12));
#50115=CARTESIAN_POINT('Ctrl Pts',(-66.2527734492732,-3.22375014837333,
-0.00289065711299982));
#50116=CARTESIAN_POINT('Ctrl Pts',(-66.2393723295005,-3.22576060998705,
-0.219739632465005));
#50117=CARTESIAN_POINT('Ctrl Pts',(-66.1596800324953,-3.10681143896077,
-1.50707965918289));
#50118=CARTESIAN_POINT('Ctrl Pts',(-66.0136965582577,-1.37507787149593,
-3.555123412599));
#50119=CARTESIAN_POINT('Ctrl Pts',(-65.8148230265601,2.24749004247856,-3.07872216032026));
#50120=CARTESIAN_POINT('Ctrl Pts',(-65.6159494948628,3.80505949071416,0.22641533431646));
#50121=CARTESIAN_POINT('Ctrl Pts',(-65.4170759631652,1.8665324660573,3.32352195489086));
#50122=CARTESIAN_POINT('Ctrl Pts',(-65.2182024314679,-1.78696842091292,
3.36696977921506));
#50123=CARTESIAN_POINT('Ctrl Pts',(-65.0801015935038,-3.18387565979518,
1.24891197307991));
#50124=CARTESIAN_POINT('Ctrl Pts',(-65.0082919327723,-3.22766738564045,
0.0906315578881633));
#50125=CARTESIAN_POINT('Ctrl Pts',(-65.0027734492732,-3.22713225326276,
0.00157808088591662));
#50126=CARTESIAN_POINT('Ctrl Pts',(-66.0062265507269,-3.22676995476309,
0.00183908904011598));
#50127=CARTESIAN_POINT('Ctrl Pts',(-65.9465306977704,-3.22021441834723,
-0.961776633740155));
#50128=CARTESIAN_POINT('Ctrl Pts',(-65.8205436675812,-2.24946408802035,
-3.00692622463982));
#50129=CARTESIAN_POINT('Ctrl Pts',(-65.6282654601599,1.23173349036234,-3.60729458738919));
#50130=CARTESIAN_POINT('Ctrl Pts',(-65.4293919284621,3.70062017644406,-0.913866478859252));
#50131=CARTESIAN_POINT('Ctrl Pts',(-65.230518396765,2.76936944602707,2.61922402686354));
#50132=CARTESIAN_POINT('Ctrl Pts',(-65.0316448650673,-0.706383617669903,
3.74576611872324));
#50133=CARTESIAN_POINT('Ctrl Pts',(-64.8735475830548,-2.95352906927565,
1.9053646207508));
#50134=CARTESIAN_POINT('Ctrl Pts',(-64.7817414782746,-3.22076178585125,
0.416462656245822));
#50135=CARTESIAN_POINT('Ctrl Pts',(-64.756226550727,-3.21854419053207,0.00189994234605008));
#50136=CARTESIAN_POINT('Origin',(-111.877773449273,0.,0.));
#50137=CARTESIAN_POINT('',(-67.5027734492732,-3.21741959772868,-0.000221941790678977));
#50138=CARTESIAN_POINT('',(-67.256226550727,-3.22427826197944,-0.00280124290513745));
#50139=CARTESIAN_POINT('',(-111.877773449273,-3.22275,5.46201577318104E-12));
#50140=CARTESIAN_POINT('Ctrl Pts',(-67.5027734492732,-3.21741959772868,
-0.000221941790679026));
#50141=CARTESIAN_POINT('Ctrl Pts',(-67.4704527262287,-3.21774121840307,
-0.525822896622257));
#50142=CARTESIAN_POINT('Ctrl Pts',(-67.3718408259518,-2.84712891776362,
-2.12902637166851));
#50143=CARTESIAN_POINT('Ctrl Pts',(-67.2069377484423,-0.318917148843096,
-3.79842513203319));
#50144=CARTESIAN_POINT('Ctrl Pts',(-67.008064216745,3.02313441827591,-2.32172348063307));
#50145=CARTESIAN_POINT('Ctrl Pts',(-66.8091906850474,3.58752387456407,1.28818247190379));
#50146=CARTESIAN_POINT('Ctrl Pts',(-66.61031715335,0.855689028738441,3.71450372426576));
#50147=CARTESIAN_POINT('Ctrl Pts',(-66.4248447414253,-2.42529080533395,
2.79441164195831));
#50148=CARTESIAN_POINT('Ctrl Pts',(-66.305663506733,-3.21581548081763,0.852944897003651));
#50149=CARTESIAN_POINT('Ctrl Pts',(-66.2527734492732,-3.22375014837333,
-0.00289065711299982));
#50150=CARTESIAN_POINT('Ctrl Pts',(-67.256226550727,-3.22427826197944,-0.00280124290513738));
#50151=CARTESIAN_POINT('Ctrl Pts',(-67.2439022717311,-3.22610275259481,
-0.202141319110646));
#50152=CARTESIAN_POINT('Ctrl Pts',(-67.1652868155028,-3.11834622337749,
-1.4717463453671));
#50153=CARTESIAN_POINT('Ctrl Pts',(-67.0203801820419,-1.43262347679405,
-3.53232665607612));
#50154=CARTESIAN_POINT('Ctrl Pts',(-66.8215066503446,2.19720248236392,-3.11481024831069));
#50155=CARTESIAN_POINT('Ctrl Pts',(-66.6226331186469,3.80823428927037,0.164600211157061));
#50156=CARTESIAN_POINT('Ctrl Pts',(-66.4237595869497,1.92025261185217,3.29277565864461));
#50157=CARTESIAN_POINT('Ctrl Pts',(-66.2248860552521,-1.73206110813779,
3.39554207000353));
#50158=CARTESIAN_POINT('Ctrl Pts',(-66.0857083765112,-3.17433560462667,
1.28410951244796));
#50159=CARTESIAN_POINT('Ctrl Pts',(-66.0128218750029,-3.22749422431154,
0.108301395119127));
#50160=CARTESIAN_POINT('Ctrl Pts',(-66.0062265507269,-3.22676995476309,
0.00183908904011598));
#50161=CARTESIAN_POINT('Origin',(-111.877773449273,0.,0.));
#50162=CARTESIAN_POINT('',(-68.7527734492732,-3.22293282582728,0.00296792478262312));
#50163=CARTESIAN_POINT('',(-68.5062265507269,-3.21747859664537,-0.000509701883559255));
#50164=CARTESIAN_POINT('',(-111.877773449273,-3.22275,5.46201577318104E-12));
#50165=CARTESIAN_POINT('Ctrl Pts',(-68.7527734492732,-3.22293282582728,
0.00296792478262326));
#50166=CARTESIAN_POINT('Ctrl Pts',(-68.701533122957,-3.21523694329641,-0.826711997340943));
#50167=CARTESIAN_POINT('Ctrl Pts',(-68.5840016194083,-2.4650798738634,-2.74212576371246));
#50168=CARTESIAN_POINT('Ctrl Pts',(-68.4001789386271,0.76302674318989,-3.73463944988864));
#50169=CARTESIAN_POINT('Ctrl Pts',(-68.2013054069296,3.55437052989495,-1.37702279127899));
#50170=CARTESIAN_POINT('Ctrl Pts',(-68.0024318752321,3.07995137564101,2.24580523536093));
#50171=CARTESIAN_POINT('Ctrl Pts',(-67.8035583435348,-0.224333426531556,
3.80518280050091));
#50172=CARTESIAN_POINT('Ctrl Pts',(-67.6370055348817,-2.81898931674464,
2.18312258522133));
#50173=CARTESIAN_POINT('Ctrl Pts',(-67.5367439034612,-3.21708156072468,
0.552207010145866));
#50174=CARTESIAN_POINT('Ctrl Pts',(-67.5027734492732,-3.21741959772868,
-0.000221941790679026));
#50175=CARTESIAN_POINT('Ctrl Pts',(-68.5062265507269,-3.21747859664537,
-0.000509701883559047));
#50176=CARTESIAN_POINT('Ctrl Pts',(-68.4749826684593,-3.2181933316529,-0.508575802308148));
#50177=CARTESIAN_POINT('Ctrl Pts',(-68.3774476089592,-2.86499356994955,
-2.09368301619967));
#50178=CARTESIAN_POINT('Ctrl Pts',(-68.2136213722266,-0.380552649142222,
-3.79274588032446));
#50179=CARTESIAN_POINT('Ctrl Pts',(-68.0147478405293,2.98503648681207,-2.37050602274877));
#50180=CARTESIAN_POINT('Ctrl Pts',(-67.8158743088317,3.6079679695899,1.22975963582352));
#50181=CARTESIAN_POINT('Ctrl Pts',(-67.6170007771343,0.915891073766863,
3.70011961596942));
#50182=CARTESIAN_POINT('Ctrl Pts',(-67.4304515244327,-2.39872972824626,
2.82839230532065));
#50183=CARTESIAN_POINT('Ctrl Pts',(-67.3101934489636,-3.21628898330386,
0.8700908435767));
#50184=CARTESIAN_POINT('Ctrl Pts',(-67.256226550727,-3.22427826197944,-0.00280124290513738));
#50185=CARTESIAN_POINT('Origin',(-111.877773449273,0.,0.));
#50186=CARTESIAN_POINT('',(-70.0027734492732,-3.22759001795114,-0.00114057037762329));
#50187=CARTESIAN_POINT('',(-69.7562265507269,-3.22240161101842,0.00297936229024562));
#50188=CARTESIAN_POINT('',(-111.877773449273,-3.22275,5.46201577318104E-12));
#50189=CARTESIAN_POINT('Ctrl Pts',(-70.0027734492732,-3.22759001795114,
-0.00114057037762324));
#50190=CARTESIAN_POINT('Ctrl Pts',(-69.9989046969177,-3.22787455754374,
-0.0635483535897433));
#50191=CARTESIAN_POINT('Ctrl Pts',(-69.9287447673297,-3.19790422336463,
-1.19503652969521));
#50192=CARTESIAN_POINT('Ctrl Pts',(-69.7922936605092,-1.8701681655698,-3.32147748208183));
#50193=CARTESIAN_POINT('Ctrl Pts',(-69.5934201288118,1.78328299053953,-3.36892318213695));
#50194=CARTESIAN_POINT('Ctrl Pts',(-69.3945465971144,3.79825007337514,-0.320995345127123));
#50195=CARTESIAN_POINT('Ctrl Pts',(-69.1956730654169,2.32337718995098,3.02186367407648));
#50196=CARTESIAN_POINT('Ctrl Pts',(-68.9967995337195,-1.2862194261268,3.58822814482881));
#50197=CARTESIAN_POINT('Ctrl Pts',(-68.8491663283382,-3.0885014647762,1.56124403622359));
#50198=CARTESIAN_POINT('Ctrl Pts',(-68.7678243001894,-3.22519334188891,
0.246670291918771));
#50199=CARTESIAN_POINT('Ctrl Pts',(-68.7527734492732,-3.22293282582728,
0.00296792478262326));
#50200=CARTESIAN_POINT('Ctrl Pts',(-69.7562265507269,-3.22240161101842,
0.00297936229024551));
#50201=CARTESIAN_POINT('Ctrl Pts',(-69.7060630651875,-3.21495053399222,
-0.809606534766093));
#50202=CARTESIAN_POINT('Ctrl Pts',(-69.5896084024157,-2.49046711360947,
-2.70785758711506));
#50203=CARTESIAN_POINT('Ctrl Pts',(-69.4068625624114,0.702284330303311,
-3.74653684766316));
#50204=CARTESIAN_POINT('Ctrl Pts',(-69.2079890307139,3.53154229168029,-1.43455591510438));
#50205=CARTESIAN_POINT('Ctrl Pts',(-69.0091154990165,3.11601194424255,2.19549793778661));
#50206=CARTESIAN_POINT('Ctrl Pts',(-68.810241967319,-0.162516575587105,
3.8083237774836));
#50207=CARTESIAN_POINT('Ctrl Pts',(-68.6426123178892,-2.80011258075798,
2.21839497315072));
#50208=CARTESIAN_POINT('Ctrl Pts',(-68.5412738456918,-3.21667685477425,
0.569404828286875));
#50209=CARTESIAN_POINT('Ctrl Pts',(-68.5062265507269,-3.21747859664537,
-0.000509701883559047));
#50210=CARTESIAN_POINT('Origin',(-111.877773449273,0.,0.));
#50211=CARTESIAN_POINT('',(-71.2527734492732,-3.21945012312131,-0.00240714690090972));
#50212=CARTESIAN_POINT('',(-71.0062265507269,-3.22781546179181,-0.00083510151203281));
#50213=CARTESIAN_POINT('',(-111.877773449273,-3.22275,5.46201577318104E-12));
#50214=CARTESIAN_POINT('Ctrl Pts',(-71.2527734492732,-3.21945012312131,
-0.00240714690090973));
#50215=CARTESIAN_POINT('Ctrl Pts',(-71.2299850936459,-3.22200381206688,
-0.372407551372853));
#50216=CARTESIAN_POINT('Ctrl Pts',(-71.1409055607861,-2.99193409339074,
-1.81565804682397));
#50217=CARTESIAN_POINT('Ctrl Pts',(-70.9855348506941,-0.859753171502819,
-3.71356514896109));
#50218=CARTESIAN_POINT('Ctrl Pts',(-70.7866613189964,2.65936797721959,-2.73084301878126));
#50219=CARTESIAN_POINT('Ctrl Pts',(-70.5877877872991,3.73505636806534,0.760983284219782));
#50220=CARTESIAN_POINT('Ctrl Pts',(-70.3889142556016,1.37896729884392,3.55361658317363));
#50221=CARTESIAN_POINT('Ctrl Pts',(-70.1939094762596,-2.17363864940172,
3.09037013995876));
#50222=CARTESIAN_POINT('Ctrl Pts',(-70.0651958741502,-3.22299896385633,
1.00581071554859));
#50223=CARTESIAN_POINT('Ctrl Pts',(-70.0027734492732,-3.22759001795114,
-0.00114057037762324));
#50224=CARTESIAN_POINT('Ctrl Pts',(-71.0062265507269,-3.22781546179181,
-0.000835101512032888));
#50225=CARTESIAN_POINT('Ctrl Pts',(-71.0034346391483,-3.22797109666668,
-0.0458637190486939));
#50226=CARTESIAN_POINT('Ctrl Pts',(-70.9343515503372,-3.20668289731449,
-1.15990179856474));
#50227=CARTESIAN_POINT('Ctrl Pts',(-70.7989772842935,-1.92385463457588,
-3.29067242011544));
#50228=CARTESIAN_POINT('Ctrl Pts',(-70.6001037525962,1.72834444495199,-3.39743537261432));
#50229=CARTESIAN_POINT('Ctrl Pts',(-70.4012302208986,3.79253709969573,-0.382627728894362));
#50230=CARTESIAN_POINT('Ctrl Pts',(-70.2023566892013,2.3721388801267,2.98373905777277));
#50231=CARTESIAN_POINT('Ctrl Pts',(-70.0034831575037,-1.22778541315046,
3.60864027172874));
#50232=CARTESIAN_POINT('Ctrl Pts',(-69.8547731113456,-3.07612755899721,
1.59661877607581));
#50233=CARTESIAN_POINT('Ctrl Pts',(-69.77235424242,-3.22479715175424,0.264227851724424));
#50234=CARTESIAN_POINT('Ctrl Pts',(-69.7562265507269,-3.22240161101842,
0.00297936229024551));
#50235=CARTESIAN_POINT('Origin',(-111.877773449273,0.,0.));
#50236=CARTESIAN_POINT('',(-72.5027734492732,-3.21882799635161,0.00208781935145901));
#50237=CARTESIAN_POINT('',(-72.2562265507269,-3.21986660597496,-0.00256872119734103));
#50238=CARTESIAN_POINT('',(-111.877773449273,-3.22275,5.46201577318104E-12));
#50239=CARTESIAN_POINT('Ctrl Pts',(-72.5027734492732,-3.21882799635161,
0.00208781935145931));
#50240=CARTESIAN_POINT('Ctrl Pts',(-72.4610654903742,-3.2148231872832,-0.675427126265385));
#50241=CARTESIAN_POINT('Ctrl Pts',(-72.3530663542426,-2.67416790804054,
-2.43563871880424));
#50242=CARTESIAN_POINT('Ctrl Pts',(-72.1787760408787,0.220169410119124,
-3.80542600274073));
#50243=CARTESIAN_POINT('Ctrl Pts',(-71.9799025091812,3.3204537540748,-1.87198517583289));
#50244=CARTESIAN_POINT('Ctrl Pts',(-71.7810289774838,3.36989837098991,1.78143947432599));
#50245=CARTESIAN_POINT('Ctrl Pts',(-71.5821554457863,0.323073445319674,
3.79807387769336));
#50246=CARTESIAN_POINT('Ctrl Pts',(-71.4060702697162,-2.63745085413309,
2.49382211291307));
#50247=CARTESIAN_POINT('Ctrl Pts',(-71.2962762708784,-3.21457514765352,
0.70392120135233));
#50248=CARTESIAN_POINT('Ctrl Pts',(-71.2527734492732,-3.21945012312131,
-0.00240714690090973));
#50249=CARTESIAN_POINT('Ctrl Pts',(-72.2562265507269,-3.21986660597496,
-0.00256872119734103));
#50250=CARTESIAN_POINT('Ctrl Pts',(-72.2345150358765,-3.22248512237309,
-0.354970389721529));
#50251=CARTESIAN_POINT('Ctrl Pts',(-72.1465123437936,-3.00645953474252,
-1.780228858952));
#50252=CARTESIAN_POINT('Ctrl Pts',(-71.9922184744782,-0.919939440447408,
-3.69911517222657));
#50253=CARTESIAN_POINT('Ctrl Pts',(-71.7933449427809,2.61467485947912,-2.77366490598547));
#50254=CARTESIAN_POINT('Ctrl Pts',(-71.5944714110833,3.74692052987602,0.700234370965129));
#50255=CARTESIAN_POINT('Ctrl Pts',(-71.3955978793859,1.43648792397377,3.53075687010093));
#50256=CARTESIAN_POINT('Ctrl Pts',(-71.1995162592671,-2.14282857537852,
3.12301830014379));
#50257=CARTESIAN_POINT('Ctrl Pts',(-71.0697258163808,-3.2242757005974,1.02329623877626));
#50258=CARTESIAN_POINT('Ctrl Pts',(-71.0062265507269,-3.22781546179181,
-0.000835101512032888));
#50259=CARTESIAN_POINT('Origin',(-111.877773449273,0.,0.));
#50260=CARTESIAN_POINT('',(-73.7527734492733,-3.22708613677034,0.00161448296875132));
#50261=CARTESIAN_POINT('',(-73.5062265507269,-3.21850254177831,0.00186944240760517));
#50262=CARTESIAN_POINT('',(-111.877773449273,-3.22275,5.46201577318104E-12));
#50263=CARTESIAN_POINT('Ctrl Pts',(-73.7527734492733,-3.22708613677034,
0.00161448296875113));
#50264=CARTESIAN_POINT('Ctrl Pts',(-73.6921458871025,-3.22109534309337,
-0.976788199942429));
#50265=CARTESIAN_POINT('Ctrl Pts',(-73.565227147699,-2.22390442281198,-3.03556114541307));
#50266=CARTESIAN_POINT('Ctrl Pts',(-73.3720172310635,1.28229218005324,-3.5896334626897));
#50267=CARTESIAN_POINT('Ctrl Pts',(-73.1731436993659,3.71309419372906,-0.861784857132571));
#50268=CARTESIAN_POINT('Ctrl Pts',(-72.9742701676686,2.73229763821218,2.65787344463722));
#50269=CARTESIAN_POINT('Ctrl Pts',(-72.7753966359709,-0.758939597445834,
3.73547216813566));
#50270=CARTESIAN_POINT('Ctrl Pts',(-72.6182310631726,-2.96691742054202,
1.87471226882313));
#50271=CARTESIAN_POINT('Ctrl Pts',(-72.5273566676067,-3.22118848337403,
0.401424019730246));
#50272=CARTESIAN_POINT('Ctrl Pts',(-72.5027734492732,-3.21882799635161,
0.00208781935145931));
#50273=CARTESIAN_POINT('Ctrl Pts',(-73.5062265507269,-3.21850254177831,
0.00186944240760538));
#50274=CARTESIAN_POINT('Ctrl Pts',(-73.4655954326047,-3.21503052406492,
-0.658320259377352));
#50275=CARTESIAN_POINT('Ctrl Pts',(-73.3586731372501,-2.69562174110393,
-2.40064775943804));
#50276=CARTESIAN_POINT('Ctrl Pts',(-73.185459664663,0.158349159120692,-3.80849933376564));
#50277=CARTESIAN_POINT('Ctrl Pts',(-72.9865861329655,3.28961932307638,-1.92565478233509));
#50278=CARTESIAN_POINT('Ctrl Pts',(-72.7877126012682,3.39838049850435,1.72648533699904));
#50279=CARTESIAN_POINT('Ctrl Pts',(-72.5888390695705,0.384702694105128,
3.79232718375349));
#50280=CARTESIAN_POINT('Ctrl Pts',(-72.4116770527236,-2.61484136747631,
2.52863830808241));
#50281=CARTESIAN_POINT('Ctrl Pts',(-72.300806213109,-3.21449007753948,0.721008031228958));
#50282=CARTESIAN_POINT('Ctrl Pts',(-72.2562265507269,-3.21986660597496,
-0.00256872119734103));
#50283=CARTESIAN_POINT('Origin',(-111.877773449273,0.,0.));
#50284=CARTESIAN_POINT('',(-75.0027734492731,-3.22382174436618,-0.00288039460979974));
#50285=CARTESIAN_POINT('',(-74.7562265507269,-3.22671773329219,0.00187259391569501));
#50286=CARTESIAN_POINT('',(-111.877773449273,-3.22275,5.46201577318104E-12));
#50287=CARTESIAN_POINT('Ctrl Pts',(-75.0027734492731,-3.22382174436618,
-0.00288039460980015));
#50288=CARTESIAN_POINT('Ctrl Pts',(-74.9895174610631,-3.2258080640962,-0.217368688148813));
#50289=CARTESIAN_POINT('Ctrl Pts',(-74.9099702956205,-3.10838512112799,
-1.50231655289377));
#50290=CARTESIAN_POINT('Ctrl Pts',(-74.7641319529457,-1.38285507499101,
-3.55210549858237));
#50291=CARTESIAN_POINT('Ctrl Pts',(-74.5652584212481,2.24074678227322,-3.08363348814666));
#50292=CARTESIAN_POINT('Ctrl Pts',(-74.3663848895507,3.80554589512093,0.218087302738192));
#50293=CARTESIAN_POINT('Ctrl Pts',(-74.1675113578533,1.87380162570858,3.31942903207455));
#50294=CARTESIAN_POINT('Ctrl Pts',(-73.9686378261556,-1.77959542483032,
3.37087255104825));
#50295=CARTESIAN_POINT('Ctrl Pts',(-73.8303918566292,-3.18260764459991,
1.25365432148051));
#50296=CARTESIAN_POINT('Ctrl Pts',(-73.758437064335,-3.22764577578741,0.0930134436550926));
#50297=CARTESIAN_POINT('Ctrl Pts',(-73.7527734492733,-3.22708613677034,
0.00161448296875113));
#50298=CARTESIAN_POINT('Ctrl Pts',(-74.7562265507269,-3.22671773329219,
0.00187259391569496));
#50299=CARTESIAN_POINT('Ctrl Pts',(-74.696675829333,-3.22008363392945,-0.959441334008879));
#50300=CARTESIAN_POINT('Ctrl Pts',(-74.5708339307065,-2.2534128417743,-3.00245490988977));
#50301=CARTESIAN_POINT('Ctrl Pts',(-74.3787008548478,1.22383586576573,-3.60998163501602));
#50302=CARTESIAN_POINT('Ctrl Pts',(-74.1798273231502,3.69861128925905,-0.921963211008446));
#50303=CARTESIAN_POINT('Ctrl Pts',(-73.9809537914529,2.77509506592403,2.61315690431547));
#50304=CARTESIAN_POINT('Ctrl Pts',(-73.7820802597554,-0.698184202008545,
3.74730309043091));
#50305=CARTESIAN_POINT('Ctrl Pts',(-73.6238378461801,-2.95141859444466,
1.910138997005));
#50306=CARTESIAN_POINT('Ctrl Pts',(-73.5318866098372,-3.22069524982759,
0.418803741899784));
#50307=CARTESIAN_POINT('Ctrl Pts',(-73.5062265507269,-3.21850254177831,
0.00186944240760538));
#50308=CARTESIAN_POINT('Origin',(-111.877773449273,0.,0.));
#50309=CARTESIAN_POINT('',(-76.2527734492732,-3.21742483922095,-0.000260901863258924));
#50310=CARTESIAN_POINT('',(-76.0062265507269,-3.22434875022485,-0.00278685721651517));
#50311=CARTESIAN_POINT('',(-111.877773449273,-3.22275,5.46201577318104E-12));
#50312=CARTESIAN_POINT('Ctrl Pts',(-76.2527734492732,-3.21742483922095,
-0.000260901863258847));
#50313=CARTESIAN_POINT('Ctrl Pts',(-76.2205978577914,-3.21780125389046,
-0.523499596499799));
#50314=CARTESIAN_POINT('Ctrl Pts',(-76.122131089077,-2.84955967489057,-2.1242643517588));
#50315=CARTESIAN_POINT('Ctrl Pts',(-75.9573731431304,-0.327229354942119,
-3.79771807547001));
#50316=CARTESIAN_POINT('Ctrl Pts',(-75.7584996114328,3.01804601534794,-2.32833414284333));
#50317=CARTESIAN_POINT('Ctrl Pts',(-75.5596260797355,3.59033450986518,1.28032798093242));
#50318=CARTESIAN_POINT('Ctrl Pts',(-75.3607525480379,0.863816284783001,
3.71262212696513));
#50319=CARTESIAN_POINT('Ctrl Pts',(-75.1751350045506,-2.42173826724886,
2.79899842446453));
#50320=CARTESIAN_POINT('Ctrl Pts',(-75.0558086382956,-3.21587478178058,
0.855254586403673));
#50321=CARTESIAN_POINT('Ctrl Pts',(-75.0027734492731,-3.22382174436618,
-0.00288039460980015));
#50322=CARTESIAN_POINT('Ctrl Pts',(-76.0062265507269,-3.22434875022485,
-0.00278685721651517));
#50323=CARTESIAN_POINT('Ctrl Pts',(-75.9940474032937,-3.22614707084526,
-0.199768380540557));
#50324=CARTESIAN_POINT('Ctrl Pts',(-75.915577078628,-3.11987589874836,-1.4669856933204));
#50325=CARTESIAN_POINT('Ctrl Pts',(-75.77081557673,-1.4403506510764,-3.52918285633249));
#50326=CARTESIAN_POINT('Ctrl Pts',(-75.5719420450324,2.19038036270197,-3.1196114338451));
#50327=CARTESIAN_POINT('Ctrl Pts',(-75.373068513335,3.80858540178188,0.156265379471771));
#50328=CARTESIAN_POINT('Ctrl Pts',(-75.1741949816376,1.92745435364065,3.28856524127456));
#50329=CARTESIAN_POINT('Ctrl Pts',(-74.9753214499401,-1.72462571221478,
3.39932460707347));
#50330=CARTESIAN_POINT('Ctrl Pts',(-74.8359986396366,-3.17302647816718,
1.28885510720927));
#50331=CARTESIAN_POINT('Ctrl Pts',(-74.7629670065655,-3.22746863693763,
0.110682259466689));
#50332=CARTESIAN_POINT('Ctrl Pts',(-74.7562265507269,-3.22671773329219,
0.00187259391569496));
#50333=CARTESIAN_POINT('Origin',(-111.877773449273,0.,0.));
#50334=CARTESIAN_POINT('',(-77.5027734492732,-3.22286096438354,0.00297125643594199));
#50335=CARTESIAN_POINT('',(-77.2562265507269,-3.2174900915274,-0.00054818518968075));
#50336=CARTESIAN_POINT('',(-111.877773449273,-3.22275,5.46201577318104E-12));
#50337=CARTESIAN_POINT('Ctrl Pts',(-77.5027734492732,-3.22286096438354,
0.00297125643594204));
#50338=CARTESIAN_POINT('Ctrl Pts',(-77.4516782545196,-3.21519424277418,
-0.824405892672294));
#50339=CARTESIAN_POINT('Ctrl Pts',(-77.3342918825336,-2.46852826513399,
-2.73751347857648));
#50340=CARTESIAN_POINT('Ctrl Pts',(-77.150614333315,0.754851542933501,-3.73630041345961));
#50341=CARTESIAN_POINT('Ctrl Pts',(-76.9517408016175,3.55134836116475,-1.38479834240944));
#50342=CARTESIAN_POINT('Ctrl Pts',(-76.7528672699202,3.08485901327164,2.23905928901498));
#50343=CARTESIAN_POINT('Ctrl Pts',(-76.5539937382226,-0.216005130071836,
3.80566464829338));
#50344=CARTESIAN_POINT('Ctrl Pts',(-76.3872957980071,-2.81646876630082,
2.18787831468303));
#50345=CARTESIAN_POINT('Ctrl Pts',(-76.2868890350239,-3.21702572901523,
0.554525932903884));
#50346=CARTESIAN_POINT('Ctrl Pts',(-76.2527734492732,-3.21742483922095,
-0.000260901863258847));
#50347=CARTESIAN_POINT('Ctrl Pts',(-77.2562265507269,-3.2174900915274,-0.000548185189681097));
#50348=CARTESIAN_POINT('Ctrl Pts',(-77.225127800022,-3.21825537090246,-0.506249753593985));
#50349=CARTESIAN_POINT('Ctrl Pts',(-77.1277378720846,-2.86737116326948,
-2.08891786712429));
#50350=CARTESIAN_POINT('Ctrl Pts',(-76.9640567669146,-0.388852278417899,
-3.79190394618015));
#50351=CARTESIAN_POINT('Ctrl Pts',(-76.7651832352172,2.9798414130333,-2.37703318964188));
#50352=CARTESIAN_POINT('Ctrl Pts',(-76.5663097035197,3.61065069576294,1.22186054223637));
#50353=CARTESIAN_POINT('Ctrl Pts',(-76.3674361718222,0.923986705575531,
3.69810629909514));
#50354=CARTESIAN_POINT('Ctrl Pts',(-76.1807417875581,-2.39511414671302,
2.83296268424476));
#50355=CARTESIAN_POINT('Ctrl Pts',(-76.0603385805262,-3.21635880022759,
0.872403308475266));
#50356=CARTESIAN_POINT('Ctrl Pts',(-76.0062265507269,-3.22434875022485,
-0.00278685721651517));
#50357=CARTESIAN_POINT('Origin',(-111.877773449273,0.,0.));
#50358=CARTESIAN_POINT('',(-78.7527734492732,-3.2276239969737,-0.00110020614287963));
#50359=CARTESIAN_POINT('',(-78.5062265507269,-3.22233048953625,0.00297856531753751));
#50360=CARTESIAN_POINT('',(-111.877773449273,-3.22275,5.46201577318104E-12));
#50361=CARTESIAN_POINT('Ctrl Pts',(-78.7527734492731,-3.2276239969737,-0.00110020614287983));
#50362=CARTESIAN_POINT('Ctrl Pts',(-78.7490498284803,-3.22788936443132,
-0.0611651541018486));
#50363=CARTESIAN_POINT('Ctrl Pts',(-78.679035030455,-3.19910469106636,-1.19029975791683));
#50364=CARTESIAN_POINT('Ctrl Pts',(-78.5427290551972,-1.87743284212275,
-3.31737660732185));
#50365=CARTESIAN_POINT('Ctrl Pts',(-78.3438555234997,1.77590572820074,-3.3728178836147));
#50366=CARTESIAN_POINT('Ctrl Pts',(-78.1449819918024,3.79753846903493,-0.329307163127962));
#50367=CARTESIAN_POINT('Ctrl Pts',(-77.9461084601048,2.32998506713825,3.01677165499815));
#50368=CARTESIAN_POINT('Ctrl Pts',(-77.7472349284074,-1.27836339853949,
3.59103448225746));
#50369=CARTESIAN_POINT('Ctrl Pts',(-77.5994565914635,-3.08685333698085,
1.56601082283768));
#50370=CARTESIAN_POINT('Ctrl Pts',(-77.5179694317521,-3.22514108813702,
0.24903761790008));
#50371=CARTESIAN_POINT('Ctrl Pts',(-77.5027734492732,-3.22286096438354,
0.00297125643594204));
#50372=CARTESIAN_POINT('Ctrl Pts',(-78.5062265507269,-3.22233048953625,
0.00297856531753734));
#50373=CARTESIAN_POINT('Ctrl Pts',(-78.4562081967502,-3.21491722942411,
-0.807301991740865));
#50374=CARTESIAN_POINT('Ctrl Pts',(-78.339898665541,-2.49385359742783,-2.70323107546322));
#50375=CARTESIAN_POINT('Ctrl Pts',(-78.1572979570994,0.694083237695167,
-3.74806484610899));
#50376=CARTESIAN_POINT('Ctrl Pts',(-77.9584244254018,3.52839426461459,-1.44228136815333));
#50377=CARTESIAN_POINT('Ctrl Pts',(-77.7595508937045,3.12080939645103,2.18867319225837));
#50378=CARTESIAN_POINT('Ctrl Pts',(-77.560677362007,-0.154181553044083,
3.80867032968048));
#50379=CARTESIAN_POINT('Ctrl Pts',(-77.3929025810144,-2.79753745286427,
2.22314625409605));
#50380=CARTESIAN_POINT('Ctrl Pts',(-77.2914189772544,-3.21662407480424,
0.571721275400419));
#50381=CARTESIAN_POINT('Ctrl Pts',(-77.2562265507269,-3.2174900915274,-0.000548185189681097));
#50382=CARTESIAN_POINT('Origin',(-111.877773449273,0.,0.));
#50383=CARTESIAN_POINT('',(-80.0027734492731,-3.21950446961254,-0.00243030051328978));
#50384=CARTESIAN_POINT('',(-79.7562265507269,-3.2278409596885,-0.000792969578133351));
#50385=CARTESIAN_POINT('',(-111.877773449273,-3.22275,5.46201577318104E-12));
#50386=CARTESIAN_POINT('Ctrl Pts',(-80.0027734492731,-3.21950446961254,
-0.00243030051328971));
#50387=CARTESIAN_POINT('Ctrl Pts',(-79.9801302252086,-3.22206910334583,
-0.370058688680998));
#50388=CARTESIAN_POINT('Ctrl Pts',(-79.8911958239115,-2.99391276895397,
-1.81088294607542));
#50389=CARTESIAN_POINT('Ctrl Pts',(-79.7359702453819,-0.867878363713628,
-3.71167465940716));
#50390=CARTESIAN_POINT('Ctrl Pts',(-79.5370967136845,2.65338507480061,-2.73665658720871));
#50391=CARTESIAN_POINT('Ctrl Pts',(-79.338223181987,3.73671285846524,0.752807176418981));
#50392=CARTESIAN_POINT('Ctrl Pts',(-79.1393496502896,1.38674119528204,3.55059016063458));
#50393=CARTESIAN_POINT('Ctrl Pts',(-78.944199739385,-2.16951483572038,3.09478083178531));
#50394=CARTESIAN_POINT('Ctrl Pts',(-78.8153410057128,-3.2231650592069,1.00816395649729));
#50395=CARTESIAN_POINT('Ctrl Pts',(-78.7527734492731,-3.2276239969737,-0.00110020614287983));
#50396=CARTESIAN_POINT('Ctrl Pts',(-79.7562265507269,-3.2278409596885,-0.00079296957813336));
#50397=CARTESIAN_POINT('Ctrl Pts',(-79.7535797707109,-3.22798174349532,
-0.0434799691742248));
#50398=CARTESIAN_POINT('Ctrl Pts',(-79.6846418134625,-3.2078434111715,-1.15516845035792));
#50399=CARTESIAN_POINT('Ctrl Pts',(-79.5494126789815,-1.9310517647361,-3.28645412464514));
#50400=CARTESIAN_POINT('Ctrl Pts',(-79.3505391472841,1.72090491437897,-3.40120977111878));
#50401=CARTESIAN_POINT('Ctrl Pts',(-79.1516656155866,3.79169062467575,-0.39092689627776));
#50402=CARTESIAN_POINT('Ctrl Pts',(-78.9527920838892,2.37866320364617,2.9785404135427));
#50403=CARTESIAN_POINT('Ctrl Pts',(-78.7539185521916,-1.21988485293742,
3.61131867564487));
#50404=CARTESIAN_POINT('Ctrl Pts',(-78.605063374471,-3.07443410069902,1.60138749919574));
#50405=CARTESIAN_POINT('Ctrl Pts',(-78.5224993739827,-3.22474229764194,
0.266592843763458));
#50406=CARTESIAN_POINT('Ctrl Pts',(-78.5062265507269,-3.22233048953625,
0.00297856531753734));
#50407=CARTESIAN_POINT('Origin',(-111.877773449273,0.,0.));
#50408=CARTESIAN_POINT('',(-81.2527734492731,-3.21878195259031,0.00205948639376733));
#50409=CARTESIAN_POINT('',(-81.0062265507269,-3.21992499686852,-0.002588646514457));
#50410=CARTESIAN_POINT('',(-111.877773449273,-3.22275,5.46201577318104E-12));
#50411=CARTESIAN_POINT('Ctrl Pts',(-81.2527734492731,-3.21878195259031,
0.00205948639376698));
#50412=CARTESIAN_POINT('Ctrl Pts',(-81.2112106219368,-3.21484868389951,
-0.673122117896321));
#50413=CARTESIAN_POINT('Ctrl Pts',(-81.1033566173679,-2.6770843609167,-2.43092628129503));
#50414=CARTESIAN_POINT('Ctrl Pts',(-80.9292114355667,0.211840591375986,
-3.8058987368732));
#50415=CARTESIAN_POINT('Ctrl Pts',(-80.7303379038692,3.31634890518381,-1.87924760757427));
#50416=CARTESIAN_POINT('Ctrl Pts',(-80.5314643721718,3.3737890355405,1.77406008217146));
#50417=CARTESIAN_POINT('Ctrl Pts',(-80.3325908404742,0.331384872734104,
3.79735772578913));
#50418=CARTESIAN_POINT('Ctrl Pts',(-80.1563605328414,-2.63442917895774,
2.49851864517239));
#50419=CARTESIAN_POINT('Ctrl Pts',(-80.046421402441,-3.2145607825844,0.706224377997202));
#50420=CARTESIAN_POINT('Ctrl Pts',(-80.0027734492731,-3.21950446961254,
-0.00243030051328971));
#50421=CARTESIAN_POINT('Ctrl Pts',(-81.0062265507269,-3.21992499686852,
-0.0025886465144568));
#50422=CARTESIAN_POINT('Ctrl Pts',(-80.9846601674391,-3.22254938084776,
-0.352618678648645));
#50423=CARTESIAN_POINT('Ctrl Pts',(-80.8968026069189,-3.00838975708643,
-1.77545409631581));
#50424=CARTESIAN_POINT('Ctrl Pts',(-80.7426538691663,-0.92803286430498,
-3.69709299778318));
#50425=CARTESIAN_POINT('Ctrl Pts',(-80.5437803374688,2.60859834707974,-2.77938055960323));
#50426=CARTESIAN_POINT('Ctrl Pts',(-80.3449068057714,3.74844404100414,0.692032443566012));
#50427=CARTESIAN_POINT('Ctrl Pts',(-80.1460332740739,1.44421165347667,3.52760461665555));
#50428=CARTESIAN_POINT('Ctrl Pts',(-79.9498065223924,-2.13863853957505,
3.1274044744303));
#50429=CARTESIAN_POINT('Ctrl Pts',(-79.8198709479434,-3.22445567626158,
1.0256574123546));
#50430=CARTESIAN_POINT('Ctrl Pts',(-79.7562265507269,-3.2278409596885,-0.00079296957813336));
#50431=CARTESIAN_POINT('Origin',(-111.877773449273,0.,0.));
#50432=CARTESIAN_POINT('',(-82.5027734492731,-3.2270391465412,0.00165051543764288));
#50433=CARTESIAN_POINT('',(-82.2562265507269,-3.21846159883558,0.00183862481499944));
#50434=CARTESIAN_POINT('',(-111.877773449273,-3.22275,5.46201577318104E-12));
#50435=CARTESIAN_POINT('Ctrl Pts',(-82.5027734492731,-3.2270391465412,0.00165051543764267));
#50436=CARTESIAN_POINT('Ctrl Pts',(-82.4422910186651,-3.22095338202291,
-0.974447575458847));
#50437=CARTESIAN_POINT('Ctrl Pts',(-82.3155174108245,-2.22790971805254,
-3.03110875266732));
#50438=CARTESIAN_POINT('Ctrl Pts',(-82.1224526257514,1.27443308628981,-3.59243120185442));
#50439=CARTESIAN_POINT('Ctrl Pts',(-81.9235790940539,3.71119925889672,-0.86990901377786));
#50440=CARTESIAN_POINT('Ctrl Pts',(-81.7247055623564,2.73810793232568,2.65188736231815));
#50441=CARTESIAN_POINT('Ctrl Pts',(-81.525832030659,-0.750762584548115,
3.73712418486865));
#50442=CARTESIAN_POINT('Ctrl Pts',(-81.368521326298,-2.96485012079678,1.87948715189045));
#50443=CARTESIAN_POINT('Ctrl Pts',(-81.2775017991693,-3.22112210244669,
0.403767647852714));
#50444=CARTESIAN_POINT('Ctrl Pts',(-81.2527734492731,-3.21878195259031,
0.00205948639376698));
#50445=CARTESIAN_POINT('Ctrl Pts',(-82.2562265507268,-3.21846159883558,
0.00183862481499927));
#50446=CARTESIAN_POINT('Ctrl Pts',(-82.2157405641674,-3.21506159653712,
-0.656013876140592));
#50447=CARTESIAN_POINT('Ctrl Pts',(-82.1089634003754,-2.69848048787162,
-2.39592739628771));
#50448=CARTESIAN_POINT('Ctrl Pts',(-81.9358950593511,0.150013762347644,
-3.80883676502338));
#50449=CARTESIAN_POINT('Ctrl Pts',(-81.7370215276534,3.28539709044952,-1.93284960344911));
#50450=CARTESIAN_POINT('Ctrl Pts',(-81.5381479959562,3.40215082603064,1.7190437424413));
#50451=CARTESIAN_POINT('Ctrl Pts',(-81.3392744642585,0.393001397111847,
3.79147616811124));
#50452=CARTESIAN_POINT('Ctrl Pts',(-81.161967315849,-2.61176059653824,2.53332507606297));
#50453=CARTESIAN_POINT('Ctrl Pts',(-81.0509513446717,-3.21448249725523,
0.723310585305127));
#50454=CARTESIAN_POINT('Ctrl Pts',(-81.0062265507269,-3.21992499686852,
-0.0025886465144568));
#50455=CARTESIAN_POINT('Origin',(-111.877773449273,0.,0.));
#50456=CARTESIAN_POINT('',(-83.7527734492731,-3.2238932335569,-0.0028695734350786));
#50457=CARTESIAN_POINT('',(-83.5062265507268,-3.22666475540204,0.00190568230792103));
#50458=CARTESIAN_POINT('',(-111.877773449273,-3.22275,5.46201577318104E-12));
#50459=CARTESIAN_POINT('Ctrl Pts',(-83.7527734492731,-3.2238932335569,-0.00286957343507855));
#50460=CARTESIAN_POINT('Ctrl Pts',(-83.7396625926257,-3.22585510627631,
-0.214997467059213));
#50461=CARTESIAN_POINT('Ctrl Pts',(-83.6602605587458,-3.10995284371994,
-1.49755376714856));
#50462=CARTESIAN_POINT('Ctrl Pts',(-83.5145673476336,-1.39062565506363,
-3.54907057114484));
#50463=CARTESIAN_POINT('Ctrl Pts',(-83.3156938159361,2.23399278962533,-3.08853004637957));
#50464=CARTESIAN_POINT('Ctrl Pts',(-83.1168202842386,3.80601407221043,0.209758226593208));
#50465=CARTESIAN_POINT('Ctrl Pts',(-82.9179467525413,1.88106181046435,3.31532021028137));
#50466=CARTESIAN_POINT('Ctrl Pts',(-82.7190732208437,-1.77221390506902,
3.37475917750697));
#50467=CARTESIAN_POINT('Ctrl Pts',(-82.5806821197544,-3.18133411452089,
1.25839711222566));
#50468=CARTESIAN_POINT('Ctrl Pts',(-82.5085821958975,-3.2276236247731,0.0953952018457218));
#50469=CARTESIAN_POINT('Ctrl Pts',(-82.5027734492731,-3.2270391465412,0.00165051543764267));
#50470=CARTESIAN_POINT('Ctrl Pts',(-83.5062265507268,-3.22666475540204,
0.00190568230792082));
#50471=CARTESIAN_POINT('Ctrl Pts',(-83.4468209608956,-3.21995456564922,
-0.957106822200469));
#50472=CARTESIAN_POINT('Ctrl Pts',(-83.321124193832,-2.25735281108562,-2.99798071119528));
#50473=CARTESIAN_POINT('Ctrl Pts',(-83.1291362495355,1.21593237939653,-3.61265139201427));
#50474=CARTESIAN_POINT('Ctrl Pts',(-82.9302627178384,3.69658468693845,-0.930055527256101));
#50475=CARTESIAN_POINT('Ctrl Pts',(-82.7313891861407,2.78080739402538,2.60707726560248));
#50476=CARTESIAN_POINT('Ctrl Pts',(-82.5325156544434,-0.689981442273743,
3.74882211378524));
#50477=CARTESIAN_POINT('Ctrl Pts',(-82.3741281093054,-2.94930135841404,
1.91491326972369));
#50478=CARTESIAN_POINT('Ctrl Pts',(-82.2820317413998,-3.22062871183087,
0.421144430712464));
#50479=CARTESIAN_POINT('Ctrl Pts',(-82.2562265507268,-3.21846159883558,
0.00183862481499927));
#50480=CARTESIAN_POINT('Origin',(-111.877773449273,0.,0.));
#50481=CARTESIAN_POINT('',(-85.0027734492731,-3.21743092663228,-0.000299818468146348));
#50482=CARTESIAN_POINT('',(-84.756226550727,-3.2244190327258,-0.00277192079580268));
#50483=CARTESIAN_POINT('',(-111.877773449273,-3.22275,5.46201577318104E-12));
#50484=CARTESIAN_POINT('Ctrl Pts',(-85.0027734492731,-3.21743092663228,
-0.000299818468146203));
#50485=CARTESIAN_POINT('Ctrl Pts',(-84.970742989354,-3.21786158184376,-0.521175930689154));
#50486=CARTESIAN_POINT('Ctrl Pts',(-84.8724213522023,-2.85198323582054,
-2.11950188255398));
#50487=CARTESIAN_POINT('Ctrl Pts',(-84.7078085378184,-0.335539993719798,
-3.79699282908225));
#50488=CARTESIAN_POINT('Ctrl Pts',(-84.5089350061207,3.01294315696887,-2.33493365309634));
#50489=CARTESIAN_POINT('Ctrl Pts',(-84.3100614744234,3.59312794864103,1.27246735760964));
#50490=CARTESIAN_POINT('Ctrl Pts',(-84.1111879427259,0.871939403430806,
3.71072274742162));
#50491=CARTESIAN_POINT('Ctrl Pts',(-83.9254252676759,-2.41817725657903,
2.80358304503091));
#50492=CARTESIAN_POINT('Ctrl Pts',(-83.8059537698582,-3.2159354758778,0.857564621780238));
#50493=CARTESIAN_POINT('Ctrl Pts',(-83.7527734492731,-3.2238932335569,-0.00286957343507855));
#50494=CARTESIAN_POINT('Ctrl Pts',(-84.7562265507269,-3.2244190327258,-0.00277192079580251));
#50495=CARTESIAN_POINT('Ctrl Pts',(-84.7441925348564,-3.2261909527838,-0.197395183872092));
#50496=CARTESIAN_POINT('Ctrl Pts',(-84.6658673417535,-3.1213996803745,-1.46222538507072));
#50497=CARTESIAN_POINT('Ctrl Pts',(-84.5212509714179,-1.44807092655128,
-3.52602215295995));
#50498=CARTESIAN_POINT('Ctrl Pts',(-84.3223774397204,2.18354775183615,-3.1243976774634));
#50499=CARTESIAN_POINT('Ctrl Pts',(-84.123503908023,3.80891827241787,0.147929799326536));
#50500=CARTESIAN_POINT('Ctrl Pts',(-83.9246303763255,1.93464686355464,3.28433907275508));
#50501=CARTESIAN_POINT('Ctrl Pts',(-83.7257568446282,-1.71718205589994,
3.40309086249292));
#50502=CARTESIAN_POINT('Ctrl Pts',(-83.5862889027618,-3.17171177674872,
1.29360113283735));
#50503=CARTESIAN_POINT('Ctrl Pts',(-83.5131121381281,-3.22744252056106,
0.113062973018134));
#50504=CARTESIAN_POINT('Ctrl Pts',(-83.5062265507268,-3.22666475540204,
0.00190568230792082));
#50505=CARTESIAN_POINT('Origin',(-111.877773449273,0.,0.));
#50506=CARTESIAN_POINT('',(-86.2527734492731,-3.22278916444396,0.00297402901880627));
#50507=CARTESIAN_POINT('',(-86.0062265507268,-3.217502424002,-0.000586577060036064));
#50508=CARTESIAN_POINT('',(-111.877773449273,-3.22275,5.46201577318104E-12));
#50509=CARTESIAN_POINT('Ctrl Pts',(-86.2527734492731,-3.22278916444396,
0.00297402901880631));
#50510=CARTESIAN_POINT('Ctrl Pts',(-86.2018233860822,-3.21515283337601,
-0.822100023465869));
#50511=CARTESIAN_POINT('Ctrl Pts',(-86.0845821456587,-2.4719682872732,-2.73289922972401));
#50512=CARTESIAN_POINT('Ctrl Pts',(-85.9010497280032,0.746672727185684,
-3.73794348137644));
#50513=CARTESIAN_POINT('Ctrl Pts',(-85.7021761963054,3.54830918264012,-1.3925672608098));
#50514=CARTESIAN_POINT('Ctrl Pts',(-85.5033026646083,3.08975187543889,2.23230261830901));
#50515=CARTESIAN_POINT('Ctrl Pts',(-85.3044291329105,-0.20767579901831,
3.80612826819978));
#50516=CARTESIAN_POINT('Ctrl Pts',(-85.1375860611324,-2.81394089092827,
2.19263347472861));
#50517=CARTESIAN_POINT('Ctrl Pts',(-85.0370341665865,-3.21697028521478,
0.556844514805024));
#50518=CARTESIAN_POINT('Ctrl Pts',(-85.0027734492731,-3.21743092663228,
-0.000299818468146203));
#50519=CARTESIAN_POINT('Ctrl Pts',(-86.0062265507269,-3.217502424002,-0.000586577060035821));
#50520=CARTESIAN_POINT('Ctrl Pts',(-85.9752729315846,-3.2183176510168,-0.503923328628746));
#50521=CARTESIAN_POINT('Ctrl Pts',(-85.8780281352097,-2.86974163214569,
-2.08415233200003));
#50522=CARTESIAN_POINT('Ctrl Pts',(-85.7144921616027,-0.397150045218662,
-3.79104385005903));
#50523=CARTESIAN_POINT('Ctrl Pts',(-85.5156186299052,2.97463206679106,-2.38354897132526));
#50524=CARTESIAN_POINT('Ctrl Pts',(-85.3167450982077,3.61331612810275,1.21395559633781));
#50525=CARTESIAN_POINT('Ctrl Pts',(-85.1178715665104,0.932077911790798,
3.69607526950402));
#50526=CARTESIAN_POINT('Ctrl Pts',(-84.9310320506832,-2.39149003712163,
2.83753078784002));
#50527=CARTESIAN_POINT('Ctrl Pts',(-84.8104837120889,-3.21643006598832,
0.874716184849638));
#50528=CARTESIAN_POINT('Ctrl Pts',(-84.7562265507269,-3.2244190327258,-0.00277192079580251));
#50529=CARTESIAN_POINT('Origin',(-111.877773449273,0.,0.));
#50530=CARTESIAN_POINT('',(-87.5027734492732,-3.22765688580833,-0.00105957506344378));
#50531=CARTESIAN_POINT('',(-87.2562265507268,-3.22225951709131,0.0029772163012047));
#50532=CARTESIAN_POINT('',(-111.877773449273,-3.22275,5.46201577318104E-12));
#50533=CARTESIAN_POINT('Ctrl Pts',(-87.5027734492732,-3.22765688580833,
-0.00105957506344349));
#50534=CARTESIAN_POINT('Ctrl Pts',(-87.499194960043,-3.2279036135337,-0.0587818699554488));
#50535=CARTESIAN_POINT('Ctrl Pts',(-87.4293252935804,-3.20029974928073,
-1.18556344460323));
#50536=CARTESIAN_POINT('Ctrl Pts',(-87.2931644498851,-1.88468852638785,
-3.31325984341546));
#50537=CARTESIAN_POINT('Ctrl Pts',(-87.0942909181878,1.76851995985574,-3.37669643040047));
#50538=CARTESIAN_POINT('Ctrl Pts',(-86.8954173864903,3.79680867573037,-0.337617403855405));
#50539=CARTESIAN_POINT('Ctrl Pts',(-86.6965438547928,2.33658178446086,3.01166518657256));
#50540=CARTESIAN_POINT('Ctrl Pts',(-86.4976703230953,-1.27050124801057,
3.59382361980817));
#50541=CARTESIAN_POINT('Ctrl Pts',(-86.3497468545889,-3.08519912907081,
1.57077788286796));
#50542=CARTESIAN_POINT('Ctrl Pts',(-86.2681145633147,-3.22508847122468,
0.251404636150737));
#50543=CARTESIAN_POINT('Ctrl Pts',(-86.2527734492731,-3.22278916444396,
0.00297402901880631));
#50544=CARTESIAN_POINT('Ctrl Pts',(-87.2562265507268,-3.22225951709131,
0.0029772163012047));
#50545=CARTESIAN_POINT('Ctrl Pts',(-87.2063533283128,-3.21488515861041,
-0.80499762696524));
#50546=CARTESIAN_POINT('Ctrl Pts',(-87.0901889286664,-2.49723177137797,
-2.6986027067367));
#50547=CARTESIAN_POINT('Ctrl Pts',(-86.9077333517873,0.685878820655876,
-3.74957489255291));
#50548=CARTESIAN_POINT('Ctrl Pts',(-86.70885982009,3.52522933769711,-1.44999991314728));
#50549=CARTESIAN_POINT('Ctrl Pts',(-86.5099862883923,3.12559190100552,2.1818379637031));
#50550=CARTESIAN_POINT('Ctrl Pts',(-86.311112756695,-0.145845792021992,
3.80899863959504));
#50551=CARTESIAN_POINT('Ctrl Pts',(-86.1431928441399,-2.79495492899174,
2.22789689550261));
#50552=CARTESIAN_POINT('Ctrl Pts',(-86.0415641088171,-3.21657173696795,
0.574037398758534));
#50553=CARTESIAN_POINT('Ctrl Pts',(-86.0062265507269,-3.217502424002,-0.000586577060035821));
#50554=CARTESIAN_POINT('Origin',(-111.877773449273,0.,0.));
#50555=CARTESIAN_POINT('',(-88.7527734492731,-3.21955938617937,-0.00245303289388847));
#50556=CARTESIAN_POINT('',(-88.5062265507269,-3.22786524494525,-0.00075063836163014));
#50557=CARTESIAN_POINT('',(-111.877773449273,-3.22275,5.46201577318104E-12));
#50558=CARTESIAN_POINT('Ctrl Pts',(-88.7527734492731,-3.21955938617937,
-0.00245303289388835));
#50559=CARTESIAN_POINT('Ctrl Pts',(-88.7302753567712,-3.22213427281091,
-0.367709439234079));
#50560=CARTESIAN_POINT('Ctrl Pts',(-88.6414860870369,-2.99588488351278,
-1.80610787243726));
#50561=CARTESIAN_POINT('Ctrl Pts',(-88.4864056400698,-0.875999399071568,
-3.70976639214839));
#50562=CARTESIAN_POINT('Ctrl Pts',(-88.2875321083726,2.64738946353692,-2.74245704794827));
#50563=CARTESIAN_POINT('Ctrl Pts',(-88.0886585766749,3.73835145123555,0.744627462918542));
#50564=CARTESIAN_POINT('Ctrl Pts',(-87.8897850449776,1.39450844968449,3.54754673193265));
#50565=CARTESIAN_POINT('Ctrl Pts',(-87.6944900025101,-2.16538211451947,
3.09918827690999));
#50566=CARTESIAN_POINT('Ctrl Pts',(-87.5654861372755,-3.22333300557069,
1.01051822704953));
#50567=CARTESIAN_POINT('Ctrl Pts',(-87.5027734492732,-3.22765688580833,
-0.00105957506344349));
#50568=CARTESIAN_POINT('Ctrl Pts',(-88.5062265507269,-3.22786524494525,
-0.000750638361630088));
#50569=CARTESIAN_POINT('Ctrl Pts',(-88.5037249022736,-3.2279918262627,-0.041096158914104));
#50570=CARTESIAN_POINT('Ctrl Pts',(-88.4349320765878,-3.20899857239634,
-1.15043556710435));
#50571=CARTESIAN_POINT('Ctrl Pts',(-88.2998480736696,-1.93823964579142,
-3.28222008813697));
#50572=CARTESIAN_POINT('Ctrl Pts',(-88.1009745419719,1.71345714123552,-3.40496787894343));
#50573=CARTESIAN_POINT('Ctrl Pts',(-87.9021010102748,3.79082598870071,-0.399224191249501));
#50574=CARTESIAN_POINT('Ctrl Pts',(-87.703227478577,2.38517613414864,2.97332750308055));
#50575=CARTESIAN_POINT('Ctrl Pts',(-87.5043539468798,-1.2119784498759,3.61397978252837));
#50576=CARTESIAN_POINT('Ctrl Pts',(-87.3553536375962,-3.07273449438949,
1.60615646661143));
#50577=CARTESIAN_POINT('Ctrl Pts',(-87.2726445055453,-3.22468711006595,
0.268957512522698));
#50578=CARTESIAN_POINT('Ctrl Pts',(-87.2562265507268,-3.22225951709131,
0.0029772163012047));
#50579=CARTESIAN_POINT('Origin',(-111.877773449273,0.,0.));
#50580=CARTESIAN_POINT('',(-90.0027734492731,-3.21873657735583,0.00203080160484108));
#50581=CARTESIAN_POINT('',(-89.7562265507268,-3.21998389906979,-0.00260811917007442));
#50582=CARTESIAN_POINT('',(-111.877773449273,-3.22275,5.46201577318104E-12));
#50583=CARTESIAN_POINT('Ctrl Pts',(-90.0027734492731,-3.21873657735583,
0.00203080160484068));
#50584=CARTESIAN_POINT('Ctrl Pts',(-89.9613557534995,-3.21487495702084,
-0.670816938378399));
#50585=CARTESIAN_POINT('Ctrl Pts',(-89.8536468804933,-2.67999300708434,
-2.42621273871526));
#50586=CARTESIAN_POINT('Ctrl Pts',(-89.6796468302546,0.203510757985896,
-3.80635324199837));
#50587=CARTESIAN_POINT('Ctrl Pts',(-89.4807732985572,3.31222817206875,-1.88650103833566));
#50588=CARTESIAN_POINT('Ctrl Pts',(-89.2818997668597,3.37766354074761,1.76667219285066));
#50589=CARTESIAN_POINT('Ctrl Pts',(-89.0830262351624,0.339694712923688,
3.79662338578627));
#50590=CARTESIAN_POINT('Ctrl Pts',(-88.9066507959666,-2.63139956759911,
2.50321390108784));
#50591=CARTESIAN_POINT('Ctrl Pts',(-88.7965665340037,-3.21454730667008,
0.708527453556772));
#50592=CARTESIAN_POINT('Ctrl Pts',(-88.7527734492731,-3.21955938617937,
-0.00245303289388835));
#50593=CARTESIAN_POINT('Ctrl Pts',(-89.7562265507268,-3.21998389906979,
-0.00260811917007466));
#50594=CARTESIAN_POINT('Ctrl Pts',(-89.7348052990017,-3.22261347762718,
-0.350266587756745));
#50595=CARTESIAN_POINT('Ctrl Pts',(-89.6470928700442,-3.01031348933854,
-1.77067940302499));
#50596=CARTESIAN_POINT('Ctrl Pts',(-89.4930892638543,-0.936121843189332,
-3.69505311547631));
#50597=CARTESIAN_POINT('Ctrl Pts',(-89.2942157321568,2.60250934034945,-2.78508290089926));
#50598=CARTESIAN_POINT('Ctrl Pts',(-89.0953422004592,3.74994959831413,0.683827201558385));
#50599=CARTESIAN_POINT('Ctrl Pts',(-88.896468668762,1.45192846567913,3.52443546714054));
#50600=CARTESIAN_POINT('Ctrl Pts',(-88.7000967855176,-2.13443955597185,
3.13178726832469));
#50601=CARTESIAN_POINT('Ctrl Pts',(-88.5700160795061,-3.22463754819128,
1.02801970744573));
#50602=CARTESIAN_POINT('Ctrl Pts',(-88.5062265507269,-3.22786524494525,
-0.000750638361630088));
#50603=CARTESIAN_POINT('Origin',(-111.877773449273,0.,0.));
#50604=CARTESIAN_POINT('',(-91.2527734492731,-3.22699129851545,0.00168617155983299));
#50605=CARTESIAN_POINT('',(-91.0062265507269,-3.21842136713232,0.00180749504835861));
#50606=CARTESIAN_POINT('',(-111.877773449273,-3.22275,5.46201577318104E-12));
#50607=CARTESIAN_POINT('Ctrl Pts',(-91.2527734492731,-3.22699129851545,
0.00168617155983283));
#50608=CARTESIAN_POINT('Ctrl Pts',(-91.1924361502277,-3.22081317993391,
-0.972107811042261));
#50609=CARTESIAN_POINT('Ctrl Pts',(-91.0658076739498,-2.23190618928049,
-3.02665336582039));
#50610=CARTESIAN_POINT('Ctrl Pts',(-90.8728880204393,1.26656788840972,-3.59521173445138));
#50611=CARTESIAN_POINT('Ctrl Pts',(-90.6740144887419,3.70928654863654,-0.878029003844108));
#50612=CARTESIAN_POINT('Ctrl Pts',(-90.4751409570445,2.74390511179979,2.64588857832797));
#50613=CARTESIAN_POINT('Ctrl Pts',(-90.276267425347,-0.742581975743678,
3.73875830200189));
#50614=CARTESIAN_POINT('Ctrl Pts',(-90.1188115894232,-2.96277612187353,
1.88426197372598));
#50615=CARTESIAN_POINT('Ctrl Pts',(-90.0276469307319,-3.22105568130425,
0.406110880721617));
#50616=CARTESIAN_POINT('Ctrl Pts',(-90.0027734492731,-3.21873657735583,
0.00203080160484068));
#50617=CARTESIAN_POINT('Ctrl Pts',(-91.0062265507269,-3.21842136713232,
0.00180749504835851));
#50618=CARTESIAN_POINT('Ctrl Pts',(-90.9658856957301,-3.21509338775306,
-0.65370728955473));
#50619=CARTESIAN_POINT('Ctrl Pts',(-90.8592536635008,-2.70133149590602,
-2.39120601286823));
#50620=CARTESIAN_POINT('Ctrl Pts',(-90.6863304540388,0.141677647057878,
-3.80915595320164));
#50621=CARTESIAN_POINT('Ctrl Pts',(-90.4874569223416,3.28115912184763,-1.94003516684714));
#50622=CARTESIAN_POINT('Ctrl Pts',(-90.288583390644,3.40590485836977,1.71159391422753));
#50623=CARTESIAN_POINT('Ctrl Pts',(-90.0897098589466,0.401298217770733,
3.79060699254111));
#50624=CARTESIAN_POINT('Ctrl Pts',(-89.9122575789742,-2.60867182378199,
2.53801047560143));
#50625=CARTESIAN_POINT('Ctrl Pts',(-89.8010964762342,-3.21447586454873,
0.725613078532235));
#50626=CARTESIAN_POINT('Ctrl Pts',(-89.7562265507268,-3.21998389906979,
-0.00260811917007466));
#50627=CARTESIAN_POINT('Origin',(-111.877773449273,0.,0.));
#50628=CARTESIAN_POINT('',(-92.5027734492732,-3.22396460283213,-0.00285819432760913));
#50629=CARTESIAN_POINT('',(-92.2562265507269,-3.22661103672827,0.00193834844061623));
#50630=CARTESIAN_POINT('',(-111.877773449273,-3.22275,5.46201577318104E-12));
#50631=CARTESIAN_POINT('Ctrl Pts',(-92.5027734492732,-3.22396460283213,
-0.00285819432760914));
#50632=CARTESIAN_POINT('Ctrl Pts',(-92.4898077241885,-3.22590173312812,
-0.212625971653954));
#50633=CARTESIAN_POINT('Ctrl Pts',(-92.4105508218713,-3.11151461565573,
-1.49279130520091));
#50634=CARTESIAN_POINT('Ctrl Pts',(-92.2650027423214,-1.39838957449524,
-3.54601864482274));
#50635=CARTESIAN_POINT('Ctrl Pts',(-92.0661292106243,2.22722809688435,-3.09341181156606));
#50636=CARTESIAN_POINT('Ctrl Pts',(-91.8672556789264,3.80646401974024,0.201428145775125));
#50637=CARTESIAN_POINT('Ctrl Pts',(-91.6683821472293,1.88831298555067,3.31119550919123));
#50638=CARTESIAN_POINT('Ctrl Pts',(-91.4695086155316,-1.7648238969841,3.37862963997555));
#50639=CARTESIAN_POINT('Ctrl Pts',(-91.3309723828797,-3.18005506152525,
1.26314034387524));
#50640=CARTESIAN_POINT('Ctrl Pts',(-91.2587273274602,-3.22760093411468,
0.0977768293023363));
#50641=CARTESIAN_POINT('Ctrl Pts',(-91.2527734492731,-3.22699129851545,
0.00168617155983283));
#50642=CARTESIAN_POINT('Ctrl Pts',(-92.2562265507269,-3.22661103672827,
0.00193834844061606));
#50643=CARTESIAN_POINT('Ctrl Pts',(-92.1969660924583,-3.219827206744,-0.954773087278188));
#50644=CARTESIAN_POINT('Ctrl Pts',(-92.0714144569572,-2.26128400223956,
-2.99350364556276));
#50645=CARTESIAN_POINT('Ctrl Pts',(-91.8795716442237,1.2080230691099,-3.61530384559662));
#50646=CARTESIAN_POINT('Ctrl Pts',(-91.6806981125261,3.69454037918903,-0.938143388842634));
#50647=CARTESIAN_POINT('Ctrl Pts',(-91.4818245808289,2.78650640297092,2.60098513984405));
#50648=CARTESIAN_POINT('Ctrl Pts',(-91.2829510491313,-0.681775377754059,
3.75032318151061));
#50649=CARTESIAN_POINT('Ctrl Pts',(-91.1244183724306,-2.94717735151063,
1.91968743215883));
#50650=CARTESIAN_POINT('Ctrl Pts',(-91.0321768729625,-3.22056217791316,
0.423484722564532));
#50651=CARTESIAN_POINT('Ctrl Pts',(-91.0062265507269,-3.21842136713232,
0.00180749504835851));
#50652=CARTESIAN_POINT('Origin',(-111.877773449273,0.,0.));
#50653=CARTESIAN_POINT('',(-93.7527734492732,-3.21743785918669,-0.000338685115544857));
#50654=CARTESIAN_POINT('',(-93.5062265507269,-3.22448909586232,-0.00275643515406654));
#50655=CARTESIAN_POINT('',(-111.877773449273,-3.22275,5.46201577318104E-12));
#50656=CARTESIAN_POINT('Ctrl Pts',(-93.7527734492731,-3.21743785918669,
-0.000338685115544891));
#50657=CARTESIAN_POINT('Ctrl Pts',(-93.7208881209167,-3.2179221952485,-0.518851897634327));
#50658=CARTESIAN_POINT('Ctrl Pts',(-93.6227116153277,-2.85439961021422,
-2.11473897272031));
#50659=CARTESIAN_POINT('Ctrl Pts',(-93.4582439325062,-0.343849025370891,
-3.79624939634358));
#50660=CARTESIAN_POINT('Ctrl Pts',(-93.2593704008088,3.00782586757985,-2.34152197978259));
#50661=CARTESIAN_POINT('Ctrl Pts',(-93.0604968691114,3.59590417751189,1.26460063958548));
#50662=CARTESIAN_POINT('Ctrl Pts',(-92.8616233374138,0.880058345774601,
3.70880559473261));
#50663=CARTESIAN_POINT('Ctrl Pts',(-92.6757155308011,-2.41460776576439,
2.8081654885147));
#50664=CARTESIAN_POINT('Ctrl Pts',(-92.556098901421,-3.21599757065862,0.859875011787762));
#50665=CARTESIAN_POINT('Ctrl Pts',(-92.5027734492732,-3.22396460283213,
-0.00285819432760914));
#50666=CARTESIAN_POINT('Ctrl Pts',(-93.5062265507269,-3.22448909586232,
-0.00275643515406668));
#50667=CARTESIAN_POINT('Ctrl Pts',(-93.4943376664191,-3.22623439527328,
-0.195021731697769));
#50668=CARTESIAN_POINT('Ctrl Pts',(-93.4161576048787,-3.12291757706562,
-1.45746542359579));
#50669=CARTESIAN_POINT('Ctrl Pts',(-93.2716863661057,-1.45578426624114,
-3.52284456109722));
#50670=CARTESIAN_POINT('Ctrl Pts',(-93.0728128344086,2.17670468249244,-3.12916895624107));
#50671=CARTESIAN_POINT('Ctrl Pts',(-92.8739393027108,3.80923289958397,0.139593510646091));
#50672=CARTESIAN_POINT('Ctrl Pts',(-92.6750657710136,1.94183010714438,3.28009717332813));
#50673=CARTESIAN_POINT('Ctrl Pts',(-92.476192239316,-1.70973017484599,3.40684081822274));
#50674=CARTESIAN_POINT('Ctrl Pts',(-92.3365791658872,-3.170391492192,1.29834758764436));
#50675=CARTESIAN_POINT('Ctrl Pts',(-92.2632572696908,-3.22741587697946,
0.115443532683487));
#50676=CARTESIAN_POINT('Ctrl Pts',(-92.2562265507269,-3.22661103672827,
0.00193834844061606));
#50677=CARTESIAN_POINT('Origin',(-111.877773449273,0.,0.));
#50678=CARTESIAN_POINT('',(-95.0027734492731,-3.22271743805854,0.00297624318753977));
#50679=CARTESIAN_POINT('',(-94.7562265507269,-3.21751559249332,-0.000624871069029309));
#50680=CARTESIAN_POINT('',(-111.877773449273,-3.22275,5.46201577318104E-12));
#50681=CARTESIAN_POINT('Ctrl Pts',(-95.0027734492731,-3.22271743805854,
0.00297624318753967));
#50682=CARTESIAN_POINT('Ctrl Pts',(-94.9519685176449,-3.21511270739749,
-0.819794381838916));
#50683=CARTESIAN_POINT('Ctrl Pts',(-94.8348724087843,-2.47539994819433,
-2.72828303166915));
#50684=CARTESIAN_POINT('Ctrl Pts',(-94.6514851226908,0.738490335120334,
-3.73956864576937));
#50685=CARTESIAN_POINT('Ctrl Pts',(-94.4526115909935,3.54525300887773,-1.40032950926946));
#50686=CARTESIAN_POINT('Ctrl Pts',(-94.2537380592961,3.09462993870752,2.22553525560538));
#50687=CARTESIAN_POINT('Ctrl Pts',(-94.0548645275986,-0.199345473265892,
3.80657365799952));
#50688=CARTESIAN_POINT('Ctrl Pts',(-93.8878763242577,-2.8114056810318,2.19738805605108));
#50689=CARTESIAN_POINT('Ctrl Pts',(-93.7871792981492,-3.21691523658229,
0.559162758014472));
#50690=CARTESIAN_POINT('Ctrl Pts',(-93.7527734492731,-3.21743785918669,
-0.000338685115544891));
#50691=CARTESIAN_POINT('Ctrl Pts',(-94.7562265507269,-3.21751559249332,
-0.000624871069029309));
#50692=CARTESIAN_POINT('Ctrl Pts',(-94.7254180631473,-3.21838016512199,
-0.501596526159939));
#50693=CARTESIAN_POINT('Ctrl Pts',(-94.6283183983351,-2.87210498626068,
-2.07938641916441));
#50694=CARTESIAN_POINT('Ctrl Pts',(-94.4649275562905,-0.40544590980093,
-3.79016559608063));
#50695=CARTESIAN_POINT('Ctrl Pts',(-94.2660540245932,2.96940847303638,-2.39005333659048));
#50696=CARTESIAN_POINT('Ctrl Pts',(-94.0671804928955,3.61596425384286,1.20604483598993));
#50697=CARTESIAN_POINT('Ctrl Pts',(-93.8683069611984,0.940164653658382,
3.69402653692401));
#50698=CARTESIAN_POINT('Ctrl Pts',(-93.6813223138085,-2.38785739210696,
2.84209660064214));
#50699=CARTESIAN_POINT('Ctrl Pts',(-93.5606288436515,-3.21650278803584,
0.877029481754939));
#50700=CARTESIAN_POINT('Ctrl Pts',(-93.5062265507269,-3.22448909586232,
-0.00275643515406668));
#50701=CARTESIAN_POINT('Origin',(-111.877773449273,0.,0.));
#50702=CARTESIAN_POINT('',(-96.2527734492731,-3.22768866803615,-0.00101868579972961));
#50703=CARTESIAN_POINT('',(-96.0062265507269,-3.22218870514462,0.00297531656463582));
#50704=CARTESIAN_POINT('',(-111.877773449273,-3.22275,5.46201577318104E-12));
#50705=CARTESIAN_POINT('Ctrl Pts',(-96.2527734492731,-3.22768866803615,
-0.00101868579972937));
#50706=CARTESIAN_POINT('Ctrl Pts',(-96.2493400916056,-3.22791730388182,
-0.0563985044060784));
#50707=CARTESIAN_POINT('Ctrl Pts',(-96.1796155567056,-3.20148940574067,
-1.18082759072959));
#50708=CARTESIAN_POINT('Ctrl Pts',(-96.0435998445732,-1.89193518361277,
-3.30912721008056));
#50709=CARTESIAN_POINT('Ctrl Pts',(-95.8447263128756,1.76112572087986,-3.38055880391732));
#50710=CARTESIAN_POINT('Ctrl Pts',(-95.6458527811783,3.79606069695695,-0.345926027506187));
#50711=CARTESIAN_POINT('Ctrl Pts',(-95.4469792494807,2.3431673103227,3.00654429325805));
#50712=CARTESIAN_POINT('Ctrl Pts',(-95.2481057177834,-1.26263301219719,
3.59659554412187));
#50713=CARTESIAN_POINT('Ctrl Pts',(-95.100037117714,-3.0835388319343,1.57554521251432));
#50714=CARTESIAN_POINT('Ctrl Pts',(-95.0182596948773,-3.22503549504625,
0.253771344504622));
#50715=CARTESIAN_POINT('Ctrl Pts',(-95.0027734492731,-3.22271743805854,
0.00297624318753967));
#50716=CARTESIAN_POINT('Ctrl Pts',(-96.0062265507269,-3.22218870514462,
0.00297531656463585));
#50717=CARTESIAN_POINT('Ctrl Pts',(-95.9564984598755,-3.21485431378588,
-0.802693432952016));
#50718=CARTESIAN_POINT('Ctrl Pts',(-95.8404791917917,-2.50060164354313,
-2.69397249512217));
#50719=CARTESIAN_POINT('Ctrl Pts',(-95.6581687464753,0.677671118481855,
-3.7510669797623));
#50720=CARTESIAN_POINT('Ctrl Pts',(-95.4592952147778,3.52204752608671,-1.45771151311705));
#50721=CARTESIAN_POINT('Ctrl Pts',(-95.2604216830804,3.13035943499951,2.17499228485918));
#50722=CARTESIAN_POINT('Ctrl Pts',(-95.0615481513829,-0.137509332446344,
3.80930870565481));
#50723=CARTESIAN_POINT('Ctrl Pts',(-94.8934831072652,-2.79236499959111,
2.23264688773096));
#50724=CARTESIAN_POINT('Ctrl Pts',(-94.7917092403798,-3.21651984863585,
0.576353200851608));
#50725=CARTESIAN_POINT('Ctrl Pts',(-94.7562265507269,-3.21751559249332,
-0.000624871069029309));
#50726=CARTESIAN_POINT('Origin',(-111.877773449273,0.,0.));
#50727=CARTESIAN_POINT('',(-97.5027734492731,-3.2196148652113,-0.00247533961895227));
#50728=CARTESIAN_POINT('',(-97.2562265507269,-3.2278883009554,-0.000708117556544874));
#50729=CARTESIAN_POINT('',(-111.877773449273,-3.22275,5.46201577318104E-12));
#50730=CARTESIAN_POINT('Ctrl Pts',(-97.5027734492731,-3.2196148652113,-0.00247533961895269));
#50731=CARTESIAN_POINT('Ctrl Pts',(-97.4804204883339,-3.22219931499525,
-0.365359803868385));
#50732=CARTESIAN_POINT('Ctrl Pts',(-97.3917763501621,-2.99785044664452,
-1.8013328317353));
#50733=CARTESIAN_POINT('Ctrl Pts',(-97.236841034758,-0.884116238679596,
-3.70784035632476));
#50734=CARTESIAN_POINT('Ctrl Pts',(-97.0379675030604,2.6413811721456,-2.74824437321759));
#50735=CARTESIAN_POINT('Ctrl Pts',(-96.8390939713629,3.73997213852792,0.736444182896666));
#50736=CARTESIAN_POINT('Ctrl Pts',(-96.6402204396655,1.4022690248486,3.54448631164484));
#50737=CARTESIAN_POINT('Ctrl Pts',(-96.4447802656356,-2.16124048025456,
3.10359245744214));
#50738=CARTESIAN_POINT('Ctrl Pts',(-96.3156312688381,-3.22350280914098,
1.01287353942035));
#50739=CARTESIAN_POINT('Ctrl Pts',(-96.2527734492731,-3.22768866803615,
-0.00101868579972937));
#50740=CARTESIAN_POINT('Ctrl Pts',(-97.2562265507269,-3.2278883009554,-0.000708117556544644));
#50741=CARTESIAN_POINT('Ctrl Pts',(-97.2538700338363,-3.22800134428475,
-0.0387122915581514));
#50742=CARTESIAN_POINT('Ctrl Pts',(-97.1852223397131,-3.21014838855854,
-1.14570314954745));
#50743=CARTESIAN_POINT('Ctrl Pts',(-97.0502834683574,-1.94541824331421,
-3.27797033087057));
#50744=CARTESIAN_POINT('Ctrl Pts',(-96.8514099366601,1.70600116119408,-3.40870967808817));
#50745=CARTESIAN_POINT('Ctrl Pts',(-96.6525364049625,3.78994319591188,-0.407519574068266));
#50746=CARTESIAN_POINT('Ctrl Pts',(-96.4536628732652,2.39167764043941,2.96810035135433));
#50747=CARTESIAN_POINT('Ctrl Pts',(-96.2547893415676,-1.20406624183485,
3.6166235796335));
#50748=CARTESIAN_POINT('Ctrl Pts',(-96.1056439007216,-3.07102873086741,
1.6109256742346));
#50749=CARTESIAN_POINT('Ctrl Pts',(-96.022789637108,-3.22463159316923,0.271321856002311));
#50750=CARTESIAN_POINT('Ctrl Pts',(-96.0062265507269,-3.22218870514462,
0.00297531656463585));
#50751=CARTESIAN_POINT('Origin',(-111.877773449273,0.,0.));
#50752=CARTESIAN_POINT('',(-98.7527734492732,-3.21869187673167,0.00200177019059543));
#50753=CARTESIAN_POINT('',(-98.5062265507269,-3.22004330425499,-0.00262713518237062));
#50754=CARTESIAN_POINT('',(-111.877773449273,-3.22275,5.46201577318104E-12));
#50755=CARTESIAN_POINT('Ctrl Pts',(-98.7527734492732,-3.21869187673167,
0.00200177019059538));
#50756=CARTESIAN_POINT('Ctrl Pts',(-98.7115008850621,-3.21490199884244,
-0.668511583215047));
#50757=CARTESIAN_POINT('Ctrl Pts',(-98.6039371436185,-2.68289385566343,
-2.42149810263904));
#50758=CARTESIAN_POINT('Ctrl Pts',(-98.4300822249426,0.195179949845956,
-3.80678951593933));
#50759=CARTESIAN_POINT('Ctrl Pts',(-98.2312086932451,3.30809157446657,-1.89374543337553));
#50760=CARTESIAN_POINT('Ctrl Pts',(-98.0323351615477,3.38152186805364,1.75927584174923));
#50761=CARTESIAN_POINT('Ctrl Pts',(-97.8334616298501,0.348002926086945,
3.795870861202));
#50762=CARTESIAN_POINT('Ctrl Pts',(-97.6569410590921,-2.62836201115969,
2.50790786839153));
#50763=CARTESIAN_POINT('Ctrl Pts',(-97.5467116655664,-3.2145347277783,0.710830433291791));
#50764=CARTESIAN_POINT('Ctrl Pts',(-97.5027734492731,-3.2196148652113,-0.00247533961895269));
#50765=CARTESIAN_POINT('Ctrl Pts',(-98.5062265507269,-3.22004330425499,
-0.00262713518237034));
#50766=CARTESIAN_POINT('Ctrl Pts',(-98.4849504305645,-3.22267740745809,
-0.347914118107918));
#50767=CARTESIAN_POINT('Ctrl Pts',(-98.3973831331696,-3.01223074102848,
-1.76590478459706));
#50768=CARTESIAN_POINT('Ctrl Pts',(-98.2435246585422,-0.94420633835697,
-3.69299553507636));
#50769=CARTESIAN_POINT('Ctrl Pts',(-98.0446511268448,2.59640786845259,-2.79077190256118));
#50770=CARTESIAN_POINT('Ctrl Pts',(-97.8457775951473,3.75143719459486,0.675618684242606));
#50771=CARTESIAN_POINT('Ctrl Pts',(-97.6469040634498,1.45963832362029,3.52124943673499));
#50772=CARTESIAN_POINT('Ctrl Pts',(-97.450387048643,-2.13023161929317,3.13616666364257));
#50773=CARTESIAN_POINT('Ctrl Pts',(-97.3201612110688,-3.22482132235888,
1.03038313666224));
#50774=CARTESIAN_POINT('Ctrl Pts',(-97.2562265507269,-3.2278883009554,-0.000708117556544644));
#50775=CARTESIAN_POINT('Origin',(-111.877773449273,0.,0.));
#50776=CARTESIAN_POINT('',(-100.002773449273,-3.22694260859439,0.00172144473337393));
#50777=CARTESIAN_POINT('',(-99.7562265507269,-3.21838185199414,0.00177605862614089));
#50778=CARTESIAN_POINT('',(-111.877773449273,-3.22275,5.46201577318104E-12));
#50779=CARTESIAN_POINT('Ctrl Pts',(-100.002773449273,-3.22694260859439,
0.001721444733374));
#50780=CARTESIAN_POINT('Ctrl Pts',(-99.9425812817904,-3.22067473021912,
-0.969768895307658));
#50781=CARTESIAN_POINT('Ctrl Pts',(-99.8160979370751,-2.23589384257021,
-3.02219500214244));
#50782=CARTESIAN_POINT('Ctrl Pts',(-99.6233234151273,1.25869662408462,-3.5979750471627));
#50783=CARTESIAN_POINT('Ctrl Pts',(-99.4244498834298,3.70735607210978,-0.886144788439325));
#50784=CARTESIAN_POINT('Ctrl Pts',(-99.2255763517325,2.74968914886796,2.63987712139888));
#50785=CARTESIAN_POINT('Ctrl Pts',(-99.0267028200349,-0.734397810215034,
3.74037451170853));
#50786=CARTESIAN_POINT('Ctrl Pts',(-98.8691018525486,-2.96069541412064,
1.88903672785569));
#50787=CARTESIAN_POINT('Ctrl Pts',(-98.7777920622946,-3.22098922583323,
0.40845371799762));
#50788=CARTESIAN_POINT('Ctrl Pts',(-98.7527734492732,-3.21869187673167,
0.00200177019059538));
#50789=CARTESIAN_POINT('Ctrl Pts',(-99.7562265507269,-3.21838185199414,
0.0017760586261405));
#50790=CARTESIAN_POINT('Ctrl Pts',(-99.7160308272927,-3.21512588995624,
-0.651400495484813));
#50791=CARTESIAN_POINT('Ctrl Pts',(-99.6095439266259,-2.70417477442122,
-2.38648362041853));
#50792=CARTESIAN_POINT('Ctrl Pts',(-99.4367658487271,0.133340853178626,
-3.80945689677165));
#50793=CARTESIAN_POINT('Ctrl Pts',(-99.2378923170293,3.2769054375692,-1.94721143811269));
#50794=CARTESIAN_POINT('Ctrl Pts',(-99.0390187853321,3.40964257754116,1.70413588804003));
#50795=CARTESIAN_POINT('Ctrl Pts',(-98.8401452536345,0.409593116342725,
3.78971966120611));
#50796=CARTESIAN_POINT('Ctrl Pts',(-98.6625478420995,-2.60557504043074,
2.5426944940956));
#50797=CARTESIAN_POINT('Ctrl Pts',(-98.551241607797,-3.21447018729988,0.72791551654661));
#50798=CARTESIAN_POINT('Ctrl Pts',(-98.5062265507269,-3.22004330425499,
-0.00262713518237034));
#50799=CARTESIAN_POINT('Origin',(-111.877773449273,0.,0.));
#50800=CARTESIAN_POINT('',(-101.252773449273,-3.22403583900848,-0.00284625812878155));
#50801=CARTESIAN_POINT('',(-101.006226550727,-3.22655659286261,0.00197058666357074));
#50802=CARTESIAN_POINT('',(-111.877773449273,-3.22275,5.46201577318104E-12));
#50803=CARTESIAN_POINT('Ctrl Pts',(-101.252773449273,-3.22403583900848,
-0.00284625812878147));
#50804=CARTESIAN_POINT('Ctrl Pts',(-101.239952855751,-3.22594794128741,
-0.210254204409943));
#50805=CARTESIAN_POINT('Ctrl Pts',(-101.160841084997,-3.11307044583999,
-1.48802917026718));
#50806=CARTESIAN_POINT('Ctrl Pts',(-101.015438137009,-1.40614679609923,
-3.54294973423381));
#50807=CARTESIAN_POINT('Ctrl Pts',(-100.816564605312,2.22045273645088,-3.09827876032406));
#50808=CARTESIAN_POINT('Ctrl Pts',(-100.617691073615,3.80689573555524,0.193097100182191));
#50809=CARTESIAN_POINT('Ctrl Pts',(-100.418817541917,1.89555511623687,3.30705494856008));
#50810=CARTESIAN_POINT('Ctrl Pts',(-100.21994401022,-1.75742543597124,3.38248391991576));
#50811=CARTESIAN_POINT('Ctrl Pts',(-100.081262646005,-3.17877047756002,
1.26788401495614));
#50812=CARTESIAN_POINT('Ctrl Pts',(-100.008872459023,-3.22757770536726,
0.100158322875876));
#50813=CARTESIAN_POINT('Ctrl Pts',(-100.002773449273,-3.22694260859439,
0.001721444733374));
#50814=CARTESIAN_POINT('Ctrl Pts',(-101.006226550727,-3.22655659286261,
0.00197058666357072));
#50815=CARTESIAN_POINT('Ctrl Pts',(-100.947111224021,-3.21970155042776,
-0.952440118260013));
#50816=CARTESIAN_POINT('Ctrl Pts',(-100.821704720082,-2.26520642155357,
-2.98902372995717));
#50817=CARTESIAN_POINT('Ctrl Pts',(-100.630007038912,1.20010797278872,-3.61793898305879));
#50818=CARTESIAN_POINT('Ctrl Pts',(-100.431133507214,3.69247837580237,-0.946226757029911));
#50819=CARTESIAN_POINT('Ctrl Pts',(-100.232259975517,2.79219206546425,2.59488055621948));
#50820=CARTESIAN_POINT('Ctrl Pts',(-100.033386443819,-0.673566047753791,
3.75180628641736));
#50821=CARTESIAN_POINT('Ctrl Pts',(-99.8747086355561,-2.94504656405884,
1.92446147751931));
#50822=CARTESIAN_POINT('Ctrl Pts',(-99.7823220045252,-3.22049565415193,
0.425824617370613));
#50823=CARTESIAN_POINT('Ctrl Pts',(-99.7562265507269,-3.21838185199414,
0.0017760586261405));
#50824=CARTESIAN_POINT('Origin',(-111.877773449273,0.,0.));
#50825=CARTESIAN_POINT('',(-102.502773449273,-3.21744563600034,-0.000377495323892581));
#50826=CARTESIAN_POINT('',(-102.256226550727,-3.22455892594853,-0.00274040190877844));
#50827=CARTESIAN_POINT('',(-111.877773449273,-3.22275,5.46201577318104E-12));
#50828=CARTESIAN_POINT('Ctrl Pts',(-102.502773449273,-3.21744563600034,
-0.000377495323892994));
#50829=CARTESIAN_POINT('Ctrl Pts',(-102.471033252479,-3.21798308710835,
-0.516527495821932));
#50830=CARTESIAN_POINT('Ctrl Pts',(-102.373001878453,-2.85680880773506,
-2.10997563087918));
#50831=CARTESIAN_POINT('Ctrl Pts',(-102.208679327194,-0.352156410097993,
-3.79548778081539));
#50832=CARTESIAN_POINT('Ctrl Pts',(-102.009805795497,3.00269417169098,-2.34809909134587));
#50833=CARTESIAN_POINT('Ctrl Pts',(-101.810932263799,3.59866318318054,1.25672786453859));
#50834=CARTESIAN_POINT('Ctrl Pts',(-101.612058732102,0.888173072927529,
3.70687067808071));
#50835=CARTESIAN_POINT('Ctrl Pts',(-101.426005793926,-2.41102978727076,
2.81274573972963));
#50836=CARTESIAN_POINT('Ctrl Pts',(-101.306244032984,-3.21606107365988,
0.862185765134263));
#50837=CARTESIAN_POINT('Ctrl Pts',(-101.252773449273,-3.22403583900848,
-0.00284625812878147));
#50838=CARTESIAN_POINT('Ctrl Pts',(-102.256226550727,-3.22455892594853,
-0.0027404019087786));
#50839=CARTESIAN_POINT('Ctrl Pts',(-102.244482797982,-3.22627739521217,
-0.192648026627219));
#50840=CARTESIAN_POINT('Ctrl Pts',(-102.166447868004,-3.1244295976162,-1.45270581183642));
#50841=CARTESIAN_POINT('Ctrl Pts',(-102.022121760794,-1.46349063320167,
-3.51965009596396));
#50842=CARTESIAN_POINT('Ctrl Pts',(-101.823248229096,2.16985118744687,-3.13392524732525));
#50843=CARTESIAN_POINT('Ctrl Pts',(-101.624374697399,3.80952928177325,0.131256553358462));
#50844=CARTESIAN_POINT('Ctrl Pts',(-101.425501165701,1.94900405000445,3.27583956331103));
#50845=CARTESIAN_POINT('Ctrl Pts',(-101.226627634004,-1.70227010474501,
3.41057445630188));
#50846=CARTESIAN_POINT('Ctrl Pts',(-101.086869429013,-3.16906561629859,
1.30309446990841));
#50847=CARTESIAN_POINT('Ctrl Pts',(-101.013402401253,-3.22738870802812,
0.117823935382279));
#50848=CARTESIAN_POINT('Ctrl Pts',(-101.006226550727,-3.22655659286261,
0.00197058666357072));
#50849=CARTESIAN_POINT('Origin',(-111.877773449273,0.,0.));
#50850=CARTESIAN_POINT('',(-103.752773449273,-3.22264579720397,0.00297789965849656));
#50851=CARTESIAN_POINT('',(-103.506226550727,-3.21752959531867,-0.000663060806946891));
#50852=CARTESIAN_POINT('',(-111.877773449273,-3.22275,5.46201577318104E-12));
#50853=CARTESIAN_POINT('Ctrl Pts',(-103.752773449273,-3.22264579720397,
0.00297789965849664));
#50854=CARTESIAN_POINT('Ctrl Pts',(-103.702113649208,-3.21507385712874,
-0.817488959989247));
#50855=CARTESIAN_POINT('Ctrl Pts',(-103.58516267191,-2.47882325582672,-2.72366489883768));
#50856=CARTESIAN_POINT('Ctrl Pts',(-103.401920517379,0.730304405924223,
-3.74117589888118));
#50857=CARTESIAN_POINT('Ctrl Pts',(-103.203046985682,3.5421798545178,-1.40808505059571));
#50858=CARTESIAN_POINT('Ctrl Pts',(-103.004173453984,3.09949317971213,2.2187572333099));
#50859=CARTESIAN_POINT('Ctrl Pts',(-102.805299922287,-0.191014192713332,
3.80700081556329));
#50860=CARTESIAN_POINT('Ctrl Pts',(-102.638166587383,-2.8088631270226,2.20214204929746));
#50861=CARTESIAN_POINT('Ctrl Pts',(-102.537324429712,-3.21686059039271,
0.561480664739076));
#50862=CARTESIAN_POINT('Ctrl Pts',(-102.502773449273,-3.21744563600034,
-0.000377495323892994));
#50863=CARTESIAN_POINT('Ctrl Pts',(-103.506226550727,-3.21752959531867,
-0.000663060806946926));
#50864=CARTESIAN_POINT('Ctrl Pts',(-103.47556319471,-3.21844290636372,-0.499269344977216));
#50865=CARTESIAN_POINT('Ctrl Pts',(-103.37860866146,-2.87446123529701,-2.0746201369058));
#50866=CARTESIAN_POINT('Ctrl Pts',(-103.215362950979,-0.413739832431433,
-3.78926918845535));
#50867=CARTESIAN_POINT('Ctrl Pts',(-103.016489419281,2.96417065678915,-2.39654625428174));
#50868=CARTESIAN_POINT('Ctrl Pts',(-102.817615887584,3.61859506029929,1.19812829908153));
#50869=CARTESIAN_POINT('Ctrl Pts',(-102.618742355886,0.948246892445682,
3.69196011116847));
#50870=CARTESIAN_POINT('Ctrl Pts',(-102.431612576934,-2.38421620433085,
2.84666010714341));
#50871=CARTESIAN_POINT('Ctrl Pts',(-102.310773975214,-3.21657697380546,
0.879343208300523));
#50872=CARTESIAN_POINT('Ctrl Pts',(-102.256226550727,-3.22455892594853,
-0.0027404019087786));
#50873=CARTESIAN_POINT('Origin',(-111.877773449273,0.,0.));
#50874=CARTESIAN_POINT('',(-105.002773449273,-3.22771932735903,-0.000977548123388087));
#50875=CARTESIAN_POINT('',(-104.756226550727,-3.22211806513786,0.00297286732293386));
#50876=CARTESIAN_POINT('',(-111.877773449273,-3.22275,5.46201577318104E-12));
#50877=CARTESIAN_POINT('Ctrl Pts',(-105.002773449273,-3.22771932735903,
-0.000977548123388232));
#50878=CARTESIAN_POINT('Ctrl Pts',(-104.999485223168,-3.22793043470303,
-0.0540150617505775));
#50879=CARTESIAN_POINT('Ctrl Pts',(-104.929905819831,-3.20267366849749,
-1.17609219946835));
#50880=CARTESIAN_POINT('Ctrl Pts',(-104.794035239261,-1.89917277873868,
-3.30497872482143));
#50881=CARTESIAN_POINT('Ctrl Pts',(-104.595161707564,1.75372304650391,-3.38440498687836));
#50882=CARTESIAN_POINT('Ctrl Pts',(-104.396288175866,3.79529453639531,-0.354232993642497));
#50883=CARTESIAN_POINT('Ctrl Pts',(-104.197414644169,2.34974161312935,3.00140899924184));
#50884=CARTESIAN_POINT('Ctrl Pts',(-103.998541112471,-1.25475872875807,
3.59935024210211));
#50885=CARTESIAN_POINT('Ctrl Pts',(-103.850327380839,-3.08187243645139,
1.58031280791233));
#50886=CARTESIAN_POINT('Ctrl Pts',(-103.76840482644,-3.22498216353482,0.256137740784716));
#50887=CARTESIAN_POINT('Ctrl Pts',(-103.752773449273,-3.22264579720397,
0.00297789965849664));
#50888=CARTESIAN_POINT('Ctrl Pts',(-104.756226550727,-3.22211806513786,
0.00297286732293373));
#50889=CARTESIAN_POINT('Ctrl Pts',(-104.706643591438,-3.21482468722874,
-0.800389402427977));
#50890=CARTESIAN_POINT('Ctrl Pts',(-104.590769454917,-2.50396322193643,
-2.68934045447677));
#50891=CARTESIAN_POINT('Ctrl Pts',(-104.408604141163,0.66946017042967,-3.75254110076405));
#50892=CARTESIAN_POINT('Ctrl Pts',(-104.209730609466,3.51884884505274,-1.46541613103467));
#50893=CARTESIAN_POINT('Ctrl Pts',(-104.010857077768,3.1351119755824,2.16813618846657));
#50894=CARTESIAN_POINT('Ctrl Pts',(-103.811983546071,-0.129172214237829,
3.80960052640045));
#50895=CARTESIAN_POINT('Ctrl Pts',(-103.64377337039,-2.78976765512291,2.23739622108886));
#50896=CARTESIAN_POINT('Ctrl Pts',(-103.541854371942,-3.21646841719422,
0.57866868420927));
#50897=CARTESIAN_POINT('Ctrl Pts',(-103.506226550727,-3.21752959531867,
-0.000663060806946926));
#50898=CARTESIAN_POINT('Origin',(-111.877773449273,0.,0.));
#50899=CARTESIAN_POINT('',(-106.252773449273,-3.21967089505607,-0.00249719049460675));
#50900=CARTESIAN_POINT('',(-106.006226550727,-3.22791011323673,-0.000665423688525069));
#50901=CARTESIAN_POINT('',(-111.877773449273,-3.22275,5.46201577318104E-12));
#50902=CARTESIAN_POINT('Ctrl Pts',(-106.252773449273,-3.21967089505607,
-0.00249719049460629));
#50903=CARTESIAN_POINT('Ctrl Pts',(-106.230565619897,-3.22226422533865,
-0.36300978920333));
#50904=CARTESIAN_POINT('Ctrl Pts',(-106.142066613287,-2.99980948769902,
-1.79655795925824));
#50905=CARTESIAN_POINT('Ctrl Pts',(-105.987276429446,-0.89222882781209,
-3.70589645739097));
#50906=CARTESIAN_POINT('Ctrl Pts',(-105.788402897748,2.63536022101092,-2.75401859025452));
#50907=CARTESIAN_POINT('Ctrl Pts',(-105.589529366051,3.74157491702501,0.728257404654141));
#50908=CARTESIAN_POINT('Ctrl Pts',(-105.390655834353,1.41002288124958,3.54140889901514));
#50909=CARTESIAN_POINT('Ctrl Pts',(-105.195070528761,-2.15708992623015,
3.10799336322487));
#50910=CARTESIAN_POINT('Ctrl Pts',(-105.065776400401,-3.22367447604636,
1.01522990611466));
#50911=CARTESIAN_POINT('Ctrl Pts',(-105.002773449273,-3.22771932735903,
-0.000977548123388232));
#50912=CARTESIAN_POINT('Ctrl Pts',(-106.006226550727,-3.22791011323674,
-0.000665423688524592));
#50913=CARTESIAN_POINT('Ctrl Pts',(-106.004015165399,-3.22801029914443,
-0.0363283773460198));
#50914=CARTESIAN_POINT('Ctrl Pts',(-105.935512602838,-3.21129287176671,
-1.14097121261763));
#50915=CARTESIAN_POINT('Ctrl Pts',(-105.800718863045,-1.95258751815794,
-3.27370485835312));
#50916=CARTESIAN_POINT('Ctrl Pts',(-105.601845331348,1.69853700744364,-3.41243515849443));
#50917=CARTESIAN_POINT('Ctrl Pts',(-105.402971799651,3.78904225187362,-0.415813000837348));
#50918=CARTESIAN_POINT('Ctrl Pts',(-105.204098267953,2.39816769067077,2.96285898119487));
#50919=CARTESIAN_POINT('Ctrl Pts',(-105.005224736256,-1.19614826633649,
3.61925005546539));
#50920=CARTESIAN_POINT('Ctrl Pts',(-104.855934163847,-3.0693168009762,1.61569511776405));
#50921=CARTESIAN_POINT('Ctrl Pts',(-104.772934768671,-3.22457575119371,
0.273685872019571));
#50922=CARTESIAN_POINT('Ctrl Pts',(-104.756226550727,-3.22211806513786,
0.00297286732293373));
#50923=CARTESIAN_POINT('Origin',(-111.877773449273,0.,0.));
#50924=CARTESIAN_POINT('',(-107.502773449273,-3.21864717840401,0.00197683862682141));
#50925=CARTESIAN_POINT('',(-107.256226550727,-3.22010315981886,-0.00264555290059448));
#50926=CARTESIAN_POINT('',(-111.877773449273,-3.22275,5.46201577318104E-12));
#50927=CARTESIAN_POINT('Ctrl Pts',(-107.502773449273,-3.21864717840401,
0.00197683862682117));
#50928=CARTESIAN_POINT('Ctrl Pts',(-107.461646016625,-3.21492939379356,
-0.66620337802367));
#50929=CARTESIAN_POINT('Ctrl Pts',(-107.354227406744,-2.68578800952235,
-2.41678954596452));
#50930=CARTESIAN_POINT('Ctrl Pts',(-107.180517619631,0.186848925119125,
-3.80720285370364));
#50931=CARTESIAN_POINT('Ctrl Pts',(-106.981644087933,3.3039387517963,-1.90098324867159));
#50932=CARTESIAN_POINT('Ctrl Pts',(-106.782770556236,3.3853642004366,1.75187238336515));
#50933=CARTESIAN_POINT('Ctrl Pts',(-106.583897024538,0.356309365737235,
3.79509945705497));
#50934=CARTESIAN_POINT('Ctrl Pts',(-106.407231322217,-2.62531646247706,
2.51260078542008));
#50935=CARTESIAN_POINT('Ctrl Pts',(-106.296856797129,-3.21452304026067,
0.713133411027618));
#50936=CARTESIAN_POINT('Ctrl Pts',(-106.252773449273,-3.21967089505607,
-0.00249719049460629));
#50937=CARTESIAN_POINT('Ctrl Pts',(-107.256226550727,-3.22010315981886,
-0.00264555290059414));
#50938=CARTESIAN_POINT('Ctrl Pts',(-107.235095562127,-3.22274118326769,
-0.345561327371345));
#50939=CARTESIAN_POINT('Ctrl Pts',(-107.147673396295,-3.01414178771879,
-1.76113107576296));
#50940=CARTESIAN_POINT('Ctrl Pts',(-106.99396005323,-0.952286095205662,
-3.69091959353343));
#50941=CARTESIAN_POINT('Ctrl Pts',(-106.795086521533,2.59029384628224,-2.79644789371376));
#50942=CARTESIAN_POINT('Ctrl Pts',(-106.596212989835,3.75290688327137,0.667407119671472));
#50943=CARTESIAN_POINT('Ctrl Pts',(-106.397339458138,1.46734115830479,3.5180464407433));
#50944=CARTESIAN_POINT('Ctrl Pts',(-106.200677311768,-2.12601470786238,
3.14054269339691));
#50945=CARTESIAN_POINT('Ctrl Pts',(-106.070306342631,-3.22500700447711,
1.03274771338295));
#50946=CARTESIAN_POINT('Ctrl Pts',(-106.006226550727,-3.22791011323674,
-0.000665423688524592));
#50947=CARTESIAN_POINT('Origin',(-111.877773449273,0.,0.));
#50948=CARTESIAN_POINT('',(-108.752773449273,-3.22685723674299,0.00199079345700962));
#50949=CARTESIAN_POINT('',(-108.506226550727,-3.21833411702487,0.00177219254916039));
#50950=CARTESIAN_POINT('',(-111.877773449273,-3.22275,5.46201577318104E-12));
#50951=CARTESIAN_POINT('Ctrl Pts',(-108.752773449273,-3.22685723674299,
0.00199079345700971));
#50952=CARTESIAN_POINT('Ctrl Pts',(-108.692726413353,-3.22049187575973,
-0.967128193374095));
#50953=CARTESIAN_POINT('Ctrl Pts',(-108.5663882002,-2.23993119932473,-3.01811690972611));
#50954=CARTESIAN_POINT('Ctrl Pts',(-108.373758809815,1.25085188316156,-3.60050797555933));
#50955=CARTESIAN_POINT('Ctrl Pts',(-108.174885278118,3.70539059895966,-0.894369208581839));
#50956=CARTESIAN_POINT('Ctrl Pts',(-107.97601174642,2.7554691459713,2.63391280124896));
#50957=CARTESIAN_POINT('Ctrl Pts',(-107.777138214723,-0.726214962520435,
3.74194114611939));
#50958=CARTESIAN_POINT('Ctrl Pts',(-107.619392115674,-2.95860695660328,
1.89381816019148));
#50959=CARTESIAN_POINT('Ctrl Pts',(-107.527937193857,-3.22092189813076,
0.410801684361577));
#50960=CARTESIAN_POINT('Ctrl Pts',(-107.502773449273,-3.21864717840401,
0.00197683862682117));
#50961=CARTESIAN_POINT('Ctrl Pts',(-108.506226550727,-3.21833411702487,
0.00177219254916029));
#50962=CARTESIAN_POINT('Ctrl Pts',(-108.466175958855,-3.2151539473228,-0.649077442870454));
#50963=CARTESIAN_POINT('Ctrl Pts',(-108.359834189751,-2.70702507792134,
-2.38180619169885));
#50964=CARTESIAN_POINT('Ctrl Pts',(-108.187201243415,0.125013204392657,
-3.80970909802013));
#50965=CARTESIAN_POINT('Ctrl Pts',(-107.988327711718,3.27263087647587,-1.95439453380991));
#50966=CARTESIAN_POINT('Ctrl Pts',(-107.78945418002,3.41336670979149,1.69667825319885));
#50967=CARTESIAN_POINT('Ctrl Pts',(-107.590580648323,0.417884599785739,
3.78880964833669));
#50968=CARTESIAN_POINT('Ctrl Pts',(-107.412838105225,-2.60246970424512,
2.54737878177037));
#50969=CARTESIAN_POINT('Ctrl Pts',(-107.30138673936,-3.21446529597712,0.730218458034701));
#50970=CARTESIAN_POINT('Ctrl Pts',(-107.256226550727,-3.22010315981886,
-0.00264555290059414));
#50971=CARTESIAN_POINT('Ctrl Pts',(-109.977063028692,-1.43290239521125,
2.88667772504966));
#50972=CARTESIAN_POINT('Ctrl Pts',(-109.910771851459,-2.39478902451357,
2.4092120062101));
#50973=CARTESIAN_POINT('Ctrl Pts',(-109.778189496994,-3.78690710807203,
0.425397354299135));
#50974=CARTESIAN_POINT('Ctrl Pts',(-109.579315965297,-2.40225732364717,
-2.962905510084));
#50975=CARTESIAN_POINT('Ctrl Pts',(-109.3804424336,1.19263195710595,-3.61916700220439));
#50976=CARTESIAN_POINT('Ctrl Pts',(-109.181568901902,3.6901636846244,-0.955038498682453));
#50977=CARTESIAN_POINT('Ctrl Pts',(-108.982695370205,2.7979887412231,2.58915131051891));
#50978=CARTESIAN_POINT('Ctrl Pts',(-108.783821838507,-0.665419358724505,
3.75306610556087));
#50979=CARTESIAN_POINT('Ctrl Pts',(-108.58494830681,-3.51720830079989,1.4693745407153));
#50980=CARTESIAN_POINT('Ctrl Pts',(-108.386074775112,-3.13750109000173,
-2.16476182736599));
#50981=CARTESIAN_POINT('Ctrl Pts',(-108.187201243415,0.125013204392657,
-3.80970909802013));
#50982=CARTESIAN_POINT('Ctrl Pts',(-107.988327711718,3.27263087647587,-1.95439453380991));
#50983=CARTESIAN_POINT('Ctrl Pts',(-107.78945418002,3.41336670979149,1.69667825319885));
#50984=CARTESIAN_POINT('Ctrl Pts',(-107.590580648323,0.417884599785739,
3.78880964833669));
#50985=CARTESIAN_POINT('Ctrl Pts',(-107.391707116625,-2.96154565338688,
2.39979080968668));
#50986=CARTESIAN_POINT('Ctrl Pts',(-107.192833584928,-3.61990437248132,
-1.19416914684889));
#50987=CARTESIAN_POINT('Ctrl Pts',(-106.99396005323,-0.952286095205662,
-3.69091959353343));
#50988=CARTESIAN_POINT('Ctrl Pts',(-106.795086521533,2.59029384628224,-2.79644789371376));
#50989=CARTESIAN_POINT('Ctrl Pts',(-106.596212989835,3.75290688327137,0.667407119671472));
#50990=CARTESIAN_POINT('Ctrl Pts',(-106.397339458138,1.46734115830479,3.5180464407433));
#50991=CARTESIAN_POINT('Ctrl Pts',(-106.19846592644,-2.16642052355891,3.13629781829738));
#50992=CARTESIAN_POINT('Ctrl Pts',(-105.999592394743,-3.80967063954889,
-0.127087864501012));
#50993=CARTESIAN_POINT('Ctrl Pts',(-105.800718863045,-1.95258751815794,
-3.27370485835312));
#50994=CARTESIAN_POINT('Ctrl Pts',(-105.601845331348,1.69853700744364,-3.41243515849443));
#50995=CARTESIAN_POINT('Ctrl Pts',(-105.402971799651,3.78904225187362,-0.415813000837348));
#50996=CARTESIAN_POINT('Ctrl Pts',(-105.204098267953,2.39816769067077,2.96285898119487));
#50997=CARTESIAN_POINT('Ctrl Pts',(-105.005224736256,-1.19614826633649,
3.61925005546539));
#50998=CARTESIAN_POINT('Ctrl Pts',(-104.806351204558,-3.69144074152657,
0.950266743380403));
#50999=CARTESIAN_POINT('Ctrl Pts',(-104.607477672861,-2.79502988317361,
-2.59182360151461));
#51000=CARTESIAN_POINT('Ctrl Pts',(-104.408604141163,0.66946017042967,-3.75254110076405));
#51001=CARTESIAN_POINT('Ctrl Pts',(-104.209730609466,3.51884884505274,-1.46541613103467));
#51002=CARTESIAN_POINT('Ctrl Pts',(-104.010857077768,3.1351119755824,2.16813618846657));
#51003=CARTESIAN_POINT('Ctrl Pts',(-103.811983546071,-0.129172214237829,
3.80960052640045));
#51004=CARTESIAN_POINT('Ctrl Pts',(-103.613110014373,-3.27477270841952,
1.95079607843917));
#51005=CARTESIAN_POINT('Ctrl Pts',(-103.414236482676,-3.41150531408905,
-1.70040381186034));
#51006=CARTESIAN_POINT('Ctrl Pts',(-103.215362950979,-0.413739832431433,
-3.78926918845535));
#51007=CARTESIAN_POINT('Ctrl Pts',(-103.016489419281,2.96417065678915,-2.39654625428174));
#51008=CARTESIAN_POINT('Ctrl Pts',(-102.817615887584,3.61859506029929,1.19812829908153));
#51009=CARTESIAN_POINT('Ctrl Pts',(-102.618742355886,0.948246892445682,
3.69196011116847));
#51010=CARTESIAN_POINT('Ctrl Pts',(-102.419868824189,-2.59335246719697,
2.79361139251142));
#51011=CARTESIAN_POINT('Ctrl Pts',(-102.220995292491,-3.75217425511925,
-0.671513209629694));
#51012=CARTESIAN_POINT('Ctrl Pts',(-102.022121760794,-1.46349063320167,
-3.51965009596396));
#51013=CARTESIAN_POINT('Ctrl Pts',(-101.823248229096,2.16985118744687,-3.13392524732525));
#51014=CARTESIAN_POINT('Ctrl Pts',(-101.624374697399,3.80952928177325,0.131256553358462));
#51015=CARTESIAN_POINT('Ctrl Pts',(-101.425501165701,1.94900405000445,3.27583956331103));
#51016=CARTESIAN_POINT('Ctrl Pts',(-101.226627634004,-1.70227010474501,
3.41057445630188));
#51017=CARTESIAN_POINT('Ctrl Pts',(-101.027754102307,-3.78949499203023,
0.411666536003608));
#51018=CARTESIAN_POINT('Ctrl Pts',(-100.828880570609,-2.39492409977199,
-2.96548144283838));
#51019=CARTESIAN_POINT('Ctrl Pts',(-100.630007038912,1.20010797278872,-3.61793898305879));
#51020=CARTESIAN_POINT('Ctrl Pts',(-100.431133507214,3.69247837580237,-0.946226757029911));
#51021=CARTESIAN_POINT('Ctrl Pts',(-100.232259975517,2.79219206546425,2.59488055621948));
#51022=CARTESIAN_POINT('Ctrl Pts',(-100.033386443819,-0.673566047753791,
3.75180628641736));
#51023=CARTESIAN_POINT('Ctrl Pts',(-99.834512912122,-3.52045029328096,1.46156469717404));
#51024=CARTESIAN_POINT('Ctrl Pts',(-99.6356393804242,-3.13273758089758,
-2.17156553682348));
#51025=CARTESIAN_POINT('Ctrl Pts',(-99.4367658487271,0.133340853178626,
-3.80945689677165));
#51026=CARTESIAN_POINT('Ctrl Pts',(-99.2378923170293,3.2769054375692,-1.94721143811269));
#51027=CARTESIAN_POINT('Ctrl Pts',(-99.0390187853321,3.40964257754116,1.70413588804003));
#51028=CARTESIAN_POINT('Ctrl Pts',(-98.8401452536345,0.409593116342725,
3.78971966120611));
#51029=CARTESIAN_POINT('Ctrl Pts',(-98.6412717219371,-2.9667913411577,2.39330122832859));
#51030=CARTESIAN_POINT('Ctrl Pts',(-98.4423981902396,-3.61728182277116,
-1.20208728723698));
#51031=CARTESIAN_POINT('Ctrl Pts',(-98.2435246585422,-0.94420633835697,
-3.69299553507636));
#51032=CARTESIAN_POINT('Ctrl Pts',(-98.0446511268448,2.59640786845259,-2.79077190256118));
#51033=CARTESIAN_POINT('Ctrl Pts',(-97.8457775951473,3.75143719459486,0.675618684242606));
#51034=CARTESIAN_POINT('Ctrl Pts',(-97.6469040634498,1.45963832362029,3.52124943673499));
#51035=CARTESIAN_POINT('Ctrl Pts',(-97.4480305317524,-2.17327923613194,
3.13154897667037));
#51036=CARTESIAN_POINT('Ctrl Pts',(-97.249157000055,-3.80938337139148,-0.135425113082561));
#51037=CARTESIAN_POINT('Ctrl Pts',(-97.0502834683574,-1.94541824331421,
-3.27797033087057));
#51038=CARTESIAN_POINT('Ctrl Pts',(-96.8514099366601,1.70600116119408,-3.40870967808817));
#51039=CARTESIAN_POINT('Ctrl Pts',(-96.6525364049625,3.78994319591188,-0.407519574068266));
#51040=CARTESIAN_POINT('Ctrl Pts',(-96.4536628732652,2.39167764043941,2.96810035135433));
#51041=CARTESIAN_POINT('Ctrl Pts',(-96.2547893415676,-1.20406624183485,
3.6166235796335));
#51042=CARTESIAN_POINT('Ctrl Pts',(-96.0559158098702,-3.69351158883507,
0.94218563703149));
#51043=CARTESIAN_POINT('Ctrl Pts',(-95.8570422781728,-2.78935090422765,
-2.59793440343899));
#51044=CARTESIAN_POINT('Ctrl Pts',(-95.6581687464753,0.677671118481855,
-3.7510669797623));
#51045=CARTESIAN_POINT('Ctrl Pts',(-95.4592952147778,3.52204752608671,-1.45771151311705));
#51046=CARTESIAN_POINT('Ctrl Pts',(-95.2604216830804,3.13035943499951,2.17499228485918));
#51047=CARTESIAN_POINT('Ctrl Pts',(-95.0615481513829,-0.137509332446344,
3.80930870565481));
#51048=CARTESIAN_POINT('Ctrl Pts',(-94.8626746196855,-3.27903424289638,
1.94362446614579));
#51049=CARTESIAN_POINT('Ctrl Pts',(-94.663801087988,-3.40777575822217,-1.70786592364882));
#51050=CARTESIAN_POINT('Ctrl Pts',(-94.4649275562905,-0.40544590980093,
-3.79016559608063));
#51051=CARTESIAN_POINT('Ctrl Pts',(-94.2660540245932,2.96940847303638,-2.39005333659048));
#51052=CARTESIAN_POINT('Ctrl Pts',(-94.0671804928955,3.61596425384286,1.20604483598993));
#51053=CARTESIAN_POINT('Ctrl Pts',(-93.8683069611984,0.940164653658382,
3.69402653692401));
#51054=CARTESIAN_POINT('Ctrl Pts',(-93.6694334295006,-2.59946016072173,
2.78792907088901));
#51055=CARTESIAN_POINT('Ctrl Pts',(-93.4705598978035,-3.75069564203049,
-0.679723349857117));
#51056=CARTESIAN_POINT('Ctrl Pts',(-93.2716863661057,-1.45578426624114,
-3.52284456109722));
#51057=CARTESIAN_POINT('Ctrl Pts',(-93.0728128344086,2.17670468249244,-3.12916895624107));
#51058=CARTESIAN_POINT('Ctrl Pts',(-92.8739393027108,3.80923289958397,0.139593510646091));
#51059=CARTESIAN_POINT('Ctrl Pts',(-92.6750657710136,1.94183010714438,3.28009717332813));
#51060=CARTESIAN_POINT('Ctrl Pts',(-92.476192239316,-1.70973017484599,3.40684081822274));
#51061=CARTESIAN_POINT('Ctrl Pts',(-92.2773187076186,-3.79038686164578,
0.403372124161483));
#51062=CARTESIAN_POINT('Ctrl Pts',(-92.0784451759211,-2.38842831726804,
-2.97071570581227));
#51063=CARTESIAN_POINT('Ctrl Pts',(-91.8795716442237,1.2080230691099,-3.61530384559662));
#51064=CARTESIAN_POINT('Ctrl Pts',(-91.6806981125261,3.69454037918903,-0.938143388842634));
#51065=CARTESIAN_POINT('Ctrl Pts',(-91.4818245808289,2.78650640297092,2.60098513984405));
#51066=CARTESIAN_POINT('Ctrl Pts',(-91.2829510491313,-0.681775377754059,
3.75032318151061));
#51067=CARTESIAN_POINT('Ctrl Pts',(-91.0840775174338,-3.52364054152792,
1.45385658356948));
#51068=CARTESIAN_POINT('Ctrl Pts',(-90.8852039857365,-3.12797754075145,
-2.17841642851909));
#51069=CARTESIAN_POINT('Ctrl Pts',(-90.6863304540388,0.141677647057878,
-3.80915595320164));
#51070=CARTESIAN_POINT('Ctrl Pts',(-90.4874569223416,3.28115912184763,-1.94003516684714));
#51071=CARTESIAN_POINT('Ctrl Pts',(-90.288583390644,3.40590485836977,1.71159391422753));
#51072=CARTESIAN_POINT('Ctrl Pts',(-90.0897098589466,0.401298217770733,
3.79060699254111));
#51073=CARTESIAN_POINT('Ctrl Pts',(-89.8908363272491,-2.97202204929068,
2.38680258295854));
#51074=CARTESIAN_POINT('Ctrl Pts',(-89.6919627955516,-3.61464235509244,
-1.21000094060259));
#51075=CARTESIAN_POINT('Ctrl Pts',(-89.4930892638543,-0.936121843189332,
-3.69505311547631));
#51076=CARTESIAN_POINT('Ctrl Pts',(-89.2942157321568,2.60250934034945,-2.78508290089926));
#51077=CARTESIAN_POINT('Ctrl Pts',(-89.0953422004592,3.74994959831413,0.683827201558385));
#51078=CARTESIAN_POINT('Ctrl Pts',(-88.896468668762,1.45192846567913,3.52443546714054));
#51079=CARTESIAN_POINT('Ctrl Pts',(-88.6975951370643,-2.18012752242672,
3.12678518888728));
#51080=CARTESIAN_POINT('Ctrl Pts',(-88.498721605367,-3.80907786653088,-0.143761741057804));
#51081=CARTESIAN_POINT('Ctrl Pts',(-88.2998480736696,-1.93823964579142,
-3.28222008813697));
#51082=CARTESIAN_POINT('Ctrl Pts',(-88.1009745419719,1.71345714123552,-3.40496787894343));
#51083=CARTESIAN_POINT('Ctrl Pts',(-87.9021010102748,3.79082598870071,-0.399224191249501));
#51084=CARTESIAN_POINT('Ctrl Pts',(-87.703227478577,2.38517613414864,2.97332750308055));
#51085=CARTESIAN_POINT('Ctrl Pts',(-87.5043539468798,-1.2119784498759,3.61397978252837));
#51086=CARTESIAN_POINT('Ctrl Pts',(-87.3054804151821,-3.69556474563236,
0.934100017303625));
#51087=CARTESIAN_POINT('Ctrl Pts',(-87.1066068834849,-2.78365856510014,
-2.60403276178164));
#51088=CARTESIAN_POINT('Ctrl Pts',(-86.9077333517873,0.685878820655876,
-3.74957489255291));
#51089=CARTESIAN_POINT('Ctrl Pts',(-86.70885982009,3.52522933769711,-1.44999991314728));
#51090=CARTESIAN_POINT('Ctrl Pts',(-86.5099862883923,3.12559190100552,2.1818379637031));
#51091=CARTESIAN_POINT('Ctrl Pts',(-86.311112756695,-0.145845792021992,
3.80899863959504));
#51092=CARTESIAN_POINT('Ctrl Pts',(-86.1122392249976,-3.28328007187856,
1.93644354451469));
#51093=CARTESIAN_POINT('Ctrl Pts',(-85.9133656932999,-3.40402988022421,
-1.71531985531219));
#51094=CARTESIAN_POINT('Ctrl Pts',(-85.7144921616027,-0.397150045218662,
-3.79104385005903));
#51095=CARTESIAN_POINT('Ctrl Pts',(-85.5156186299052,2.97463206679106,-2.38354897132526));
#51096=CARTESIAN_POINT('Ctrl Pts',(-85.3167450982077,3.61331612810275,1.21395559633781));
#51097=CARTESIAN_POINT('Ctrl Pts',(-85.1178715665104,0.932077911790798,
3.69607526950402));
#51098=CARTESIAN_POINT('Ctrl Pts',(-84.9189980348126,-2.60555540368459,
2.78223339599998));
#51099=CARTESIAN_POINT('Ctrl Pts',(-84.7201245031155,-3.74919906433912,
-0.687930234432375));
#51100=CARTESIAN_POINT('Ctrl Pts',(-84.5212509714179,-1.44807092655128,
-3.52602215295995));
#51101=CARTESIAN_POINT('Ctrl Pts',(-84.3223774397204,2.18354775183615,-3.1243976774634));
#51102=CARTESIAN_POINT('Ctrl Pts',(-84.123503908023,3.80891827241787,0.147929799326536));
#51103=CARTESIAN_POINT('Ctrl Pts',(-83.9246303763255,1.93464686355464,3.28433907275508));
#51104=CARTESIAN_POINT('Ctrl Pts',(-83.7257568446282,-1.71718205589994,
3.40309086249292));
#51105=CARTESIAN_POINT('Ctrl Pts',(-83.5268833129305,-3.79126057655081,
0.395075780299149));
#51106=CARTESIAN_POINT('Ctrl Pts',(-83.3280097812333,-2.38192109497551,
-2.97593574003171));
#51107=CARTESIAN_POINT('Ctrl Pts',(-83.1291362495355,1.21593237939653,-3.61265139201427));
#51108=CARTESIAN_POINT('Ctrl Pts',(-82.9302627178384,3.69658468693845,-0.930055527256101));
#51109=CARTESIAN_POINT('Ctrl Pts',(-82.7313891861407,2.78080739402538,2.60707726560248));
#51110=CARTESIAN_POINT('Ctrl Pts',(-82.5325156544434,-0.689981442273743,
3.74882211378524));
#51111=CARTESIAN_POINT('Ctrl Pts',(-82.3336421227459,-3.52681391269177,
1.44614150646857));
#51112=CARTESIAN_POINT('Ctrl Pts',(-82.1347685910484,-3.12320251861839,
-2.18525688631411));
#51113=CARTESIAN_POINT('Ctrl Pts',(-81.9358950593511,0.150013762347644,
-3.80883676502338));
#51114=CARTESIAN_POINT('Ctrl Pts',(-81.7370215276534,3.28539709044952,-1.93284960344911));
#51115=CARTESIAN_POINT('Ctrl Pts',(-81.5381479959562,3.40215082603064,1.7190437424413));
#51116=CARTESIAN_POINT('Ctrl Pts',(-81.3392744642585,0.393001397111847,
3.79147616811124));
#51117=CARTESIAN_POINT('Ctrl Pts',(-81.1404009325613,-2.97723852241226,
2.38029250558662));
#51118=CARTESIAN_POINT('Ctrl Pts',(-80.9415274008636,-3.61198557446186,
-1.21790879846029));
#51119=CARTESIAN_POINT('Ctrl Pts',(-80.7426538691663,-0.92803286430498,
-3.69709299778318));
#51120=CARTESIAN_POINT('Ctrl Pts',(-80.5437803374688,2.60859834707974,-2.77938055960323));
#51121=CARTESIAN_POINT('Ctrl Pts',(-80.3449068057714,3.74844404100414,0.692032443566012));
#51122=CARTESIAN_POINT('Ctrl Pts',(-80.1460332740739,1.44421165347667,3.52760461665555));
#51123=CARTESIAN_POINT('Ctrl Pts',(-79.9471597423764,-2.18696536662534,
3.12200642482824));
#51124=CARTESIAN_POINT('Ctrl Pts',(-79.748286210679,-3.80875411743601,-0.152097680461436));
#51125=CARTESIAN_POINT('Ctrl Pts',(-79.5494126789815,-1.9310517647361,-3.28645412464514));
#51126=CARTESIAN_POINT('Ctrl Pts',(-79.3505391472841,1.72090491437897,-3.40120977111878));
#51127=CARTESIAN_POINT('Ctrl Pts',(-79.1516656155866,3.79169062467575,-0.39092689627776));
#51128=CARTESIAN_POINT('Ctrl Pts',(-78.9527920838892,2.37866320364617,2.9785404135427));
#51129=CARTESIAN_POINT('Ctrl Pts',(-78.7539185521916,-1.21988485293742,
3.61131867564487));
#51130=CARTESIAN_POINT('Ctrl Pts',(-78.5550450204943,-3.69760020188601,
0.926009923542931));
#51131=CARTESIAN_POINT('Ctrl Pts',(-78.3561714887968,-2.77795289316067,
-2.61011864766102));
#51132=CARTESIAN_POINT('Ctrl Pts',(-78.1572979570994,0.694083237695167,
-3.74806484610899));
#51133=CARTESIAN_POINT('Ctrl Pts',(-77.9584244254018,3.52839426461459,-1.44228136815333));
#51134=CARTESIAN_POINT('Ctrl Pts',(-77.7595508937045,3.12080939645103,2.18867319225837));
#51135=CARTESIAN_POINT('Ctrl Pts',(-77.560677362007,-0.154181553044083,
3.80867032968048));
#51136=CARTESIAN_POINT('Ctrl Pts',(-77.3618038303095,-3.28751017502554,
1.92925334795383));
#51137=CARTESIAN_POINT('Ctrl Pts',(-77.1629302986122,-3.40026769803905,
-1.72276557115579));
#51138=CARTESIAN_POINT('Ctrl Pts',(-76.9640567669146,-0.388852278417899,
-3.79190394618015));
#51139=CARTESIAN_POINT('Ctrl Pts',(-76.7651832352172,2.9798414130333,-2.37703318964188));
#51140=CARTESIAN_POINT('Ctrl Pts',(-76.5663097035197,3.61065069576294,1.22186054223637));
#51141=CARTESIAN_POINT('Ctrl Pts',(-76.3674361718222,0.923986705575531,
3.69810629909514));
#51142=CARTESIAN_POINT('Ctrl Pts',(-76.1685626401249,-2.61163816689122,
2.77652439512505));
#51143=CARTESIAN_POINT('Ctrl Pts',(-75.9696891084273,-3.74768452921329,
-0.696133824047293));
#51144=CARTESIAN_POINT('Ctrl Pts',(-75.77081557673,-1.4403506510764,-3.52918285633249));
#51145=CARTESIAN_POINT('Ctrl Pts',(-75.5719420450324,2.19038036270197,-3.1196114338451));
#51146=CARTESIAN_POINT('Ctrl Pts',(-75.373068513335,3.80858540178188,0.156265379471771));
#51147=CARTESIAN_POINT('Ctrl Pts',(-75.1741949816376,1.92745435364065,3.28856524127456));
#51148=CARTESIAN_POINT('Ctrl Pts',(-74.9753214499401,-1.72462571221478,
3.39932460707347));
#51149=CARTESIAN_POINT('Ctrl Pts',(-74.7764479182427,-3.79211613256056,
0.386777544153313));
#51150=CARTESIAN_POINT('Ctrl Pts',(-74.5775743865451,-2.37540246406173,
-2.9811415204946));
#51151=CARTESIAN_POINT('Ctrl Pts',(-74.3787008548478,1.22383586576573,-3.60998163501602));
#51152=CARTESIAN_POINT('Ctrl Pts',(-74.1798273231502,3.69861128925905,-0.921963211008446));
#51153=CARTESIAN_POINT('Ctrl Pts',(-73.9809537914529,2.77509506592403,2.61315690431547));
#51154=CARTESIAN_POINT('Ctrl Pts',(-73.7820802597554,-0.698184202008545,
3.74730309043091));
#51155=CARTESIAN_POINT('Ctrl Pts',(-73.5832067280579,-3.52997039157319,
1.43841950282384));
#51156=CARTESIAN_POINT('Ctrl Pts',(-73.3843331963604,-3.11841253736907,
-2.19208687744507));
#51157=CARTESIAN_POINT('Ctrl Pts',(-73.185459664663,0.158349159120692,-3.80849933376564));
#51158=CARTESIAN_POINT('Ctrl Pts',(-72.9865861329655,3.28961932307638,-1.92565478233509));
#51159=CARTESIAN_POINT('Ctrl Pts',(-72.7877126012682,3.39838049850435,1.72648533699904));
#51160=CARTESIAN_POINT('Ctrl Pts',(-72.5888390695705,0.384702694105128,
3.79232718375349));
#51161=CARTESIAN_POINT('Ctrl Pts',(-72.3899655378733,-2.9824407355374,2.3737710273939));
#51162=CARTESIAN_POINT('Ctrl Pts',(-72.1910920061757,-3.60931149360442,
-1.22581082293416));
#51163=CARTESIAN_POINT('Ctrl Pts',(-71.9922184744782,-0.919939440447408,
-3.69911517222657));
#51164=CARTESIAN_POINT('Ctrl Pts',(-71.7933449427809,2.61467485947912,-2.77366490598547));
#51165=CARTESIAN_POINT('Ctrl Pts',(-71.5944714110833,3.74692052987602,0.700234370965129));
#51166=CARTESIAN_POINT('Ctrl Pts',(-71.3955978793859,1.43648792397377,3.53075687010093));
#51167=CARTESIAN_POINT('Ctrl Pts',(-71.1967243476885,-2.19379273597684,
3.11721270738183));
#51168=CARTESIAN_POINT('Ctrl Pts',(-70.997850815991,-3.80841212565751,-0.160432891367063));
#51169=CARTESIAN_POINT('Ctrl Pts',(-70.7989772842935,-1.92385463457588,
-3.29067242011544));
#51170=CARTESIAN_POINT('Ctrl Pts',(-70.6001037525962,1.72834444495199,-3.39743537261432));
#51171=CARTESIAN_POINT('Ctrl Pts',(-70.4012302208986,3.79253709969573,-0.382627728894362));
#51172=CARTESIAN_POINT('Ctrl Pts',(-70.2023566892013,2.3721388801267,2.98373905777277));
#51173=CARTESIAN_POINT('Ctrl Pts',(-70.0034831575037,-1.22778541315046,
3.60864027172874));
#51174=CARTESIAN_POINT('Ctrl Pts',(-69.8046096258063,-3.69961794784686,
0.91791539449824));
#51175=CARTESIAN_POINT('Ctrl Pts',(-69.6057360941088,-2.7722339157375,-2.61619203192775));
#51176=CARTESIAN_POINT('Ctrl Pts',(-69.4068625624114,0.702284330303311,
-3.74653684766316));
#51177=CARTESIAN_POINT('Ctrl Pts',(-69.2079890307139,3.53154229168029,-1.43455591510438));
#51178=CARTESIAN_POINT('Ctrl Pts',(-69.0091154990165,3.11601194424255,2.19549793778661));
#51179=CARTESIAN_POINT('Ctrl Pts',(-68.810241967319,-0.162516575587105,
3.8083237774836));
#51180=CARTESIAN_POINT('Ctrl Pts',(-68.6113684356216,-3.29172453207651,
1.92205391090189));
#51181=CARTESIAN_POINT('Ctrl Pts',(-68.4124949039241,-3.3964892296863,-1.73020303551702));
#51182=CARTESIAN_POINT('Ctrl Pts',(-68.2136213722266,-0.380552649142222,
-3.79274588032446));
#51183=CARTESIAN_POINT('Ctrl Pts',(-68.0147478405293,2.98503648681207,-2.37050602274877));
#51184=CARTESIAN_POINT('Ctrl Pts',(-67.8158743088317,3.6079679695899,1.22975963582352));
#51185=CARTESIAN_POINT('Ctrl Pts',(-67.6170007771343,0.915891073766863,
3.70011961596942));
#51186=CARTESIAN_POINT('Ctrl Pts',(-67.4181272454368,-2.61770842120721,
2.77080209560849));
#51187=CARTESIAN_POINT('Ctrl Pts',(-67.2192537137395,-3.74615204390717,
-0.70433407940944));
#51188=CARTESIAN_POINT('Ctrl Pts',(-67.0203801820419,-1.43262347679405,
-3.53232665607612));
#51189=CARTESIAN_POINT('Ctrl Pts',(-66.8215066503446,2.19720248236392,-3.11481024831069));
#51190=CARTESIAN_POINT('Ctrl Pts',(-66.6226331186469,3.80823428927037,0.164600211157061));
#51191=CARTESIAN_POINT('Ctrl Pts',(-66.4237595869497,1.92025261185217,3.29277565864461));
#51192=CARTESIAN_POINT('Ctrl Pts',(-66.2248860552521,-1.73206110813779,
3.39554207000353));
#51193=CARTESIAN_POINT('Ctrl Pts',(-66.0260125235547,-3.79295352557719,
0.378477455469882));
#51194=CARTESIAN_POINT('Ctrl Pts',(-65.8271389918571,-2.3688724557489,-2.98633302226689));
#51195=CARTESIAN_POINT('Ctrl Pts',(-65.6282654601599,1.23173349036234,-3.60729458738919));
#51196=CARTESIAN_POINT('Ctrl Pts',(-65.4293919284621,3.70062017644406,-0.913866478859252));
#51197=CARTESIAN_POINT('Ctrl Pts',(-65.230518396765,2.76936944602707,2.61922402686354));
#51198=CARTESIAN_POINT('Ctrl Pts',(-65.0316448650673,-0.706383617669903,
3.74576611872324));
#51199=CARTESIAN_POINT('Ctrl Pts',(-64.83277133337,-3.53310996305364,1.43069060962126));
#51200=CARTESIAN_POINT('Ctrl Pts',(-64.6338978016725,-3.11360761994599,
-2.19890636919852));
#51201=CARTESIAN_POINT('Ctrl Pts',(-64.435024269975,0.16668379745318,-3.80814366104459));
#51202=CARTESIAN_POINT('Ctrl Pts',(-64.2361507382776,3.2938257995051,-1.91845073796596));
#51203=CARTESIAN_POINT('Ctrl Pts',(-64.0372772065801,3.39459389384955,1.73391866225805));
#51204=CARTESIAN_POINT('Ctrl Pts',(-63.8384036748827,0.376402148498568,
3.79316003539174));
#51205=CARTESIAN_POINT('Ctrl Pts',(-63.6395301431853,-2.98762866374912,
2.3672381796161));
#51206=CARTESIAN_POINT('Ctrl Pts',(-63.4406566114878,-3.60662012532815,
-1.23370697617605));
#51207=CARTESIAN_POINT('Ctrl Pts',(-63.2417830797903,-0.911841610381489,
-3.70111962912095));
#51208=CARTESIAN_POINT('Ctrl Pts',(-63.0429095480929,2.62073884844303,-2.7679359674221));
#51209=CARTESIAN_POINT('Ctrl Pts',(-62.8440360163953,3.74537907222691,0.708432944471117));
#51210=CARTESIAN_POINT('Ctrl Pts',(-62.6451624846981,1.42875731416466,3.53389221237837));
#51211=CARTESIAN_POINT('Ctrl Pts',(-62.4462889530004,-2.20060959778032,
3.11240405950844));
#51212=CARTESIAN_POINT('Ctrl Pts',(-62.2474154213031,-3.80805189283341,
-0.168767333851733));
#51213=CARTESIAN_POINT('Ctrl Pts',(-62.0485418896055,-1.91664828978265,
-3.29487495434361));
#51214=CARTESIAN_POINT('Ctrl Pts',(-61.8496683579083,1.73577569732174,-3.39364470150818));
#51215=CARTESIAN_POINT('Ctrl Pts',(-61.6507948262106,3.79336540970629,-0.374326728849534));
#51216=CARTESIAN_POINT('Ctrl Pts',(-61.4519212945133,2.36560319483962,2.9889234108709));
#51217=CARTESIAN_POINT('Ctrl Pts',(-61.2530477628157,-1.23568009267388,
3.6059445836087));
#51218=CARTESIAN_POINT('Ctrl Pts',(-61.0541742311184,-3.70161797385057,
0.909816468939726));
#51219=CARTESIAN_POINT('Ctrl Pts',(-60.8553006994208,-2.76650166022269,
-2.62225288549229));
#51220=CARTESIAN_POINT('Ctrl Pts',(-60.6564271677235,0.71048205919978,-3.74499090453405));
#51221=CARTESIAN_POINT('Ctrl Pts',(-60.4575536360259,3.53467340381617,-1.42682359100281));
#51222=CARTESIAN_POINT('Ctrl Pts',(-60.2586801043286,3.1111995673583,2.20231216759956));
#51223=CARTESIAN_POINT('Ctrl Pts',(-60.059806572631,-0.170850819729117,
3.80795898466428));
#51224=CARTESIAN_POINT('Ctrl Pts',(-59.8609330409336,-3.29592312284612,
1.91484526784171));
#51225=CARTESIAN_POINT('Ctrl Pts',(-59.6620595092362,-3.39269449326354,
-1.73763221277302));
#51226=CARTESIAN_POINT('Ctrl Pts',(-59.4631859775387,-0.372251197144022,
-3.79356964845936));
#51227=CARTESIAN_POINT('Ctrl Pts',(-59.2643124458413,2.99021726324463,-2.36396750190888));
#51228=CARTESIAN_POINT('Ctrl Pts',(-59.0654389141438,3.60526796243309,1.23765283926516));
#51229=CARTESIAN_POINT('Ctrl Pts',(-58.8665653824463,0.90779105514019,3.70211521048372));
#51230=CARTESIAN_POINT('Ctrl Pts',(-58.6676918507489,-2.62376613755799,
2.76506652485823));
#51231=CARTESIAN_POINT('Ctrl Pts',(-58.4688183190513,-3.74460161576084,
-0.712530961242275));
#51232=CARTESIAN_POINT('Ctrl Pts',(-58.2699447873541,-1.42488944071483,
-3.53545353713309));
#51233=CARTESIAN_POINT('Ctrl Pts',(-58.0710712556564,2.20401407814638,-3.10999414385624));
#51234=CARTESIAN_POINT('Ctrl Pts',(-57.8721977239591,3.80786493656502,0.172934254461413));
#51235=CARTESIAN_POINT('Ctrl Pts',(-57.6733241922616,1.9130416726831,3.29697030469875));
#51236=CARTESIAN_POINT('Ctrl Pts',(-57.4744506605642,-1.73948820805607,
3.39174326940018));
#51237=CARTESIAN_POINT('Ctrl Pts',(-57.2755771288667,-3.79377275158988,
0.37017555400328));
#51238=CARTESIAN_POINT('Ctrl Pts',(-57.0767035971692,-2.3623311013134,-2.99151022048307));
#51239=CARTESIAN_POINT('Ctrl Pts',(-56.8778300654718,1.23962521535938,-3.60459026200378));
#51240=CARTESIAN_POINT('Ctrl Pts',(-56.6789565337743,3.70261133887159,-0.905765369589214));
#51241=CARTESIAN_POINT('Ctrl Pts',(-56.4800830020769,2.76363056175831,2.62527860418717));
#51242=CARTESIAN_POINT('Ctrl Pts',(-56.2812094703794,-0.714579649985331,
3.74421120602382));
#51243=CARTESIAN_POINT('Ctrl Pts',(-56.082335938682,-3.53623261209566,1.4229548638796));
#51244=CARTESIAN_POINT('Ctrl Pts',(-55.8834624069845,-3.10878778936306,
-2.20571532891139));
#51245=CARTESIAN_POINT('Ctrl Pts',(-55.6845888752871,0.175017637425035,
-3.80776974856381));
#51246=CARTESIAN_POINT('Ctrl Pts',(-55.4857153435897,3.29801649958808,-1.9112375048466));
#51247=CARTESIAN_POINT('Ctrl Pts',(-55.2868418118921,3.39079103020278,1.74134368261521));
#51248=CARTESIAN_POINT('Ctrl Pts',(-55.0879682801948,0.368099800048924,
3.79397471903694));
#51249=CARTESIAN_POINT('Ctrl Pts',(-54.8890947484972,-2.99280228219903,
2.36069399354332));
#51250=CARTESIAN_POINT('Ctrl Pts',(-54.6902212167998,-3.60391148252377,
-1.24159722036601));
#51251=CARTESIAN_POINT('Ctrl Pts',(-54.4913476851023,-0.90373941289318,
-3.70310635886562));
#51252=CARTESIAN_POINT('Ctrl Pts',(-54.2924741534049,2.62679028492706,-2.76219377135282));
#51253=CARTESIAN_POINT('Ctrl Pts',(-54.0936006217074,3.74381967543987,0.71662812481567));
#51254=CARTESIAN_POINT('Ctrl Pts',(-53.89472709001,1.42101986107626,3.53701062847065));
#51255=CARTESIAN_POINT('Ctrl Pts',(-53.6958535583125,-2.20741591938532,
3.10758050423988));
#51256=CARTESIAN_POINT('Ctrl Pts',(-53.4969800266151,-3.80767342068911,
-0.177100967996319));
#51257=CARTESIAN_POINT('Ctrl Pts',(-53.2981064949176,-1.90943276487233,
-3.29906170720093));
#51258=CARTESIAN_POINT('Ctrl Pts',(-53.0992329632202,1.74319863589507,-3.38983777595641));
#51259=CARTESIAN_POINT('Ctrl Pts',(-52.9003594315227,3.79417555074013,-0.366023935902194));
#51260=CARTESIAN_POINT('Ctrl Pts',(-52.7014858998253,2.35905617908858,2.99409344800579));
#51261=CARTESIAN_POINT('Ctrl Pts',(-52.5026123681278,-1.24356885369478,
3.60323162419618));
#51262=CARTESIAN_POINT('Ctrl Pts',(-52.3037388364304,-3.70360027031765,
0.901713185658582));
#51263=CARTESIAN_POINT('Ctrl Pts',(-52.1048653047329,-2.76075615407185,
-2.62830117932514));
#51264=CARTESIAN_POINT('Ctrl Pts',(-51.9059917730355,0.718676385120064,
-3.74342702412619));
#51265=CARTESIAN_POINT('Ctrl Pts',(-51.707118241338,3.53778758602515,-1.41908443288405));
#51266=CARTESIAN_POINT('Ctrl Pts',(-51.5082447096405,3.10637228884811,2.2091158490591));
#51267=CARTESIAN_POINT('Ctrl Pts',(-51.3093711779431,-0.179184245551611,
3.80757595296977));
#51268=CARTESIAN_POINT('Ctrl Pts',(-51.1104976462456,-3.3001059272244,1.90762745330053));
#51269=CARTESIAN_POINT('Ctrl Pts',(-50.9116241145482,-3.38888350694643,
-1.74505306734036));
#51270=CARTESIAN_POINT('Ctrl Pts',(-50.7127505828507,-0.363947962184506,
-3.79437524663933));
#51271=CARTESIAN_POINT('Ctrl Pts',(-50.5138770511533,2.99538371751683,-2.35741765843947));
#51272=CARTESIAN_POINT('Ctrl Pts',(-50.3150035194558,3.60255068722456,1.24554011475546));
#51273=CARTESIAN_POINT('Ctrl Pts',(-50.1161299877584,0.899686688491969,
3.70409307307982));
#51274=CARTESIAN_POINT('Ctrl Pts',(-49.9172564560609,-2.62981128692911,
2.75931771034576));
#51275=CARTESIAN_POINT('Ctrl Pts',(-49.7183829243635,-3.74303325220033,
-0.720724430285355));
#51276=CARTESIAN_POINT('Ctrl Pts',(-49.519509392666,-1.41714857988236,-3.53856348452659));
#51277=CARTESIAN_POINT('Ctrl Pts',(-49.3206358609686,2.21081511742383,-3.10516314354943));
#51278=CARTESIAN_POINT('Ctrl Pts',(-49.1217623292711,3.80747734543496,0.181267469467265));
#51279=CARTESIAN_POINT('Ctrl Pts',(-48.9228887975737,1.90582157067163,3.30114915934591));
#51280=CARTESIAN_POINT('Ctrl Pts',(-48.7240152658761,-1.74690697639595,
3.3879282234585));
#51281=CARTESIAN_POINT('Ctrl Pts',(-48.5251417341788,-3.79457380667476,
0.361871879517312));
#51282=CARTESIAN_POINT('Ctrl Pts',(-48.3262682024813,-2.35577843208649,
-2.99667309034592));
#51283=CARTESIAN_POINT('Ctrl Pts',(-48.1273946707838,1.24751100295795,-3.60186867181274));
#51284=CARTESIAN_POINT('Ctrl Pts',(-47.9285211390864,3.7045847670046,-0.897659921999986));
#51285=CARTESIAN_POINT('Ctrl Pts',(-47.7296476073888,2.75787844060516,2.63132060728692));
#51286=CARTESIAN_POINT('Ctrl Pts',(-47.5307740756916,-0.722772259698463,
3.74263835978015));
#51287=CARTESIAN_POINT('Ctrl Pts',(-47.3319005439939,-3.53933832374268,
1.41521230265069));
#51288=CARTESIAN_POINT('Ctrl Pts',(-47.1330270122967,-3.10395306870581,
-2.21251372397084));
#51289=CARTESIAN_POINT('Ctrl Pts',(-46.934153480599,0.183350639119669,-3.80737759811421));
#51290=CARTESIAN_POINT('Ctrl Pts',(-46.7352799489018,3.30219140325315,-1.90401511752624));
#51291=CARTESIAN_POINT('Ctrl Pts',(-46.5364064172041,3.3869719257786,1.74876036250685));
#51292=CARTESIAN_POINT('Ctrl Pts',(-46.3375328855069,0.3597956885221,3.79477123078697));
#51293=CARTESIAN_POINT('Ctrl Pts',(-46.1386593538092,-2.99796156610706,
2.35413850052034));
#51294=CARTESIAN_POINT('Ctrl Pts',(-45.9397858221119,-3.60118557816487,
-1.24948151771226));
#51295=CARTESIAN_POINT('Ctrl Pts',(-45.7409122904144,-0.895632886789359,
-3.7050753519448));
#51296=CARTESIAN_POINT('Ctrl Pts',(-45.5420387587169,2.63282913994673,-2.7564383452809));
#51297=CARTESIAN_POINT('Ctrl Pts',(-45.3431652270195,3.74224234698389,0.724819872746352));
#51298=CARTESIAN_POINT('Ctrl Pts',(-45.144291695322,1.41327560176868,3.54011210344149));
#51299=CARTESIAN_POINT('Ctrl Pts',(-44.9454181636246,-2.21421166819163,
3.10274206467949));
#51300=CARTESIAN_POINT('Ctrl Pts',(-44.7465446319271,-3.80727671103737,
-0.185433753885211));
#51301=CARTESIAN_POINT('Ctrl Pts',(-44.5476711002297,-1.90220809440512,
-3.30323265863413));
#51302=CARTESIAN_POINT('Ctrl Pts',(-44.3487975685321,1.75061322511827,-3.386014614193));
#51303=CARTESIAN_POINT('Ctrl Pts',(-44.1499240368348,3.79496751891687,-0.357719389820383));
#51304=CARTESIAN_POINT('Ctrl Pts',(-43.9510505051372,2.35249786423195,2.99924914441454));
#51305=CARTESIAN_POINT('Ctrl Pts',(-43.7521769734399,-1.2514516584285,3.60050140648546));
#51306=CARTESIAN_POINT('Ctrl Pts',(-43.5533034417424,-3.70556482775357,
0.893605583466879));
#51307=CARTESIAN_POINT('Ctrl Pts',(-43.3544299100449,-2.75499742480407,
-2.63433688445697));
#51308=CARTESIAN_POINT('Ctrl Pts',(-43.1555563783475,0.726867268816058,
-3.74184521393008));
#51309=CARTESIAN_POINT('Ctrl Pts',(-42.95668284665,3.54088482339137,-1.41133847781607));
#51310=CARTESIAN_POINT('Ctrl Pts',(-42.7578093149525,3.10153013183299,2.21590894957792));
#51311=CARTESIAN_POINT('Ctrl Pts',(-42.5589357832551,-0.187516813140302,
3.80717468423465));
#51312=CARTESIAN_POINT('Ctrl Pts',(-42.3600622515577,-3.30427292517715,
1.90040050184921));
#51313=CARTESIAN_POINT('Ctrl Pts',(-42.1611887198602,-3.38505628898826,
-1.75246556367551));
#51314=CARTESIAN_POINT('Ctrl Pts',(-41.9623151881627,-0.355642984033713,
-3.7951626710057));
#51315=CARTESIAN_POINT('Ctrl Pts',(-41.7634416564653,3.00053582488292,-2.35085652371245));
#51316=CARTESIAN_POINT('Ctrl Pts',(-41.5645681247678,3.59981615697931,1.2534214245169));
#51317=CARTESIAN_POINT('Ctrl Pts',(-41.3656945930704,0.891578012639441,
3.70605319428438));
#51318=CARTESIAN_POINT('Ctrl Pts',(-41.1668210613729,-2.63584384036628,
2.75355567960603));
#51319=CARTESIAN_POINT('Ctrl Pts',(-40.9679475296755,-3.7414469607376,-0.72891444729469));
#51320=CARTESIAN_POINT('Ctrl Pts',(-40.7690739979781,-1.40940093137277,
-3.54165648336101));
#51321=CARTESIAN_POINT('Ctrl Pts',(-40.5702004662805,2.21760556762163,-3.10031727052911));
#51322=CARTESIAN_POINT('Ctrl Pts',(-40.3713269345832,3.80707151773659,0.189599816261364));
#51323=CARTESIAN_POINT('Ctrl Pts',(-40.1724534028856,1.89859234039963,3.30531220257079));
#51324=CARTESIAN_POINT('Ctrl Pts',(-39.9735798711882,-1.75431737762409,
3.38409695045128));
#51325=CARTESIAN_POINT('Ctrl Pts',(-39.7747063394907,-3.79535668699504,
0.353566471783673));
#51326=CARTESIAN_POINT('Ctrl Pts',(-39.5758328077933,-2.34921447945318,
-3.00182160712704));
#51327=CARTESIAN_POINT('Ctrl Pts',(-39.3769592760958,1.25539081538779,-3.59912982985154));
#51328=CARTESIAN_POINT('Ctrl Pts',(-39.1780857443985,3.70654045139103,-0.889550174914005));
#51329=CARTESIAN_POINT('Ctrl Pts',(-38.9792122127009,2.75211311011837,2.63735000722356));
#51330=CARTESIAN_POINT('Ctrl Pts',(-38.7803386810035,-0.73096140756941,
3.74104758752567));
#51331=CARTESIAN_POINT('Ctrl Pts',(-38.581465149306,-3.54242708311941,1.40746296301879));
#51332=CARTESIAN_POINT('Ctrl Pts',(-38.3825916176086,-3.09910348113092,
-2.21930152181486));
#51333=CARTESIAN_POINT('Ctrl Pts',(-38.1837180859111,0.191682762624847,
-3.80696721157406));
#51334=CARTESIAN_POINT('Ctrl Pts',(-37.9848445542137,3.30635049050394,-1.89678361059766));
#51335=CARTESIAN_POINT('Ctrl Pts',(-37.7859710225162,3.38313659886923,1.75616866640966));
#51336=CARTESIAN_POINT('Ctrl Pts',(-37.5870974908188,0.351489853691939,
3.79554956682676));
#51337=CARTESIAN_POINT('Ctrl Pts',(-37.3882239591213,-3.00310649076192,
2.34757173194576));
#51338=CARTESIAN_POINT('Ctrl Pts',(-37.1893504274238,-3.59844242530768,
-1.2573598304516));
#51339=CARTESIAN_POINT('Ctrl Pts',(-36.9904768957264,-0.887522070897608,
-3.70702659892766));
#51340=CARTESIAN_POINT('Ctrl Pts',(-36.7916033640289,2.63885538457792,-2.75066971677293));
#51341=CARTESIAN_POINT('Ctrl Pts',(-36.5927298323315,3.74064709441386,0.733008149027457));
#51342=CARTESIAN_POINT('Ctrl Pts',(-36.393856300634,1.40552457333426,3.54319662243588));
#51343=CARTESIAN_POINT('Ctrl Pts',(-36.1949827689366,-2.22099681164992,
3.09788876400177));
#51344=CARTESIAN_POINT('Ctrl Pts',(-35.9961092372391,-3.80686176577831,
-0.19376565160721));
#51345=CARTESIAN_POINT('Ctrl Pts',(-35.7972357055417,-1.89497431298474,
-3.30738778866578));
#51346=CARTESIAN_POINT('Ctrl Pts',(-35.5983621738442,1.75801942947801,-3.3821752345296));
#51347=CARTESIAN_POINT('Ctrl Pts',(-35.3994886421468,3.79574131044322,-0.34941313038003));
#51348=CARTESIAN_POINT('Ctrl Pts',(-35.2006151104493,2.34592828168183,3.00439047540306));
#51349=CARTESIAN_POINT('Ctrl Pts',(-35.0017415787519,-1.25932846911898,
3.59775394355339));
#51350=CARTESIAN_POINT('Ctrl Pts',(-34.8028680470544,-3.70751163674873,
0.885493701197379));
#51351=CARTESIAN_POINT('Ctrl Pts',(-34.603994515357,-2.74922550000179,-2.64035997197872));
#51352=CARTESIAN_POINT('Ctrl Pts',(-34.4051209836595,0.735054671056124,
-3.74024548152205));
#51353=CARTESIAN_POINT('Ctrl Pts',(-34.206247451962,3.54396510108007,-1.40358576289945));
#51354=CARTESIAN_POINT('Ctrl Pts',(-34.0073739202646,3.09667311950531,2.22269143661931));
#51355=CARTESIAN_POINT('Ctrl Pts',(-33.8085003885672,-0.195848482584929,
3.80675518038088));
#51356=CARTESIAN_POINT('Ctrl Pts',(-33.6096268568697,-3.30842409674581,
1.8931644481025));
#51357=CARTESIAN_POINT('Ctrl Pts',(-33.4107533251723,-3.38121285772017,
-1.75986966627512));
#51358=CARTESIAN_POINT('Ctrl Pts',(-33.2118797934747,-0.347336302469681,
-3.79593191778697));
#51359=CARTESIAN_POINT('Ctrl Pts',(-33.0130062617774,3.005673560666,-2.34428412915341));
#51360=CARTESIAN_POINT('Ctrl Pts',(-32.8141327300798,3.59706438479482,1.26129673080056));
#51361=CARTESIAN_POINT('Ctrl Pts',(-32.6152591983825,0.883465066420513,
3.70799556470907));
#51362=CARTESIAN_POINT('Ctrl Pts',(-32.4163856666849,-2.64186376897555,
2.74778046023728));
#51363=CARTESIAN_POINT('Ctrl Pts',(-32.2175121349875,-3.73984274897046,
-0.737100973042777));
#51364=CARTESIAN_POINT('Ctrl Pts',(-32.0186386032901,-1.40164653229475,
-3.54473251882192));
#51365=CARTESIAN_POINT('Ctrl Pts',(-31.8197650715926,2.22438539621574,-3.09545654800542));
#51366=CARTESIAN_POINT('Ctrl Pts',(-31.6208915398952,3.8066474554137,0.1979312549345));
#51367=CARTESIAN_POINT('Ctrl Pts',(-31.4220180081977,1.89135401649272,3.30945941443378));
#51368=CARTESIAN_POINT('Ctrl Pts',(-31.2231444765003,-1.7617193762471,3.38024946872905));
#51369=CARTESIAN_POINT('Ctrl Pts',(-31.0242709448028,-3.79612138880096,
0.345259370582608));
#51370=CARTESIAN_POINT('Ctrl Pts',(-30.8253974131054,-2.34263927485271,
-3.00695574616668));
#51371=CARTESIAN_POINT('Ctrl Pts',(-30.6265238814079,1.26326461490713,-3.59637374923839));
#51372=CARTESIAN_POINT('Ctrl Pts',(-30.4276503497104,3.70847838266379,-0.881436167174301));
#51373=CARTESIAN_POINT('Ctrl Pts',(-30.228776818013,2.74633459791199,2.64336677511825));
#51374=CARTESIAN_POINT('Ctrl Pts',(-30.0299032863155,-0.739147054374844,
3.73943889687965));
#51375=CARTESIAN_POINT('Ctrl Pts',(-29.8310297546182,-3.5454988754317,1.39970688210069));
#51376=CARTESIAN_POINT('Ctrl Pts',(-29.6321562229205,-3.09423904986631,
-2.22607868993213));
#51377=CARTESIAN_POINT('Ctrl Pts',(-29.4332826912232,0.200013968032432,
-3.80653859090899));
#51378=CARTESIAN_POINT('Ctrl Pts',(-29.2344091595257,3.31049374141978,-1.88954301869738));
#51379=CARTESIAN_POINT('Ctrl Pts',(-29.0355356278283,3.37928506784462,1.76356855884025));
#51380=CARTESIAN_POINT('Ctrl Pts',(-28.8366620961308,0.343182335340544,
3.79630972342846));
#51381=CARTESIAN_POINT('Ctrl Pts',(-28.6377885644334,-3.00823703152125,
2.3409937192721));
#51382=CARTESIAN_POINT('Ctrl Pts',(-28.4389150327359,-3.59568203709087,
-1.2652321208496));
#51383=CARTESIAN_POINT('Ctrl Pts',(-28.2400415010384,-0.879407004066094,
-3.70896009046836));
#51384=CARTESIAN_POINT('Ctrl Pts',(-28.041167969341,2.64486898995689,-2.74488791345875));
#51385=CARTESIAN_POINT('Ctrl Pts',(-27.8422944376435,3.73903392537052,0.741192914439823));
#51386=CARTESIAN_POINT('Ctrl Pts',(-27.6434209059461,1.3977668128979,3.54626417068001));
#51387=CARTESIAN_POINT('Ctrl Pts',(-27.4445473742486,-2.22777131726157,
3.09302062545243));
#51388=CARTESIAN_POINT('Ctrl Pts',(-27.2456738425512,-3.80642858689937,
-0.202096621255259));
#51389=CARTESIAN_POINT('Ctrl Pts',(-27.0468003108537,-1.88773145525861,
-3.31152707739417));
#51390=CARTESIAN_POINT('Ctrl Pts',(-26.8479267791563,1.765417213501,-3.37831965535559));
#51391=CARTESIAN_POINT('Ctrl Pts',(-26.6490532474588,3.79649692161308,-0.341105197365262));
#51392=CARTESIAN_POINT('Ctrl Pts',(-26.4501797157614,2.33934746290421,3.00951741634616));
#51393=CARTESIAN_POINT('Ctrl Pts',(-26.2513061840639,-1.26719924803898,
3.5949892485593));
#51394=CARTESIAN_POINT('Ctrl Pts',(-26.0524326523664,-3.70944068797857,
0.877377577703335));
#51395=CARTESIAN_POINT('Ctrl Pts',(-25.853559120669,-2.74344040731062,-2.64637041304177));
#51396=CARTESIAN_POINT('Ctrl Pts',(-25.6546855889715,0.74323855262528,-3.73862783456431));
#51397=CARTESIAN_POINT('Ctrl Pts',(-25.4558120572741,3.54702840433774,-1.39582632526716));
#51398=CARTESIAN_POINT('Ctrl Pts',(-25.2569385255766,3.09180127512853,2.22946327769737));
#51399=CARTESIAN_POINT('Ctrl Pts',(-25.0580649938792,-0.204179213979529,
3.80631744341775));
#51400=CARTESIAN_POINT('Ctrl Pts',(-24.8591914621818,-3.31255942204762,
1.88591932671869));
#51401=CARTESIAN_POINT('Ctrl Pts',(-24.6603179304842,-3.37735323155094,
-1.76726533967594));
#51402=CARTESIAN_POINT('Ctrl Pts',(-24.4614443987868,-0.339027957278562,
-3.79668298329881));
#51403=CARTESIAN_POINT('Ctrl Pts',(-24.2625708670894,3.01079690025812,-2.33770050624184));
#51404=CARTESIAN_POINT('Ctrl Pts',(-24.0636973353919,3.59429538385108,1.26916599588641));
#51405=CARTESIAN_POINT('Ctrl Pts',(-23.8648238036945,0.87534788869354,3.70992017505057));
#51406=CARTESIAN_POINT('Ctrl Pts',(-23.665950271997,-2.64787104392343,2.74199207990092));
#51407=CARTESIAN_POINT('Ctrl Pts',(-23.4670767402996,-3.73822062458257,
-0.745283968318842));
#51408=CARTESIAN_POINT('Ctrl Pts',(-23.2682032086021,-1.39388541978934,
-3.54779157617611));
#51409=CARTESIAN_POINT('Ctrl Pts',(-23.0693296769047,2.23115457073302,-3.09058099925963));
#51410=CARTESIAN_POINT('Ctrl Pts',(-22.8704561452071,3.8062051604974,0.206261745581809));
#51411=CARTESIAN_POINT('Ctrl Pts',(-22.6715826135097,1.8841066336201,3.31359077507109));
#51412=CARTESIAN_POINT('Ctrl Pts',(-22.4727090818123,-1.76911293681183,
3.37638579672));
#51413=CARTESIAN_POINT('Ctrl Pts',(-22.2738355501148,-3.79686790842993,
0.336950615702276));
#51414=CARTESIAN_POINT('Ctrl Pts',(-22.0749620184174,-2.33605284977801,
-3.01207548287411));
#51415=CARTESIAN_POINT('Ctrl Pts',(-21.8760884867199,1.27113236380313,-3.59360044317391));
#51416=CARTESIAN_POINT('Ctrl Pts',(-21.6772149550225,3.71039855154082,-0.873317937644316));
#51417=CARTESIAN_POINT('Ctrl Pts',(-21.478341423325,2.74054293166321,2.64937088215266));
#51418=CARTESIAN_POINT('Ctrl Pts',(-21.2794678916276,-0.747329160908197,
3.73781229554719));
#51419=CARTESIAN_POINT('Ctrl Pts',(-21.0805943599301,-3.54855368596668,
1.39194409704549));
#51420=CARTESIAN_POINT('Ctrl Pts',(-20.8817208282327,-3.08935979821102,
-2.23284519586224));
#51421=CARTESIAN_POINT('Ctrl Pts',(-20.6828472965351,0.20834421543868,-3.80609173817195));
#51422=CARTESIAN_POINT('Ctrl Pts',(-20.4839737648378,3.31462113615585,-1.88229337650549));
#51423=CARTESIAN_POINT('Ctrl Pts',(-20.2851002331403,3.37541735115235,1.77096000435559));
#51424=CARTESIAN_POINT('Ctrl Pts',(-20.0862267014428,0.334873173258265,
3.79705169695109));
#51425=CARTESIAN_POINT('Ctrl Pts',(-19.8873531697454,-3.01335316381137,
2.33440449400597));
#51426=CARTESIAN_POINT('Ctrl Pts',(-19.6884796380479,-3.59290442673585,
-1.27309835120051));
#51427=CARTESIAN_POINT('Ctrl Pts',(-19.4896061063505,-0.871287725163321,
-3.71087581730611));
#51428=CARTESIAN_POINT('Ctrl Pts',(-19.290732574653,2.65086992728046,-2.7390929630313));
#51429=CARTESIAN_POINT('Ctrl Pts',(-19.0918590429556,3.73740284758043,0.749374129781112));
#51430=CARTESIAN_POINT('Ctrl Pts',(-18.8929855112581,1.39000235761673,3.5493147334813));
#51431=CARTESIAN_POINT('Ctrl Pts',(-18.6941119795607,-2.23453515257893,
3.08813767234826));
#51432=CARTESIAN_POINT('Ctrl Pts',(-18.4952384478632,-3.80597717647534,
-0.210426622926742));
#51433=CARTESIAN_POINT('Ctrl Pts',(-18.2963649161657,-1.88047955591764,
-3.31565050499345));
#51434=CARTESIAN_POINT('Ctrl Pts',(-18.0974913844683,1.7728065417542,-3.37444789513792));
#51435=CARTESIAN_POINT('Ctrl Pts',(-17.8986178527708,3.79723434880727,-0.332795630568509));
#51436=CARTESIAN_POINT('Ctrl Pts',(-17.6997443210734,2.33275543941922,3.01462994268742));
#51437=CARTESIAN_POINT('Ctrl Pts',(-17.5008707893759,-1.27506395749001,
3.59220733474523));
#51438=CARTESIAN_POINT('Ctrl Pts',(-17.3019972576785,-3.71135197220356,
0.869257251858322));
#51439=CARTESIAN_POINT('Ctrl Pts',(-17.103123725981,-2.73764217443926,-2.65236817885809));
#51440=CARTESIAN_POINT('Ctrl Pts',(-16.9042501942836,0.75141887432542,-3.73699228080485));
#51441=CARTESIAN_POINT('Ctrl Pts',(-16.7053766625861,3.55007471849215,-1.38806020208435));
#51442=CARTESIAN_POINT('Ctrl Pts',(-16.5065031308886,3.08691462203722,2.23622444037719));
#51443=CARTESIAN_POINT('Ctrl Pts',(-16.3076295991912,-0.212508967422626,
3.80586147544186));
#51444=CARTESIAN_POINT('Ctrl Pts',(-16.1087560674937,-3.31667888127574,
1.87866517239955));
#51445=CARTESIAN_POINT('Ctrl Pts',(-15.9098825357963,-3.37347742896691,
-1.77465254845506));
#51446=CARTESIAN_POINT('Ctrl Pts',(-15.7110090040988,-0.330717988254753,
-3.79741586394379));
#51447=CARTESIAN_POINT('Ctrl Pts',(-15.5121354724014,3.01590581912008,-2.33110568651127));
#51448=CARTESIAN_POINT('Ctrl Pts',(-15.3132619407039,3.59150916741074,1.27702918208321));
#51449=CARTESIAN_POINT('Ctrl Pts',(-15.1143884090065,0.867226518337144,
3.71182701609064));
#51450=CARTESIAN_POINT('Ctrl Pts',(-14.915514877309,-2.65386563643705,2.73619056632137));
#51451=CARTESIAN_POINT('Ctrl Pts',(-14.7166413456116,-3.73658059534335,
-0.753463393929017));
#51452=CARTESIAN_POINT('Ctrl Pts',(-14.5177678139141,-1.38611763102972,
-3.55083364077171));
#51453=CARTESIAN_POINT('Ctrl Pts',(-14.3188942822166,2.23791305875133,-3.08569064764402));
#51454=CARTESIAN_POINT('Ctrl Pts',(-14.1200207505192,3.80574463510616,0.214591248302973));
#51455=CARTESIAN_POINT('Ctrl Pts',(-13.9211472188217,1.87685022649435,3.31770626469487));
#51456=CARTESIAN_POINT('Ctrl Pts',(-13.7222736871243,-1.77649802390547,
3.37250595292984));
#51457=CARTESIAN_POINT('Ctrl Pts',(-13.5234001554268,-3.79759624230632,
0.328640246939039));
#51458=CARTESIAN_POINT('Ctrl Pts',(-13.3245266237294,-2.32945523577606,
-3.01718079272738));
#51459=CARTESIAN_POINT('Ctrl Pts',(-13.125653092032,1.27899402439183,-3.59080992494138));
#51460=CARTESIAN_POINT('Ctrl Pts',(-12.9267795603345,3.71230094882514,-0.865195525207697));
#51461=CARTESIAN_POINT('Ctrl Pts',(-12.727906028637,2.7347381391122,2.65536229956906));
#51462=CARTESIAN_POINT('Ctrl Pts',(-12.5290324969396,-0.755507687979863,
3.73616779131918));
#51463=CARTESIAN_POINT('Ctrl Pts',(-12.3301589652421,-3.5515915000928,1.38417464503438));
#51464=CARTESIAN_POINT('Ctrl Pts',(-12.1312854335447,-3.08446574953506,
-2.23960100719584));
#51465=CARTESIAN_POINT('Ctrl Pts',(-11.9324119018472,0.216673464944433,
-3.80562665550321));
#51466=CARTESIAN_POINT('Ctrl Pts',(-11.7335383701498,3.31873265494329,-1.87503471874537));
#51467=CARTESIAN_POINT('Ctrl Pts',(-11.5346648384523,3.37153346731751,1.77834296755299));
#51468=CARTESIAN_POINT('Ctrl Pts',(-11.3357913067549,0.326562407243348,
3.79777548384086));
#51469=CARTESIAN_POINT('Ctrl Pts',(-11.1369177750574,-3.01845486312766,
2.32780408770765));
#51470=CARTESIAN_POINT('Ctrl Pts',(-10.93804424336,-3.59010960754647,-1.28095848382767));
#51471=CARTESIAN_POINT('Ctrl Pts',(-10.7391707116625,-0.863164273077971,
-3.7127737702652));
#51472=CARTESIAN_POINT('Ctrl Pts',(-10.540297179965,2.65685816780609,-2.73328489324651));
#51473=CARTESIAN_POINT('Ctrl Pts',(-10.3414236482676,3.73575386885591,0.757551755865984));
#51474=CARTESIAN_POINT('Ctrl Pts',(-10.1425501165701,1.38223124467995,3.55234829622857));
#51475=CARTESIAN_POINT('Ctrl Pts',(-9.94367658487268,-2.24128828520545,
3.08323992807701));
#51476=CARTESIAN_POINT('Ctrl Pts',(-9.74480305317522,-3.80550753666828,
-0.218755616723621));
#51477=CARTESIAN_POINT('Ctrl Pts',(-9.54592952147778,-1.87321864969616,
-3.31975805171371));
#51478=CARTESIAN_POINT('Ctrl Pts',(-9.34705598978035,1.78018737884529,-3.37055997242112));
#51479=CARTESIAN_POINT('Ctrl Pts',(-9.14818245808286,3.79795358849371,-0.324484469789755));
#51480=CARTESIAN_POINT('Ctrl Pts',(-8.94930892638544,2.32615224280039,3.01972802993948));
#51481=CARTESIAN_POINT('Ctrl Pts',(-8.75043539468796,-1.28292255980254,
3.58940821543569));
#51482=CARTESIAN_POINT('Ctrl Pts',(-8.55156186299052,-3.71324548026926,
0.861132762556118));
#51483=CARTESIAN_POINT('Ctrl Pts',(-8.35268833129305,-2.73183082915942,
-2.65835324070026));
#51484=CARTESIAN_POINT('Ctrl Pts',(-8.1538147995956,0.759595596975361,-3.73533882807744));
#51485=CARTESIAN_POINT('Ctrl Pts',(-7.95494126789815,3.55310402895249,-1.38028743054838));
#51486=CARTESIAN_POINT('Ctrl Pts',(-7.7560677362007,3.08201318363674,2.24297489227504));
#51487=CARTESIAN_POINT('Ctrl Pts',(-7.55719420450326,-0.220837703017022,
3.80538727863702));
#51488=CARTESIAN_POINT('Ctrl Pts',(-7.35832067280577,-3.32078245469979,
1.87140201989046));
#51489=CARTESIAN_POINT('Ctrl Pts',(-7.15944714110835,-3.36958546853095,
-1.78203125723078));
#51490=CARTESIAN_POINT('Ctrl Pts',(-6.96057360941086,-0.322406435201958,
-3.79813055621078));
#51491=CARTESIAN_POINT('Ctrl Pts',(-6.76170007771344,3.02100029278552,-2.32449970155028));
#51492=CARTESIAN_POINT('Ctrl Pts',(-6.56282654601595,3.58870574881201,1.28488625173232));
#51493=CARTESIAN_POINT('Ctrl Pts',(-6.36395301431852,0.85910099426281,3.71371607868986));
#51494=CARTESIAN_POINT('Ctrl Pts',(-6.16507948262105,-2.65984751782854,
2.73037594729784));
#51495=CARTESIAN_POINT('Ctrl Pts',(-5.96620595092362,-3.73492266906212,
-0.761639210718873));
#51496=CARTESIAN_POINT('Ctrl Pts',(-5.76733241922618,-1.3783432033079,-3.55385869799583));
#51497=CARTESIAN_POINT('Ctrl Pts',(-5.5684588875287,2.24466082806341,-3.08078551666176));
#51498=CARTESIAN_POINT('Ctrl Pts',(-5.36958535583126,3.80526588113653,0.222919723353213));
#51499=CARTESIAN_POINT('Ctrl Pts',(-5.17071182413379,1.86958483045521,3.32180586330821));
#51500=CARTESIAN_POINT('Ctrl Pts',(-4.97183829243635,-1.78387460325836,
3.36860995647996));
#51501=CARTESIAN_POINT('Ctrl Pts',(-4.77296476073887,-3.79830638486021,
0.320328303080476));
#51502=CARTESIAN_POINT('Ctrl Pts',(-4.57409122904144,-2.32284646837729,
-3.02227164935517));
#51503=CARTESIAN_POINT('Ctrl Pts',(-4.37521769734396,1.28684956643968,-3.58800221152922));
#51504=CARTESIAN_POINT('Ctrl Pts',(-4.17634416564651,3.71418555139234,-0.857068961927461));
#51505=CARTESIAN_POINT('Ctrl Pts',(-3.97747063394909,2.72892027452058,2.66134098575405));
#51506=CARTESIAN_POINT('Ctrl Pts',(-3.77859710225162,-0.76368264637654,
3.73450541646114));
#51507=CARTESIAN_POINT('Ctrl Pts',(-3.57972357055418,-3.55461220892666,
1.37639851722947));
#51508=CARTESIAN_POINT('Ctrl Pts',(-3.3808500388567,-3.07955710539971,-2.24634600462084));
#51509=CARTESIAN_POINT('Ctrl Pts',(-3.18197650715927,0.225002012982617,
-3.80514350931703));
#51510=CARTESIAN_POINT('Ctrl Pts',(-2.98310297546179,3.32282764303465,-1.86776677016589));
#51511=CARTESIAN_POINT('Ctrl Pts',(-2.78422944376435,3.36763463405492,1.78571682769388));
#51512=CARTESIAN_POINT('Ctrl Pts',(-2.58535591206688,0.318247812933675,
3.79848218594141));
#51513=CARTESIAN_POINT('Ctrl Pts',(-2.38648238036943,-3.02353782982558,
2.32119044494005));
#51514=CARTESIAN_POINT('Ctrl Pts',(-2.18760884867199,-3.58730566537358,
-1.28880854030746));
#51515=CARTESIAN_POINT('Ctrl Pts',(-1.98873531697452,-0.855021444261629,
-3.71466138124353));
#51516=CARTESIAN_POINT('Ctrl Pts',(-1.78986178527709,2.66280490197648,-2.72744968181255));
#51517=CARTESIAN_POINT('Ctrl Pts',(-1.59098825357962,3.73414134137891,0.765699223969745));
#51518=CARTESIAN_POINT('Ctrl Pts',(-1.39211472188218,1.37435089712346,3.55541493832914));
#51519=CARTESIAN_POINT('Ctrl Pts',(-1.19324119018471,-2.24783691714511,
3.07823282251273));
#51520=CARTESIAN_POINT('Ctrl Pts',(-0.994367658487268,-3.80538561390127,
-0.226904901415462));
#51521=CARTESIAN_POINT('Ctrl Pts',(-0.795494126789802,-1.86525717936383,
-3.32418745080932));
#51522=CARTESIAN_POINT('Ctrl Pts',(-0.596620595092344,1.78624879507146,
-3.36601485692819));
#51523=CARTESIAN_POINT('Ctrl Pts',(-0.397747063394925,3.80117096935424,
-0.317409156202402));
#51524=CARTESIAN_POINT('Ctrl Pts',(-0.198873531697423,2.31445171887122,
3.02736545452069));
#51525=CARTESIAN_POINT('Ctrl Pts',(-0.0662911772324812,-0.0808825703380203,
3.39599395944883));
#51526=CARTESIAN_POINT('Ctrl Pts',(0.,-1.09131022003071,3.03235215074973));
#51527=CARTESIAN_POINT('Ctrl Pts',(-109.840375352461,-1.53816642191745,
3.09873914818361));
#51528=CARTESIAN_POINT('Ctrl Pts',(-109.774084175229,-2.57071526811129,
2.586197792408));
#51529=CARTESIAN_POINT('Ctrl Pts',(-109.641501820764,-4.0651012769763,0.456647939553593));
#51530=CARTESIAN_POINT('Ctrl Pts',(-109.442628289066,-2.57873220422192,
-3.18056678679282));
#51531=CARTESIAN_POINT('Ctrl Pts',(-109.243754757369,1.28024521157691,-3.88503862978065));
#51532=CARTESIAN_POINT('Ctrl Pts',(-109.044881225672,3.96125087796401,-1.02519763748056));
#51533=CARTESIAN_POINT('Ctrl Pts',(-108.846007693974,3.00353488488411,2.77935581684627));
#51534=CARTESIAN_POINT('Ctrl Pts',(-108.647134162277,-0.71430246575407,
4.02877424317354));
#51535=CARTESIAN_POINT('Ctrl Pts',(-108.448260630579,-3.77558982751309,
1.57731788801589));
#51536=CARTESIAN_POINT('Ctrl Pts',(-108.249387098882,-3.36798852559464,
-2.32378978877478));
#51537=CARTESIAN_POINT('Ctrl Pts',(-108.050513567184,0.134196937583717,
-4.08957834911196));
#51538=CARTESIAN_POINT('Ctrl Pts',(-107.851640035487,3.51304523067848,-2.09796847093758));
#51539=CARTESIAN_POINT('Ctrl Pts',(-107.652766503789,3.66411981460646,1.82131980977203));
#51540=CARTESIAN_POINT('Ctrl Pts',(-107.453892972092,0.448583282276703,
4.0671435818543));
#51541=CARTESIAN_POINT('Ctrl Pts',(-107.255019440394,-3.17910703215976,
2.57608449495303));
#51542=CARTESIAN_POINT('Ctrl Pts',(-107.056145908697,-3.88583016883055,
-1.28189532651468));
#51543=CARTESIAN_POINT('Ctrl Pts',(-106.857272377,-1.0222430366496,-3.96206231753294));
#51544=CARTESIAN_POINT('Ctrl Pts',(-106.658398845302,2.7805822856922,-3.00188084347272));
#51545=CARTESIAN_POINT('Ctrl Pts',(-106.459525313605,4.02860332407945,0.716436251805123));
#51546=CARTESIAN_POINT('Ctrl Pts',(-106.260651781907,1.57513512905252,3.77648953898132));
#51547=CARTESIAN_POINT('Ctrl Pts',(-106.06177825021,-2.32557033628216,3.36669685901759));
#51548=CARTESIAN_POINT('Ctrl Pts',(-105.862904718512,-4.08953706540046,
-0.13642400659151));
#51549=CARTESIAN_POINT('Ctrl Pts',(-105.664031186815,-2.09602870811142,
-3.51419810952553));
#51550=CARTESIAN_POINT('Ctrl Pts',(-105.465157655117,1.82331511201696,-3.66311982958988));
#51551=CARTESIAN_POINT('Ctrl Pts',(-105.26628412342,4.06739327293676,-0.446359499308134));
#51552=CARTESIAN_POINT('Ctrl Pts',(-105.067410591722,2.57434213819699,3.18051683979354));
#51553=CARTESIAN_POINT('Ctrl Pts',(-104.868537060025,-1.28401983628658,
3.88512778430906));
#51554=CARTESIAN_POINT('Ctrl Pts',(-104.669663528328,-3.96262175015484,
1.02007533898783));
#51555=CARTESIAN_POINT('Ctrl Pts',(-104.47078999663,-3.00035866289289,-2.7822244199646));
#51556=CARTESIAN_POINT('Ctrl Pts',(-104.271916464933,0.718640123994403,
-4.02821067041903));
#51557=CARTESIAN_POINT('Ctrl Pts',(-104.073042933235,3.77735088960066,-1.57306868522629));
#51558=CARTESIAN_POINT('Ctrl Pts',(-103.874169401538,3.36542390180016,2.327412037546));
#51559=CARTESIAN_POINT('Ctrl Pts',(-103.67529586984,-0.138661477048271,
4.08946180159252));
#51560=CARTESIAN_POINT('Ctrl Pts',(-103.476422338143,-3.51534440610599,
2.09410566545931));
#51561=CARTESIAN_POINT('Ctrl Pts',(-103.277548806445,-3.66212167685685,
-1.82531905581637));
#51562=CARTESIAN_POINT('Ctrl Pts',(-103.078675274748,-0.444134031586379,
-4.06763688075757));
#51563=CARTESIAN_POINT('Ctrl Pts',(-102.87980174305,3.18192487383849,-2.57260158767713));
#51564=CARTESIAN_POINT('Ctrl Pts',(-102.680928211353,3.88442467181907,1.28614532640571));
#51565=CARTESIAN_POINT('Ctrl Pts',(-102.482054679656,1.01790710555096,3.9631792737841));
#51566=CARTESIAN_POINT('Ctrl Pts',(-102.283181147958,-2.78386559933878,
2.99883596692024));
#51567=CARTESIAN_POINT('Ctrl Pts',(-102.084307616261,-4.02781687552084,
-0.720843983776407));
#51568=CARTESIAN_POINT('Ctrl Pts',(-101.885434084563,-1.57100173626865,
-3.77821100209074));
#51569=CARTESIAN_POINT('Ctrl Pts',(-101.686560552866,2.32925302396205,-3.36414999398676));
#51570=CARTESIAN_POINT('Ctrl Pts',(-101.487687021168,4.08938532318502,0.140898936108952));
#51571=CARTESIAN_POINT('Ctrl Pts',(-101.288813489471,2.09218199084294,3.51648963440394));
#51572=CARTESIAN_POINT('Ctrl Pts',(-101.089939957773,-1.82732245050554,
3.66112243629685));
#51573=CARTESIAN_POINT('Ctrl Pts',(-100.891066426076,-4.06787927233846,
0.441908426437971));
#51574=CARTESIAN_POINT('Ctrl Pts',(-100.692192894378,-2.5708602662819,-3.18333195299057));
#51575=CARTESIAN_POINT('Ctrl Pts',(-100.493319362681,1.28827043111132,-3.8837203977632));
#51576=CARTESIAN_POINT('Ctrl Pts',(-100.294445830984,3.96373561122914,-1.01573856673447));
#51577=CARTESIAN_POINT('Ctrl Pts',(-100.095572299286,2.99731237312002,2.78550594499804));
#51578=CARTESIAN_POINT('Ctrl Pts',(-99.8966987675887,-0.723047627711036,
4.0274218750634));
#51579=CARTESIAN_POINT('Ctrl Pts',(-99.6978252358912,-3.77906998358733,
1.56893431692567));
#51580=CARTESIAN_POINT('Ctrl Pts',(-99.4989517041938,-3.36287507908286,
-2.33109331305317));
#51581=CARTESIAN_POINT('Ctrl Pts',(-99.3000781724963,0.143136352982075,
-4.08930762062879));
#51582=CARTESIAN_POINT('Ctrl Pts',(-99.1012046407988,3.51763381002914,-2.09025768990755));
#51583=CARTESIAN_POINT('Ctrl Pts',(-98.9023311091013,3.66012209976044,1.82932529816953));
#51584=CARTESIAN_POINT('Ctrl Pts',(-98.703457577404,0.439682689003533,4.068120446185));
#51585=CARTESIAN_POINT('Ctrl Pts',(-98.5045840457065,-3.18473807919821,
2.56911817528557));
#51586=CARTESIAN_POINT('Ctrl Pts',(-98.3057105140089,-3.88301496109731,
-1.2903951501661));
#51587=CARTESIAN_POINT('Ctrl Pts',(-98.1068369823117,-1.01356972385213,
-3.96429076211219));
#51588=CARTESIAN_POINT('Ctrl Pts',(-97.907963450614,2.7871454568033,-2.99578788206015));
#51589=CARTESIAN_POINT('Ctrl Pts',(-97.7090899189167,4.02702566897857,0.725251055197827));
#51590=CARTESIAN_POINT('Ctrl Pts',(-97.5102163872191,1.56686642791497,3.77992783380196));
#51591=CARTESIAN_POINT('Ctrl Pts',(-97.3113428555218,-2.33293290432075,
3.3615991574867));
#51592=CARTESIAN_POINT('Ctrl Pts',(-97.1124693238244,-4.08922869391941,
-0.145373727006639));
#51593=CARTESIAN_POINT('Ctrl Pts',(-96.9135957921267,-2.08833276324387,
-3.5187769326344));
#51594=CARTESIAN_POINT('Ctrl Pts',(-96.7147222604295,1.83132759821652,-3.65912066754955));
#51595=CARTESIAN_POINT('Ctrl Pts',(-96.5158487287319,4.06836040222087,-0.437456819948072));
#51596=CARTESIAN_POINT('Ctrl Pts',(-96.3169751970346,2.56737531521184,3.1861432520398));
#51597=CARTESIAN_POINT('Ctrl Pts',(-96.1181016653369,-1.29251948293511,
3.88230836203293));
#51598=CARTESIAN_POINT('Ctrl Pts',(-95.9192281336396,-3.96484472626648,
1.01140057755301));
#51599=CARTESIAN_POINT('Ctrl Pts',(-95.7203546019421,-2.99426249419735,
-2.78878413426369));
#51600=CARTESIAN_POINT('Ctrl Pts',(-95.5214810702447,0.727454265577372,
-4.02662825738497));
#51601=CARTESIAN_POINT('Ctrl Pts',(-95.3226075385471,3.78078455247771,-1.56479806985557));
#51602=CARTESIAN_POINT('Ctrl Pts',(-95.1237340068498,3.3603222295803,2.33477179721405));
#51603=CARTESIAN_POINT('Ctrl Pts',(-94.9248604751522,-0.147611057512885,
4.08914854308052));
#51604=CARTESIAN_POINT('Ctrl Pts',(-94.725986943455,-3.51991900187753,2.08640721142814));
#51605=CARTESIAN_POINT('Ctrl Pts',(-94.5271134117573,-3.65811813996398,
-1.83332935004715));
#51606=CARTESIAN_POINT('Ctrl Pts',(-94.32823988006,-0.435230819937879,-4.06859914037424));
#51607=CARTESIAN_POINT('Ctrl Pts',(-94.1293663483624,3.18754747109466,-2.56563168658245));
#51608=CARTESIAN_POINT('Ctrl Pts',(-93.9304928166651,3.8816006007816,1.29464342878244));
#51609=CARTESIAN_POINT('Ctrl Pts',(-93.7316192849675,1.00923112848644,3.96539750352618));
#51610=CARTESIAN_POINT('Ctrl Pts',(-93.5327457532702,-2.79042197688866,
2.99273620998821));
#51611=CARTESIAN_POINT('Ctrl Pts',(-93.3338722215725,-4.02622964040159,
-0.729657258190121));
#51612=CARTESIAN_POINT('Ctrl Pts',(-93.1349986898753,-1.56272924336663,
-3.78164013935813));
#51613=CARTESIAN_POINT('Ctrl Pts',(-92.9361251581777,2.33660999118264,-3.35904429574591));
#51614=CARTESIAN_POINT('Ctrl Pts',(-92.7372516264803,4.08906716813612,0.149848343831102));
#51615=CARTESIAN_POINT('Ctrl Pts',(-92.5383780947828,2.08448103503674,3.52106001741663));
#51616=CARTESIAN_POINT('Ctrl Pts',(-92.3395045630855,-1.83533055306216,
3.65711451730382));
#51617=CARTESIAN_POINT('Ctrl Pts',(-92.1406310313879,-4.06883666057366,
0.433004689639325));
#51618=CARTESIAN_POINT('Ctrl Pts',(-91.9417574996906,-2.56388728991935,
-3.18895073594244));
#51619=CARTESIAN_POINT('Ctrl Pts',(-91.7428839679929,1.29676698707227,-3.88089167755519));
#51620=CARTESIAN_POINT('Ctrl Pts',(-91.5440104362956,3.9659490937258,-1.00706137730188));
#51621=CARTESIAN_POINT('Ctrl Pts',(-91.3451369045981,2.99120902988965,2.79205898418792));
#51622=CARTESIAN_POINT('Ctrl Pts',(-91.1462633729006,-0.731860032376595,
4.02582981814775));
#51623=CARTESIAN_POINT('Ctrl Pts',(-90.9473898412033,-3.78249459418708,
1.56065994906748));
#51624=CARTESIAN_POINT('Ctrl Pts',(-90.7485163095056,-3.35776535636607,
-2.33844748567623));
#51625=CARTESIAN_POINT('Ctrl Pts',(-90.5496427778085,0.152085585291523,
-4.08898456911055));
#51626=CARTESIAN_POINT('Ctrl Pts',(-90.3507692461107,3.52219997891014,-2.08255423464631));
#51627=CARTESIAN_POINT('Ctrl Pts',(-90.1518957144135,3.65610979986952,1.83733120666248));
#51628=CARTESIAN_POINT('Ctrl Pts',(-89.9530221827158,0.430778429718823,
4.069072962748));
#51629=CARTESIAN_POINT('Ctrl Pts',(-89.7541486510186,-3.19035304616309,
2.56214212574474));
#51630=CARTESIAN_POINT('Ctrl Pts',(-89.5552751193211,-3.88018159256591,
-1.29889015716891));
#51631=CARTESIAN_POINT('Ctrl Pts',(-89.3564015876235,-1.00489132464883,
-3.96649949670023));
#51632=CARTESIAN_POINT('Ctrl Pts',(-89.1575280559263,2.79369515567141,-2.98968095435883));
#51633=CARTESIAN_POINT('Ctrl Pts',(-88.9586545242286,4.02542879074315,0.734062587477381));
#51634=CARTESIAN_POINT('Ctrl Pts',(-88.7597809925313,1.55859018757754,3.7833479167088));
#51635=CARTESIAN_POINT('Ctrl Pts',(-88.5609074608337,-2.34028428014475,
3.35648541182365));
#51636=CARTESIAN_POINT('Ctrl Pts',(-88.3620339291363,-4.08890074602855,
-0.154322781224421));
#51637=CARTESIAN_POINT('Ctrl Pts',(-88.1631603974389,-2.08062681083363,
-3.5233388860168));
#51638=CARTESIAN_POINT('Ctrl Pts',(-87.9642868657414,1.83933131024921,-3.65510398796186));
#51639=CARTESIAN_POINT('Ctrl Pts',(-87.7654133340439,4.06930804682655,-0.4285520408428));
#51640=CARTESIAN_POINT('Ctrl Pts',(-87.5665398023466,2.56039619458104,3.19175440133679));
#51641=CARTESIAN_POINT('Ctrl Pts',(-87.367666270649,-1.30101293843677,3.87947034602635));
#51642=CARTESIAN_POINT('Ctrl Pts',(-87.1687927389516,-3.9670487122847,1.00272097117692));
#51643=CARTESIAN_POINT('Ctrl Pts',(-86.9699192072541,-2.9881519838532,-2.79533049084934));
#51644=CARTESIAN_POINT('Ctrl Pts',(-86.7710456755567,0.736264922833142,
-4.02502655830782));
#51645=CARTESIAN_POINT('Ctrl Pts',(-86.5721721438591,3.78420010666783,-1.55651995951644));
#51646=CARTESIAN_POINT('Ctrl Pts',(-86.3732986121619,3.35520446250181,2.34212037403835));
#51647=CARTESIAN_POINT('Ctrl Pts',(-86.1744250804642,-0.156559930960084,
4.08881569891521));
#51648=CARTESIAN_POINT('Ctrl Pts',(-85.975551548767,-3.52447673839568,2.07869876417571));
#51649=CARTESIAN_POINT('Ctrl Pts',(-85.7766780170693,-3.65409708188192,
-1.84133086322361));
#51650=CARTESIAN_POINT('Ctrl Pts',(-85.577804485372,-0.426325523677742,
-4.06954191273892));
#51651=CARTESIAN_POINT('Ctrl Pts',(-85.3789309536745,3.19315480104402,-2.55864949695091));
#51652=CARTESIAN_POINT('Ctrl Pts',(-85.180057421977,3.8787579381494,1.30313533024036));
#51653=CARTESIAN_POINT('Ctrl Pts',(-84.9811838902796,1.00055031753589,3.9675967403148));
#51654=CARTESIAN_POINT('Ctrl Pts',(-84.7823103585822,-2.79696498923216,
2.98662211883046));
#51655=CARTESIAN_POINT('Ctrl Pts',(-84.5834368268846,-4.02462312096219,
-0.738467037784595));
#51656=CARTESIAN_POINT('Ctrl Pts',(-84.3845632951873,-1.55444926550391,
-3.78505116380902));
#51657=CARTESIAN_POINT('Ctrl Pts',(-84.1856897634898,2.34395576680736,-3.35392250878403));
#51658=CARTESIAN_POINT('Ctrl Pts',(-83.9868162317923,4.088729427796,0.158797033828775));
#51659=CARTESIAN_POINT('Ctrl Pts',(-83.7879427000949,2.07677009524969,3.52561353570614));
#51660=CARTESIAN_POINT('Ctrl Pts',(-83.5890691683974,-1.84332986498711,
3.65308908193113));
#51661=CARTESIAN_POINT('Ctrl Pts',(-83.3901956367,-4.06977456041508,0.424098878890195));
#51662=CARTESIAN_POINT('Ctrl Pts',(-83.1913221050024,-2.55690203337726,
-3.19455424486561));
#51663=CARTESIAN_POINT('Ctrl Pts',(-82.9924485733052,1.30525733194437,-3.87804436914836));
#51664=CARTESIAN_POINT('Ctrl Pts',(-82.7935750416075,3.96814358062647,-0.99837936437545));
#51665=CARTESIAN_POINT('Ctrl Pts',(-82.5947015099103,2.98509135974858,2.79859865033059));
#51666=CARTESIAN_POINT('Ctrl Pts',(-82.3958279782126,-0.740668931672492,
4.02421847882701));
#51667=CARTESIAN_POINT('Ctrl Pts',(-82.1969544465152,-3.78590108787766,
1.55237810615983));
#51668=CARTESIAN_POINT('Ctrl Pts',(-81.9980809148179,-3.35263955105406,
-2.34579045790239));
#51669=CARTESIAN_POINT('Ctrl Pts',(-81.7992073831203,0.161034089160873,
-4.08864193269671));
#51670=CARTESIAN_POINT('Ctrl Pts',(-81.6003338514228,3.52674927760791,-2.07484080463296));
#51671=CARTESIAN_POINT('Ctrl Pts',(-81.4014603197255,3.65207998841123,1.84532831494129));
#51672=CARTESIAN_POINT('Ctrl Pts',(-81.2025867880279,0.421872107146664,
4.07000598978543));
#51673=CARTESIAN_POINT('Ctrl Pts',(-81.0037132563306,-3.19595273238265,
2.55515380438312));
#51674=CARTESIAN_POINT('Ctrl Pts',(-80.804839724633,-3.87732963923677,-1.3073789429136));
#51675=CARTESIAN_POINT('Ctrl Pts',(-80.6059661929356,-0.996208112345541,
-3.96868923305602));
#51676=CARTESIAN_POINT('Ctrl Pts',(-80.4070926612381,2.80023147365557,-2.98355970706581));
#51677=CARTESIAN_POINT('Ctrl Pts',(-80.2082191295408,4.02381263202344,0.742870603837753));
#51678=CARTESIAN_POINT('Ctrl Pts',(-80.0093455978432,1.55030648210414,3.78674987861933));
#51679=CARTESIAN_POINT('Ctrl Pts',(-79.8104720661458,-2.34762444677422,
3.35135558969589));
#51680=CARTESIAN_POINT('Ctrl Pts',(-79.6115985344483,-4.08855321364357,
-0.163271096286671));
#51681=CARTESIAN_POINT('Ctrl Pts',(-79.412725002751,-2.07291089290303,-3.52788396376096));
#51682=CARTESIAN_POINT('Ctrl Pts',(-79.2138514710534,1.8473262124879,-3.6510698016243));
#51683=CARTESIAN_POINT('Ctrl Pts',(-79.014977939356,4.07023620078068,-0.419645209113765));
#51684=CARTESIAN_POINT('Ctrl Pts',(-78.8161044076585,2.55340481049188,3.19735026317646));
#51685=CARTESIAN_POINT('Ctrl Pts',(-78.6172308759612,-1.3095001625129,3.87661374862863));
#51686=CARTESIAN_POINT('Ctrl Pts',(-78.4183573442636,-3.96923369744009,
0.994036562096127));
#51687=CARTESIAN_POINT('Ctrl Pts',(-78.2194838125662,-2.98202716124064,
-2.80186345871831));
#51688=CARTESIAN_POINT('Ctrl Pts',(-78.0206102808687,0.745072053621266,
-4.02340558067295));
#51689=CARTESIAN_POINT('Ctrl Pts',(-77.8217367491712,3.78759753577992,-1.54823439395703));
#51690=CARTESIAN_POINT('Ctrl Pts',(-77.6228632174739,3.35007062509393,2.34945773287382));
#51691=CARTESIAN_POINT('Ctrl Pts',(-77.4239896857763,-0.165508054536509,
4.08846327066312));
#51692=CARTESIAN_POINT('Ctrl Pts',(-77.2251161540789,-3.52901759382565,
2.07098036063764));
#51693=CARTESIAN_POINT('Ctrl Pts',(-77.0262426223815,-3.65005852187275,
-1.84932355702888));
#51694=CARTESIAN_POINT('Ctrl Pts',(-76.827369090684,-0.417418185458136,
-4.0704651933319));
#51695=CARTESIAN_POINT('Ctrl Pts',(-76.6284955589865,3.19874683682869,-2.5516550522271));
#51696=CARTESIAN_POINT('Ctrl Pts',(-76.4296220272891,3.87589669753825,1.31162099010726));
#51697=CARTESIAN_POINT('Ctrl Pts',(-76.2307484955916,0.991864714277272,
3.96977697361571));
#51698=CARTESIAN_POINT('Ctrl Pts',(-76.0318749638942,-2.80349460503027,
2.98049372273185));
#51699=CARTESIAN_POINT('Ctrl Pts',(-75.8330014321968,-4.0229973248974,-0.747273280364011));
#51700=CARTESIAN_POINT('Ctrl Pts',(-75.6341279004993,-1.54616184233881,
-3.78844405910568));
#51701=CARTESIAN_POINT('Ctrl Pts',(-75.4352543688018,2.35129031565238,-3.34878465763285));
#51702=CARTESIAN_POINT('Ctrl Pts',(-75.2363808371043,4.08837210378228,0.167744963240746));
#51703=CARTESIAN_POINT('Ctrl Pts',(-75.0375073054069,2.06904920841471,3.53015016746261));
#51704=CARTESIAN_POINT('Ctrl Pts',(-74.8386337737095,-1.8513203479663,3.64904614945931));
#51705=CARTESIAN_POINT('Ctrl Pts',(-74.639760242012,-4.07069296737055,0.415191036846439));
#51706=CARTESIAN_POINT('Ctrl Pts',(-74.4408867103145,-2.54990453011259,
-3.20014245292127));
#51707=CARTESIAN_POINT('Ctrl Pts',(-74.2420131786171,1.31374142506182,-3.87517848618026));
#51708=CARTESIAN_POINT('Ctrl Pts',(-74.0431396469197,3.97031906142024,-0.989692569539129));
#51709=CARTESIAN_POINT('Ctrl Pts',(-73.8442661152222,2.97895939199849,2.80512491210317));
#51710=CARTESIAN_POINT('Ctrl Pts',(-73.6453925835248,-0.749474283407049,
4.02258786481901));
#51711=CARTESIAN_POINT('Ctrl Pts',(-73.4465190518271,-3.78928944834319,
1.54408882786989));
#51712=CARTESIAN_POINT('Ctrl Pts',(-73.24764552013,-3.34749768769759,-2.35312219456132));
#51713=CARTESIAN_POINT('Ctrl Pts',(-73.0487719884322,0.169981821729752,
-4.08827971302836));
#51714=CARTESIAN_POINT('Ctrl Pts',(-72.8498984567351,3.53128168433279,-2.06711743681233));
#51715=CARTESIAN_POINT('Ctrl Pts',(-72.6510249250373,3.64803268468702,1.85331658470237));
#51716=CARTESIAN_POINT('Ctrl Pts',(-72.4521513933401,0.412963763945437,
4.07091952282843));
#51717=CARTESIAN_POINT('Ctrl Pts',(-72.2532778616425,-3.2015371110364,2.54815324467241));
#51718=CARTESIAN_POINT('Ctrl Pts',(-72.0544043299451,-3.87445911476969,
-1.31586146674182));
#51719=CARTESIAN_POINT('Ctrl Pts',(-71.8555307982476,-0.987520128531938,
-3.97085996069139));
#51720=CARTESIAN_POINT('Ctrl Pts',(-71.6566572665502,2.80675437944895,-2.97742416949987));
#51721=CARTESIAN_POINT('Ctrl Pts',(-71.4577837348527,4.02217720056034,0.751675062091496));
#51722=CARTESIAN_POINT('Ctrl Pts',(-71.2589102031553,1.54201535117083,3.79013370323939));
#51723=CARTESIAN_POINT('Ctrl Pts',(-71.0600366714579,-2.35495336905225,
3.34620971567343));
#51724=CARTESIAN_POINT('Ctrl Pts',(-70.8611631397604,-4.08818609842901,
-0.172218629333917));
#51725=CARTESIAN_POINT('Ctrl Pts',(-70.6622896080629,-2.06518504640879,
-3.53241214409748));
#51726=CARTESIAN_POINT('Ctrl Pts',(-70.4634160763654,1.85531226663959,-3.64701812785929));
#51727=CARTESIAN_POINT('Ctrl Pts',(-70.264542544668,4.07114485963774,-0.410736367421776));
#51728=CARTESIAN_POINT('Ctrl Pts',(-70.0656690129706,2.54640119643073,3.20293081075661));
#51729=CARTESIAN_POINT('Ctrl Pts',(-69.8667954812731,-1.3179811145126,3.87373858352186));
#51730=CARTESIAN_POINT('Ctrl Pts',(-69.6679219495757,-3.97139967126727,
0.985347391906037));
#51731=CARTESIAN_POINT('Ctrl Pts',(-69.4690484178782,-2.97588805569555,
-2.80838300657983));
#51732=CARTESIAN_POINT('Ctrl Pts',(-69.2701748861808,0.753875615758535,
-4.02176533224433));
#51733=CARTESIAN_POINT('Ctrl Pts',(-69.0713013544833,3.79097682354154,-1.53994141286236));
#51734=CARTESIAN_POINT('Ctrl Pts',(-68.8724278227859,3.34492074194592,2.356783838577));
#51735=CARTESIAN_POINT('Ctrl Pts',(-68.6735542910884,-0.174455385383641,
4.08809126001224));
#51736=CARTESIAN_POINT('Ctrl Pts',(-68.4746807593909,-3.53354154641825,
2.06325203778256));
#51737=CARTESIAN_POINT('Ctrl Pts',(-68.2758072276935,-3.64600247927983,
-1.85730739318052));
#51738=CARTESIAN_POINT('Ctrl Pts',(-68.076933695996,-0.408508847942281,
-4.07136897773102));
#51739=CARTESIAN_POINT('Ctrl Pts',(-67.8780601642986,3.20432355166466,-2.54464838591208));
#51740=CARTESIAN_POINT('Ctrl Pts',(-67.6791866326011,3.87301689265249,1.32010036773963));
#51741=CARTESIAN_POINT('Ctrl Pts',(-67.4803131009036,0.983174360311834,
3.9719381929863));
#51742=CARTESIAN_POINT('Ctrl Pts',(-67.2814395692062,-2.81001079300828,
2.97435105104539));
#51743=CARTESIAN_POINT('Ctrl Pts',(-67.0825660375088,-4.02135225999428,
-0.756075943749426));
#51744=CARTESIAN_POINT('Ctrl Pts',(-66.8836925058113,-1.53786701356531,
-3.79181880899725));
#51745=CARTESIAN_POINT('Ctrl Pts',(-66.6848189741139,2.35861360258762,-3.34363076690093));
#51746=CARTESIAN_POINT('Ctrl Pts',(-66.4859454424164,4.08799519780646,0.176692089209336));
#51747=CARTESIAN_POINT('Ctrl Pts',(-66.287071910719,2.0613184115123,3.53466989095704));
#51748=CARTESIAN_POINT('Ctrl Pts',(-66.0881983790215,-1.85930196372788,
3.64498573925267));
#51749=CARTESIAN_POINT('Ctrl Pts',(-65.8893248473241,-4.07159187704117,
0.406281206173773));
#51750=CARTESIAN_POINT('Ctrl Pts',(-65.6904513156265,-2.54289481364118,
-3.20571533334365));
#51751=CARTESIAN_POINT('Ctrl Pts',(-65.4915777839292,1.32221922578853,-3.87229404237759));
#51752=CARTESIAN_POINT('Ctrl Pts',(-65.2927042522315,3.97247552568726,-0.981001034399843));
#51753=CARTESIAN_POINT('Ctrl Pts',(-65.0938307205343,2.97281315600949,2.81163773824701));
#51754=CARTESIAN_POINT('Ctrl Pts',(-64.8949571888367,-0.758276045405488,
4.02093798393383));
#51755=CARTESIAN_POINT('Ctrl Pts',(-64.6960836571393,-3.79265965935448,
1.53579215390065));
#51756=CARTESIAN_POINT('Ctrl Pts',(-64.4972101254419,-3.3423397909246,-2.36044266053635));
#51757=CARTESIAN_POINT('Ctrl Pts',(-64.2983365937444,0.178928740141437,
-4.08789791184041));
#51758=CARTESIAN_POINT('Ctrl Pts',(-64.099463062047,3.53579717737605,-2.05938416817684));
#51759=CARTESIAN_POINT('Ctrl Pts',(-63.9005895303494,3.64396790808217,1.86129597768461));
#51760=CARTESIAN_POINT('Ctrl Pts',(-63.7017159986521,0.404053442783113,
4.07181355750147));
#51761=CARTESIAN_POINT('Ctrl Pts',(-63.5028424669546,-3.20710615537694,
2.54114048014296));
#51762=CARTESIAN_POINT('Ctrl Pts',(-63.3039689352571,-3.87157003291358,
-1.32433768802498));
#51763=CARTESIAN_POINT('Ctrl Pts',(-63.1050954035597,-0.978827414820659,
-3.97301166920931));
#51764=CARTESIAN_POINT('Ctrl Pts',(-62.9062218718622,2.81326384180894,-2.97127437104824));
#51765=CARTESIAN_POINT('Ctrl Pts',(-62.7073483401648,4.02052250418702,0.76047592006806));
#51766=CARTESIAN_POINT('Ctrl Pts',(-62.5084748084674,1.53371683448956,3.79349937436151));
#51767=CARTESIAN_POINT('Ctrl Pts',(-62.3096012767698,-2.36227101187565,
3.34104781440341));
#51768=CARTESIAN_POINT('Ctrl Pts',(-62.1107277450724,-4.08779940214323,
-0.181165337510387));
#51769=CARTESIAN_POINT('Ctrl Pts',(-61.911854213375,-2.0574493083552,-3.53692340533783));
#51770=CARTESIAN_POINT('Ctrl Pts',(-61.7129806816776,1.86328943445378,-3.64294898607303));
#51771=CARTESIAN_POINT('Ctrl Pts',(-61.51410714998,4.07203401904556,-0.401825558437184));
#51772=CARTESIAN_POINT('Ctrl Pts',(-61.3152336182825,2.53938538594258,3.20849601734817));
#51773=CARTESIAN_POINT('Ctrl Pts',(-61.1163600865852,-1.32645575381482,
3.87084486447718));
#51774=CARTESIAN_POINT('Ctrl Pts',(-60.9174865548877,-3.97354662339195,
0.976653502224961));
#51775=CARTESIAN_POINT('Ctrl Pts',(-60.7186130231902,-2.96973469662225,
-2.81488910320741));
#51776=CARTESIAN_POINT('Ctrl Pts',(-60.5197394914928,0.762675567078782,
-4.02010582087821));
#51777=CARTESIAN_POINT('Ctrl Pts',(-60.3208659597953,3.794337953767,-1.53164105595309));
#51778=CARTESIAN_POINT('Ctrl Pts',(-60.1219924280979,3.33975483772404,2.36409865605831));
#51779=CARTESIAN_POINT('Ctrl Pts',(-59.9231188964004,-0.183401880646781,
4.0876996687444));
#51780=CARTESIAN_POINT('Ctrl Pts',(-59.724245364703,-3.53804857450529,2.05551383262651));
#51781=CARTESIAN_POINT('Ctrl Pts',(-59.5253718330054,-3.64192897353023,
-1.86528233343871));
#51782=CARTESIAN_POINT('Ctrl Pts',(-59.3264983013081,-0.399597553802876,
-4.07225326160742));
#51783=CARTESIAN_POINT('Ctrl Pts',(-59.1276247696106,3.20988491884128,-2.53762953156546));
#51784=CARTESIAN_POINT('Ctrl Pts',(-58.9287512379131,3.87011853728548,1.32857342252401));
#51785=CARTESIAN_POINT('Ctrl Pts',(-58.7298777062157,0.974479297263519,
3.97408038807503));
#51786=CARTESIAN_POINT('Ctrl Pts',(-58.5310041745182,-2.81651352195577,
2.96819413319245));
#51787=CARTESIAN_POINT('Ctrl Pts',(-58.3321306428208,-4.01968793413213,
-0.764874985778962));
#51788=CARTESIAN_POINT('Ctrl Pts',(-58.1332571111233,-1.52956481891289,
-3.79517539731984));
#51789=CARTESIAN_POINT('Ctrl Pts',(-57.9343835794259,2.365925592537,-3.33846086127369));
#51790=CARTESIAN_POINT('Ctrl Pts',(-57.7355100477284,4.08759871167377,0.185638368880856));
#51791=CARTESIAN_POINT('Ctrl Pts',(-57.536636516031,2.05357774157035,3.5391726845415));
#51792=CARTESIAN_POINT('Ctrl Pts',(-57.3377629843335,-1.86727467404277,
3.6409078707592));
#51793=CARTESIAN_POINT('Ctrl Pts',(-57.138889452636,-4.07247128512151,0.397369429547074));
#51794=CARTESIAN_POINT('Ctrl Pts',(-56.9400159209386,-2.53587291753704,
-3.21127285944058));
#51795=CARTESIAN_POINT('Ctrl Pts',(-56.7411423892411,1.33069069351864,-3.86939105155583));
#51796=CARTESIAN_POINT('Ctrl Pts',(-56.5422688575438,3.97461296309879,-0.972304800587201));
#51797=CARTESIAN_POINT('Ctrl Pts',(-56.3433953258462,2.96665268122003,2.8181370975678));
#51798=CARTESIAN_POINT('Ctrl Pts',(-56.1445217941488,-0.767074175510283,
4.01926884407389));
#51799=CARTESIAN_POINT('Ctrl Pts',(-55.9456482624513,-3.79601170476937,
1.5274881239904));
#51800=CARTESIAN_POINT('Ctrl Pts',(-55.7467747307539,-3.33716588543964,
-2.36775182076493));
#51801=CARTESIAN_POINT('Ctrl Pts',(-55.5479011990564,0.187874801543228,
-4.08749653096158));
#51802=CARTESIAN_POINT('Ctrl Pts',(-55.349027667359,3.54029573511,-2.05164103576619));
#51803=CARTESIAN_POINT('Ctrl Pts',(-55.1501541356615,3.63988567806557,1.86926645566944));
#51804=CARTESIAN_POINT('Ctrl Pts',(-54.9512806039641,0.395141186337052,
4.07268808952245));
#51805=CARTESIAN_POINT('Ctrl Pts',(-54.7524070722666,-3.21265983873043,
2.53411554438349));
#51806=CARTESIAN_POINT('Ctrl Pts',(-54.5535335405691,-3.86866240750616,
-1.33280756616482));
#51807=CARTESIAN_POINT('Ctrl Pts',(-54.3546600088718,-0.97013001284694,
-3.97514434830377));
#51808=CARTESIAN_POINT('Ctrl Pts',(-54.1557864771742,2.81975982955745,-2.9651103411664));
#51809=CARTESIAN_POINT('Ctrl Pts',(-53.9569129454769,4.01884855082893,0.769273135614399));
#51810=CARTESIAN_POINT('Ctrl Pts',(-53.7580394137793,1.52541097180728,3.79684687586526));
#51811=CARTESIAN_POINT('Ctrl Pts',(-53.5591658820819,-2.36957734019541,
3.33586991060956));
#51812=CARTESIAN_POINT('Ctrl Pts',(-53.3602923503844,-4.0873931266384,-0.190111177964406));
#51813=CARTESIAN_POINT('Ctrl Pts',(-53.161418818687,-2.04970371579381,-3.5414177258746));
#51814=CARTESIAN_POINT('Ctrl Pts',(-52.9625452869895,1.87125767772255,-3.63886239575533));
#51815=CARTESIAN_POINT('Ctrl Pts',(-52.7636717552921,4.07290367474537,-0.392912824839691));
#51816=CARTESIAN_POINT('Ctrl Pts',(-52.5647982235946,2.53235741263075,3.2140458562957));
#51817=CARTESIAN_POINT('Ctrl Pts',(-52.3659246918972,-1.33492403982889,
3.8679326053545));
#51818=CARTESIAN_POINT('Ctrl Pts',(-52.1670511601997,-3.97567454353092,
0.967954934693781));
#51819=CARTESIAN_POINT('Ctrl Pts',(-51.9681776285023,-2.96356711349329,
-2.82138171743897));
#51820=CARTESIAN_POINT('Ctrl Pts',(-51.7693040968048,0.771471865433048,
-4.01842705452308));
#51821=CARTESIAN_POINT('Ctrl Pts',(-51.5704305651073,3.79768091035748,-1.52333336298533));
#51822=CARTESIAN_POINT('Ctrl Pts',(-51.37155703341,3.3345729371714,2.37140215028196));
#51823=CARTESIAN_POINT('Ctrl Pts',(-51.1726835017124,-0.192347497474924,
4.08728849873519));
#51824=CARTESIAN_POINT('Ctrl Pts',(-50.9738099700151,-3.54253865649944,
2.04776578223315));
#51825=CARTESIAN_POINT('Ctrl Pts',(-50.7749364383174,-3.63783802413481,
-1.87324833960604));
#51826=CARTESIAN_POINT('Ctrl Pts',(-50.5760629066202,-0.390684345722062,
-4.07311804072575));
#51827=CARTESIAN_POINT('Ctrl Pts',(-50.3771893749225,3.21543091172149,-2.53059852280511));
#51828=CARTESIAN_POINT('Ctrl Pts',(-50.1783158432253,3.86720164531933,1.33704011387727));
#51829=CARTESIAN_POINT('Ctrl Pts',(-49.9794423115276,0.965779566778829,
3.97620354862152));
#51830=CARTESIAN_POINT('Ctrl Pts',(-49.7805687798304,-2.82300276072682,
2.96202299866266));
#51831=CARTESIAN_POINT('Ctrl Pts',(-49.5816952481327,-4.01800435528252,
-0.773670364308027));
#51832=CARTESIAN_POINT('Ctrl Pts',(-49.3828217164354,-1.52125529814649,
-3.79851380799636));
#51833=CARTESIAN_POINT('Ctrl Pts',(-49.1839481847379,2.37322625047831,-3.33327496551342));
#51834=CARTESIAN_POINT('Ctrl Pts',(-48.9850746530405,4.08718264728328,0.194583759405334));
#51835=CARTESIAN_POINT('Ctrl Pts',(-48.786201121343,2.04582723566432,3.54365852664896));
#51836=CARTESIAN_POINT('Ctrl Pts',(-48.5873275896455,-1.87523844072396,
3.63681256351067));
#51837=CARTESIAN_POINT('Ctrl Pts',(-48.3884540579481,-4.07333118739941,
0.388455749651265));
#51838=CARTESIAN_POINT('Ctrl Pts',(-48.1895805262506,-2.5288388754331,-3.21681500459317));
#51839=CARTESIAN_POINT('Ctrl Pts',(-47.9907069945532,1.33915578767652,-3.86646952761948));
#51840=CARTESIAN_POINT('Ctrl Pts',(-47.7918334628557,3.97673136341719,-0.963603909753304));
#51841=CARTESIAN_POINT('Ctrl Pts',(-47.5929599311583,2.96047799713676,2.82462295893575));
#51842=CARTESIAN_POINT('Ctrl Pts',(-47.3940863994608,-0.775868631581208,
4.01758045323378));
#51843=CARTESIAN_POINT('Ctrl Pts',(-47.1952128677634,-3.79934556853258,
1.51917677791285));
#51844=CARTESIAN_POINT('Ctrl Pts',(-46.9963393360659,-3.33197599602417,
-2.37504964023841));
#51845=CARTESIAN_POINT('Ctrl Pts',(-46.7974658043685,0.196819963086194,
-4.08707557231434));
#51846=CARTESIAN_POINT('Ctrl Pts',(-46.598592272671,3.54477733598791,-2.04388807666766));
#51847=CARTESIAN_POINT('Ctrl Pts',(-46.3997187409736,3.63578601418986,1.87722798048059));
#51848=CARTESIAN_POINT('Ctrl Pts',(-46.2008452092761,0.386227037294444,
4.07354311470255));
#51849=CARTESIAN_POINT('Ctrl Pts',(-46.0019716775787,-3.2181981344964,2.52707847104148));
#51850=CARTESIAN_POINT('Ctrl Pts',(-45.8030981458811,-3.8657362524741,-1.34127106059329));
#51851=CARTESIAN_POINT('Ctrl Pts',(-45.6042246141838,-0.961427964268491,
-3.97725798775995));
#51852=CARTESIAN_POINT('Ctrl Pts',(-45.4053510824863,2.82624231158073,-2.95893210937808));
#51853=CARTESIAN_POINT('Ctrl Pts',(-45.2064775507888,4.01715534850376,0.778066666594522));
#51854=CARTESIAN_POINT('Ctrl Pts',(-45.0076040190914,1.51709780290662,3.80017619171714));
#51855=CARTESIAN_POINT('Ctrl Pts',(-44.8087304873939,-2.37687231901642,
3.33067602909248));
#51856=CARTESIAN_POINT('Ctrl Pts',(-44.6098569556966,-4.08696727386044,
-0.199056107848081));
#51857=CARTESIAN_POINT('Ctrl Pts',(-44.4109834239989,-2.04194830582366,
-3.54589508418139));
#51858=CARTESIAN_POINT('Ctrl Pts',(-44.2121098923016,1.87921695828035,-3.6347583764797));
#51859=CARTESIAN_POINT('Ctrl Pts',(-44.013236360604,4.07375382257173,-0.383998209318782));
#51860=CARTESIAN_POINT('Ctrl Pts',(-43.8143628289067,2.52531731015724,3.21958030101716));
#51861=CARTESIAN_POINT('Ctrl Pts',(-43.6154892972092,-1.34338593199437,
3.86500182010269));
#51862=CARTESIAN_POINT('Ctrl Pts',(-43.4166157655118,-3.97778342149215,
0.959251730975778));
#51863=CARTESIAN_POINT('Ctrl Pts',(-43.2177422338142,-2.95738533584939,
-2.82786081817702));
#51864=CARTESIAN_POINT('Ctrl Pts',(-43.0188687021169,0.780264468689989,
-4.0167290412197));
#51865=CARTESIAN_POINT('Ctrl Pts',(-42.8199951704193,3.80100567730137,-1.51501837375015));
#51866=CARTESIAN_POINT('Ctrl Pts',(-42.621121638722,3.32937506510755,2.37869428626672));
#51867=CARTESIAN_POINT('Ctrl Pts',(-42.4222481070244,-0.201292193021611,
4.08685775195398));
#51868=CARTESIAN_POINT('Ctrl Pts',(-42.223374575327,-3.54701177089477,2.04000792371299));
#51869=CARTESIAN_POINT('Ctrl Pts',(-42.0245010436295,-3.63372965068782,
-1.88120537352782));
#51870=CARTESIAN_POINT('Ctrl Pts',(-41.8256275119322,-0.381769266391471,
-4.07396331094387));
#51871=CARTESIAN_POINT('Ctrl Pts',(-41.6267539802346,3.22096150374165,-2.52355539330758));
#51872=CARTESIAN_POINT('Ctrl Pts',(-41.4278804485373,3.86426623072513,1.34550040124665));
#51873=CARTESIAN_POINT('Ctrl Pts',(-41.2290069168397,0.957075210526619,
3.97830766445649));
#51874=CARTESIAN_POINT('Ctrl Pts',(-41.0301333851423,-2.82947847824009,
2.95583767701373));
#51875=CARTESIAN_POINT('Ctrl Pts',(-40.8312598534449,-4.01630153150924,
-0.782462037209674));
#51876=CARTESIAN_POINT('Ctrl Pts',(-40.6323863217473,-1.51293849106592,
-3.801834025037));
#51877=CARTESIAN_POINT('Ctrl Pts',(-40.43351279005,2.38051554144388,-3.32807310445879));
#51878=CARTESIAN_POINT('Ctrl Pts',(-40.2346392583525,4.08674700662777,0.203528217937388));
#51879=CARTESIAN_POINT('Ctrl Pts',(-40.0357657266551,2.03806693091652,3.54812739579378));
#51880=CARTESIAN_POINT('Ctrl Pts',(-39.8368921949575,-1.88319322562777,
3.63269983712218));
#51881=CARTESIAN_POINT('Ctrl Pts',(-39.6380186632601,-4.07417157975626,
0.379540209179764));
#51882=CARTESIAN_POINT('Ctrl Pts',(-39.4391451315626,-2.52179272101996,
-3.22234174225643));
#51883=CARTESIAN_POINT('Ctrl Pts',(-39.2402715998652,1.34761446771718,-3.86352948456161));
#51884=CARTESIAN_POINT('Ctrl Pts',(-39.0413980681678,3.97883071649604,-0.954898403572573));
#51885=CARTESIAN_POINT('Ctrl Pts',(-38.8425245364703,2.9542891333344,2.8310952912857));
#51886=CARTESIAN_POINT('Ctrl Pts',(-38.6436510047728,-0.784659371495732,
4.01587281950036));
#51887=CARTESIAN_POINT('Ctrl Pts',(-38.4447774730754,-3.80266123467603,
1.51085815547656));
#51888=CARTESIAN_POINT('Ctrl Pts',(-38.2459039413779,-3.32677014753596,
-2.38233608400271));
#51889=CARTESIAN_POINT('Ctrl Pts',(-38.0470304096805,0.205764181926051,
-4.08663503791495));
#51890=CARTESIAN_POINT('Ctrl Pts',(-37.848156877983,3.54924195854446,-2.03612532801529));
#51891=CARTESIAN_POINT('Ctrl Pts',(-37.6492833462856,3.63166893609104,1.88518051398512));
#51892=CARTESIAN_POINT('Ctrl Pts',(-37.4504098145881,0.377311038351019,
4.0743786289465));
#51893=CARTESIAN_POINT('Ctrl Pts',(-37.2515362828907,-3.22372101614827,
2.5200292938221));
#51894=CARTESIAN_POINT('Ctrl Pts',(-37.0526627511932,-3.86279158183273,
-1.34972813077302));
#51895=CARTESIAN_POINT('Ctrl Pts',(-36.8537892194958,-0.952721310765272,
-3.97935257745422));
#51896=CARTESIAN_POINT('Ctrl Pts',(-36.6549156877983,2.83271125682985,-2.95273970527496));
#51897=CARTESIAN_POINT('Ctrl Pts',(-36.4560421561009,4.01544290532138,0.786856470890383));
#51898=CARTESIAN_POINT('Ctrl Pts',(-36.2571686244033,1.50877736760482,3.80348730597083));
#51899=CARTESIAN_POINT('Ctrl Pts',(-36.058295092706,-2.38415591339822,3.32546619472911));
#51900=CARTESIAN_POINT('Ctrl Pts',(-35.8594215610084,-4.08652184584904,
-0.208000084318258));
#51901=CARTESIAN_POINT('Ctrl Pts',(-35.6605480293111,-2.03418311559052,
-3.55035545881314));
#51902=CARTESIAN_POINT('Ctrl Pts',(-35.4616744976136,1.88716723800497,-3.63063694790301));
#51903=CARTESIAN_POINT('Ctrl Pts',(-35.2628009659162,4.07458445845272,-0.375081754572397));
#51904=CARTESIAN_POINT('Ctrl Pts',(-35.0639274342186,2.51826511224174,3.22509932500437));
#51905=CARTESIAN_POINT('Ctrl Pts',(-34.8650539025213,-1.35184138978157,
3.86205252275927));
#51906=CARTESIAN_POINT('Ctrl Pts',(-34.6661803708237,-3.97987324717481,
0.950543932756447));
#51907=CARTESIAN_POINT('Ctrl Pts',(-34.4673068391263,-2.95118939329924,
-2.83432637438878));
#51908=CARTESIAN_POINT('Ctrl Pts',(-34.2684333074289,0.789053334735911,
-4.015011789101));
#51909=CARTESIAN_POINT('Ctrl Pts',(-34.0695597757314,3.80431223867413,-1.50669612807361));
#51910=CARTESIAN_POINT('Ctrl Pts',(-33.870686244034,3.32416124642858,2.38597502908564));
#51911=CARTESIAN_POINT('Ctrl Pts',(-33.6718127123365,-0.210235924444678,
4.08640743046392));
#51912=CARTESIAN_POINT('Ctrl Pts',(-33.4729391806391,-3.5514678962665,2.03224029422364));
#51913=CARTESIAN_POINT('Ctrl Pts',(-33.2740656489416,-3.62960387286703,
-1.88915339709258));
#51914=CARTESIAN_POINT('Ctrl Pts',(-33.0751921172442,-0.372852358511318,
-4.07478906821323));
#51915=CARTESIAN_POINT('Ctrl Pts',(-32.8763185855467,3.22647666841207,-2.51650017680708));
#51916=CARTESIAN_POINT('Ctrl Pts',(-32.6774450538492,3.86131230756254,1.35395424411015));
#51917=CARTESIAN_POINT('Ctrl Pts',(-32.4785715221518,0.9483662701979,3.98039272550194));
#51918=CARTESIAN_POINT('Ctrl Pts',(-32.2796979904543,-2.83594064347902,
2.94963819787132));
#51919=CARTESIAN_POINT('Ctrl Pts',(-32.0808244587569,-4.01457947096827,
-0.791249962374674));
#51920=CARTESIAN_POINT('Ctrl Pts',(-31.8819509270594,-1.50461443750595,
-3.80513603253898));
#51921=CARTESIAN_POINT('Ctrl Pts',(-31.683077395362,2.3877934305204,-3.32285530302501));
#51922=CARTESIAN_POINT('Ctrl Pts',(-31.4842038636645,4.08629179179384,0.212471701636003));
#51923=CARTESIAN_POINT('Ctrl Pts',(-31.285330331967,2.03029686449623,3.55257927057153));
#51924=CARTESIAN_POINT('Ctrl Pts',(-31.0864568002696,-1.89113899065338,
3.62856971129236));
#51925=CARTESIAN_POINT('Ctrl Pts',(-30.8875832685721,-4.07499245816681,
0.370622850835159));
#51926=CARTESIAN_POINT('Ctrl Pts',(-30.6887097368747,-2.51473448804646,
-3.22785304595907));
#51927=CARTESIAN_POINT('Ctrl Pts',(-30.4898362051772,1.35606669312626,-3.86057093646411));
#51928=CARTESIAN_POINT('Ctrl Pts',(-30.2909626734798,3.98091101228011,-0.946188323741529));
#51929=CARTESIAN_POINT('Ctrl Pts',(-30.0920891417823,2.94808611945558,2.83755406361732));
#51930=CARTESIAN_POINT('Ctrl Pts',(-29.8932156100849,-0.793446353149102,
4.01414595105263));
#51931=CARTESIAN_POINT('Ctrl Pts',(-29.6943420783874,-3.80595868731876,
1.50253229652499));
#51932=CARTESIAN_POINT('Ctrl Pts',(-29.49546854669,-3.32154836490935,-2.38961111715816));
#51933=CARTESIAN_POINT('Ctrl Pts',(-29.2965950149925,0.214707415222938,
-4.08617492987343));
#51934=CARTESIAN_POINT('Ctrl Pts',(-29.0977214832951,3.55368958139554,-2.02835282699007));
#51935=CARTESIAN_POINT('Ctrl Pts',(-28.8988479515976,3.62753446348856,1.89312401809299));
#51936=CARTESIAN_POINT('Ctrl Pts',(-28.6999744199002,0.368393232211336,
4.07519462825255));
#51937=CARTESIAN_POINT('Ctrl Pts',(-28.5011008882027,-3.22922845723333,
2.51296804648844));
#51938=CARTESIAN_POINT('Ctrl Pts',(-28.3022273565053,-3.85982840968593,
-1.35817873619754));
#51939=CARTESIAN_POINT('Ctrl Pts',(-28.1033538248078,-0.944010094039302,
-3.98142810735417));
#51940=CARTESIAN_POINT('Ctrl Pts',(-27.9044802931104,2.83916663432068,-2.94653315851663));
#51941=CARTESIAN_POINT('Ctrl Pts',(-27.7056067614129,4.01371122948384,0.795642506401697));
#51942=CARTESIAN_POINT('Ctrl Pts',(-27.5067332297155,1.50044970575405,3.80678020276722));
#51943=CARTESIAN_POINT('Ctrl Pts',(-27.307859698018,-2.39142808845478,3.32024043247283));
#51944=CARTESIAN_POINT('Ctrl Pts',(-27.1089861663205,-4.08605684473766,
-0.216943064536219));
#51945=CARTESIAN_POINT('Ctrl Pts',(-26.9101126346231,-2.02640818228711,
-3.55479882840614));
#51946=CARTESIAN_POINT('Ctrl Pts',(-26.7112391029256,1.89510847881717,-3.62649812976556));
#51947=CARTESIAN_POINT('Ctrl Pts',(-26.5123655712282,4.07539557840993,-0.366163503307297));
#51948=CARTESIAN_POINT('Ctrl Pts',(-26.3134920395307,2.51120085266183,3.23060290182313));
#51949=CARTESIAN_POINT('Ctrl Pts',(-26.1146185078333,-1.36029037269174,
3.85908472745028));
#51950=CARTESIAN_POINT('Ctrl Pts',(-25.9157449761358,-3.9819440105693,0.941831581743292));
#51951=CARTESIAN_POINT('Ctrl Pts',(-25.7168714444383,-2.94497931551936,
-2.84077835510638));
#51952=CARTESIAN_POINT('Ctrl Pts',(-25.5179979127409,0.797838421475032,
-4.01327530639203));
#51953=CARTESIAN_POINT('Ctrl Pts',(-25.3191243810434,3.80760057863841,-1.49836666581655));
#51954=CARTESIAN_POINT('Ctrl Pts',(-25.120250849346,3.31893150610698,2.39324434386635));
#51955=CARTESIAN_POINT('Ctrl Pts',(-24.9213773176485,-0.219178648906594,
4.08593753642188));
#51956=CARTESIAN_POINT('Ctrl Pts',(-24.7225037859511,-3.55590701127126,
2.0244629309695));
#51957=CARTESIAN_POINT('Ctrl Pts',(-24.5236302542536,-3.62546071043357,
-1.89709237223187));
#51958=CARTESIAN_POINT('Ctrl Pts',(-24.3247567225562,-0.363933664790518,
-4.07559530857881));
#51959=CARTESIAN_POINT('Ctrl Pts',(-24.1258831908587,3.23197637931701,-2.50943290709563));
#51960=CARTESIAN_POINT('Ctrl Pts',(-23.9270096591613,3.85833988997977,1.36240160197672));
#51961=CARTESIAN_POINT('Ctrl Pts',(-23.7281361274638,0.939652787505642,
3.9824587217711));
#51962=CARTESIAN_POINT('Ctrl Pts',(-23.5292625957663,-2.84238922549196,
2.94342459092891));
#51963=CARTESIAN_POINT('Ctrl Pts',(-23.3303890640689,-4.01283818190772,
-0.800034097711746));
#51964=CARTESIAN_POINT('Ctrl Pts',(-23.1315155323714,-1.49628317733607,
-3.80841981468678));
#51965=CARTESIAN_POINT('Ctrl Pts',(-22.932642000674,2.39505988284916,-3.31762158620365));
#51966=CARTESIAN_POINT('Ctrl Pts',(-22.7337684689765,4.08581700496182,0.221414167664817));
#51967=CARTESIAN_POINT('Ctrl Pts',(-22.5348949372791,2.02251707361955,3.55701412965921));
#51968=CARTESIAN_POINT('Ctrl Pts',(-22.3360214055816,-1.8990756977432,3.62442220580315));
#51969=CARTESIAN_POINT('Ctrl Pts',(-22.1371478738842,-4.0757938186994,0.361703717328525));
#51970=CARTESIAN_POINT('Ctrl Pts',(-21.9382743421867,-2.50766421031908,
-3.23334888930383));
#51971=CARTESIAN_POINT('Ctrl Pts',(-21.7394008104893,1.36451242342049,-3.85759389749737));
#51972=CARTESIAN_POINT('Ctrl Pts',(-21.5405272787918,3.98297224080547,-0.937473711978594));
#51973=CARTESIAN_POINT('Ctrl Pts',(-21.3416537470944,2.9418689852107,2.84399924499518));
#51974=CARTESIAN_POINT('Ctrl Pts',(-21.1427802153969,-0.80222953445455,
4.01239985616173));
#51975=CARTESIAN_POINT('Ctrl Pts',(-20.9439066836995,-3.80923791066707,
1.4941992409363));
#51976=CARTESIAN_POINT('Ctrl Pts',(-20.745033152002,-3.31631067315495,-2.39687470485972));
#51977=CARTESIAN_POINT('Ctrl Pts',(-20.5461596203046,0.22364962014169,-4.08569525039353));
#51978=CARTESIAN_POINT('Ctrl Pts',(-20.3472860886071,3.55812018323851,-2.02057061081977));
#51979=CARTESIAN_POINT('Ctrl Pts',(-20.1484125569097,3.6233826161852,1.90105845475743));
#51980=CARTESIAN_POINT('Ctrl Pts',(-19.9495390252122,0.359473661588844,
4.07599110871226));
#51981=CARTESIAN_POINT('Ctrl Pts',(-19.7506654935147,-3.2347204313727,2.50589476286167));
#51982=CARTESIAN_POINT('Ctrl Pts',(-19.5517919618173,-3.85684675022641,
-1.36662283639115));
#51983=CARTESIAN_POINT('Ctrl Pts',(-19.3529184301198,-0.935294355814451,
-3.98348456751868));
#51984=CARTESIAN_POINT('Ctrl Pts',(-19.1540448984224,2.84560841313408,-2.94031249883042));
#51985=CARTESIAN_POINT('Ctrl Pts',(-18.9551713667249,4.0119603292853,0.804424731046237));
#51986=CARTESIAN_POINT('Ctrl Pts',(-18.7562978350274,1.49211485724107,3.81005486633438));
#51987=CARTESIAN_POINT('Ctrl Pts',(-18.55742430333,-2.39868880935476,3.31499876735332));
#51988=CARTESIAN_POINT('Ctrl Pts',(-18.3585507716326,-4.0855722727535,-0.225885005668014));
#51989=CARTESIAN_POINT('Ctrl Pts',(-18.1596772399351,-2.01862354315282,
-3.5592251716781));
#51990=CARTESIAN_POINT('Ctrl Pts',(-17.9608037082376,1.90304064268095,-3.6223419418909));
#51991=CARTESIAN_POINT('Ctrl Pts',(-17.7619301765402,4.07618717855833,-0.357243498239154));
#51992=CARTESIAN_POINT('Ctrl Pts',(-17.5630566448428,2.50412456525315,3.23609100511305));
#51993=CARTESIAN_POINT('Ctrl Pts',(-17.3641831131453,-1.36873284025696,
3.85609844839054));
#51994=CARTESIAN_POINT('Ctrl Pts',(-17.1653095814478,-3.98399570175737,
0.933114719665619));
#51995=CARTESIAN_POINT('Ctrl Pts',(-16.9664360497504,-2.93875513225399,
-2.84721672942694));
#51996=CARTESIAN_POINT('Ctrl Pts',(-16.7675625180529,0.806619686829663,
-4.01151960141));
#51997=CARTESIAN_POINT('Ctrl Pts',(-16.5686889863555,3.81087068144415,-1.49003002687437));
#51998=CARTESIAN_POINT('Ctrl Pts',(-16.369815454658,3.31368586919149,2.40050219579121));
#51999=CARTESIAN_POINT('Ctrl Pts',(-16.1709419229606,-0.22812032357462,
4.08544807207852));
#52000=CARTESIAN_POINT('Ctrl Pts',(-15.9720683912631,-3.56032909464717,
2.01667587120158));
#52001=CARTESIAN_POINT('Ctrl Pts',(-15.7731948595656,-3.6213001832318,-1.90502226092053));
#52002=CARTESIAN_POINT('Ctrl Pts',(-15.5743213278682,-0.355013227946878,
-4.07638202817894));
#52003=CARTESIAN_POINT('Ctrl Pts',(-15.3754477961708,3.2374606101146,-2.50235361802328));
#52004=CARTESIAN_POINT('Ctrl Pts',(-15.1765742644733,3.85534899221378,1.37084243438626));
#52005=CARTESIAN_POINT('Ctrl Pts',(-14.9777007327758,0.93093480418458,3.98450564336853));
#52006=CARTESIAN_POINT('Ctrl Pts',(-14.7788272010784,-2.84882419339231,
2.93719688594763));
#52007=CARTESIAN_POINT('Ctrl Pts',(-14.5799536693809,-4.01107767266776,
-0.808814401147756));
#52008=CARTESIAN_POINT('Ctrl Pts',(-14.3810801376835,-1.48794475046029,
-3.81168535575216));
#52009=CARTESIAN_POINT('Ctrl Pts',(-14.182206605986,2.40231486362624,-3.31237197906248));
#52010=CARTESIAN_POINT('Ctrl Pts',(-13.9833330742886,4.08532264840576,0.230355573192351));
#52011=CARTESIAN_POINT('Ctrl Pts',(-13.7844595425911,2.01472759554911,3.56143195181527));
#52012=CARTESIAN_POINT('Ctrl Pts',(-13.5855860108937,-1.90700330888289,
3.62025734051975));
#52013=CARTESIAN_POINT('Ctrl Pts',(-13.3867124791962,-4.07657565751574,
0.352782851379752));
#52014=CARTESIAN_POINT('Ctrl Pts',(-13.1878389474988,-2.50058192170229,
-3.23882924596736));
#52015=CARTESIAN_POINT('Ctrl Pts',(-12.9889654158013,1.37295161814754,-3.85459838192047));
#52016=CARTESIAN_POINT('Ctrl Pts',(-12.7900918841038,3.9850143921995,-0.928754610023908));
#52017=CARTESIAN_POINT('Ctrl Pts',(-12.5912183524064,2.9356377603778,2.85043080454899));
#52018=CARTESIAN_POINT('Ctrl Pts',(-12.3923448207089,-0.811008873343517,
4.01063454319088));
#52019=CARTESIAN_POINT('Ctrl Pts',(-12.1934712890115,-3.81249888901455,
1.48585902862307));
#52020=CARTESIAN_POINT('Ctrl Pts',(-11.994597757314,-3.31105709735959,-2.4041268123172));
#52021=CARTESIAN_POINT('Ctrl Pts',(-11.7957242256166,0.23259075385208,-4.08519600177279));
#52022=CARTESIAN_POINT('Ctrl Pts',(-11.5968506939191,3.56253374285225,-2.01277871677862));
#52023=CARTESIAN_POINT('Ctrl Pts',(-11.3979771622217,3.61921341406693,1.908983785975));
#52024=CARTESIAN_POINT('Ctrl Pts',(-11.1991036305242,0.350552369205444,
4.07676806651077));
#52025=CARTESIAN_POINT('Ctrl Pts',(-11.0002300988268,-3.24019691226161,
2.49880947682055));
#52026=CARTESIAN_POINT('Ctrl Pts',(-10.8013565671293,-3.85384661773532,
-1.3750603909094));
#52027=CARTESIAN_POINT('Ctrl Pts',(-10.6024830354319,-0.926574137836242,
-3.985521948098));
#52028=CARTESIAN_POINT('Ctrl Pts',(-10.4036095037344,2.85203656241603,-2.93407775601124));
#52029=CARTESIAN_POINT('Ctrl Pts',(-10.204735972037,4.010190213112,0.813203102760025));
#52030=CARTESIAN_POINT('Ctrl Pts',(-10.0058624403395,1.48377286198708,3.81331128098776));
#52031=CARTESIAN_POINT('Ctrl Pts',(-9.80698890864205,-2.40593804132169,
3.30974122447646));
#52032=CARTESIAN_POINT('Ctrl Pts',(-9.60811537694457,-4.08506813221747,
-0.234825864884617));
#52033=CARTESIAN_POINT('Ctrl Pts',(-9.40924184524715,-2.01082923547359,
-3.56363446742823));
#52034=CARTESIAN_POINT('Ctrl Pts',(-9.21036831354969,1.91096369160394,-3.61816840418592));
#52035=CARTESIAN_POINT('Ctrl Pts',(-9.01149478185224,4.07695925510639,-0.348321782091731));
#52036=CARTESIAN_POINT('Ctrl Pts',(-8.81262125015477,2.4970362839087,3.24156360858787));
#52037=CARTESIAN_POINT('Ctrl Pts',(-8.61374771845734,-1.37716875204044,
3.85309369988341));
#52038=CARTESIAN_POINT('Ctrl Pts',(-8.41487418675986,-3.98602831091206,
0.924393388274425));
#52039=CARTESIAN_POINT('Ctrl Pts',(-8.21600065506242,-2.93251687331501,
-2.85364146651265));
#52040=CARTESIAN_POINT('Ctrl Pts',(-8.01712712336496,0.81539708874029,-4.00974468256414));
#52041=CARTESIAN_POINT('Ctrl Pts',(-7.8182535916675,3.81412253142865,-1.481686251177));
#52042=CARTESIAN_POINT('Ctrl Pts',(-7.61938005997007,3.30842436080689,2.40774855009751));
#52043=CARTESIAN_POINT('Ctrl Pts',(-7.4205065282726,-0.237060905620641,
4.08493903977805));
#52044=CARTESIAN_POINT('Ctrl Pts',(-7.22163299657515,-3.56473412521439,
2.00887915221773));
#52045=CARTESIAN_POINT('Ctrl Pts',(-7.0227594648777,-3.61712231118831,-1.91294302517764));
#52046=CARTESIAN_POINT('Ctrl Pts',(-6.82388593318022,-0.346091090708137,
-4.07714922324453));
#52047=CARTESIAN_POINT('Ctrl Pts',(-6.6250124014828,3.24292933454114,-2.49526234349918));
#52048=CARTESIAN_POINT('Ctrl Pts',(-6.42613886978531,3.85233962858262,1.37927670091363));
#52049=CARTESIAN_POINT('Ctrl Pts',(-6.22726533808788,0.92221236200472,3.98653348048341));
#52050=CARTESIAN_POINT('Ctrl Pts',(-6.0283918063904,-2.85524551638475,2.93095511276885));
#52051=CARTESIAN_POINT('Ctrl Pts',(-5.82951827469298,-4.0092979516314,-0.81759083065191));
#52052=CARTESIAN_POINT('Ctrl Pts',(-5.63064474299553,-1.47959919691017,
-3.81493264004876));
#52053=CARTESIAN_POINT('Ctrl Pts',(-5.43177121129806,2.40955833827837,-3.30710650683126));
#52054=CARTESIAN_POINT('Ctrl Pts',(-5.23289767960062,4.08480872416158,0.239295875554097));
#52055=CARTESIAN_POINT('Ctrl Pts',(-5.03402414790315,2.00692846822076,3.56583271557382));
#52056=CARTESIAN_POINT('Ctrl Pts',(-4.83515061620571,-1.91492178728529,
3.61607513596826));
#52057=CARTESIAN_POINT('Ctrl Pts',(-4.63627708450823,-4.07733796863674,
0.343860294625829));
#52058=CARTESIAN_POINT('Ctrl Pts',(-4.43740355281079,-2.49348766033667,
-3.24429408764104));
#52059=CARTESIAN_POINT('Ctrl Pts',(-4.23853002111333,1.38138424485284,-3.85158440796985));
#52060=CARTESIAN_POINT('Ctrl Pts',(-4.03965648941587,3.98703744163902,-0.920031052295885));
#52061=CARTESIAN_POINT('Ctrl Pts',(-3.84078295771845,2.92939250320468,2.85684869760832));
#52062=CARTESIAN_POINT('Ctrl Pts',(-3.64190942602098,-0.819784381395129,
4.00885004677589));
#52063=CARTESIAN_POINT('Ctrl Pts',(-3.44303589432354,-3.81574150547896,
1.47751165009818));
#52064=CARTESIAN_POINT('Ctrl Pts',(-3.24416236262606,-3.30578785389167,
-2.41136731145358));
#52065=CARTESIAN_POINT('Ctrl Pts',(-3.04528883092862,0.241531134563617,
-4.08467736265059));
#52066=CARTESIAN_POINT('Ctrl Pts',(-2.84641529923116,3.56692955739015,-2.00497684939494));
#52067=CARTESIAN_POINT('Ctrl Pts',(-2.6475417675337,3.61502816430448,1.91689934540635));
#52068=CARTESIAN_POINT('Ctrl Pts',(-2.44866823583624,0.341626967292691,
4.07752668443549));
#52069=CARTESIAN_POINT('Ctrl Pts',(-2.24979470413878,-3.24565328439454,
2.49170998193123));
#52070=CARTESIAN_POINT('Ctrl Pts',(-2.05092117244136,-3.85083669206714,
-1.38348712906526));
#52071=CARTESIAN_POINT('Ctrl Pts',(-1.85204764074388,-0.917833119671589,
-3.98754822695286));
#52072=CARTESIAN_POINT('Ctrl Pts',(-1.65317410904645,2.85842015619851,-2.92781387766021));
#52073=CARTESIAN_POINT('Ctrl Pts',(-1.45430057734898,4.00845922597162,0.82194910102392));
#52074=CARTESIAN_POINT('Ctrl Pts',(-1.25542704565154,1.47531360750824,3.81660320507337));
#52075=CARTESIAN_POINT('Ctrl Pts',(-1.05655351395407,-2.41296774955078,
3.30436628639575));
#52076=CARTESIAN_POINT('Ctrl Pts',(-0.857679982256626,-4.08493725274729,
-0.243573813186974));
#52077=CARTESIAN_POINT('Ctrl Pts',(-0.658806450559161,-2.00228289876901,
-3.56838925950682));
#52078=CARTESIAN_POINT('Ctrl Pts',(-0.459932918861702,1.91747039222746,
-3.61328939493983));
#52079=CARTESIAN_POINT('Ctrl Pts',(-0.261059387164285,4.08041299153864,
-0.340726701072281));
#52080=CARTESIAN_POINT('Ctrl Pts',(-0.0621858554667818,2.48447621485804,
3.24976209445823));
#52081=CARTESIAN_POINT('Ctrl Pts',(0.0703964989981598,-0.0868243742411749,
3.6454708254482));
#52082=CARTESIAN_POINT('Ctrl Pts',(0.136687676230641,-1.17148016637885,
3.25511512389055));
#52083=CARTESIAN_POINT('Ctrl Pts',(-109.703687676231,-1.64343044862366,
3.31080057131755));
#52084=CARTESIAN_POINT('Ctrl Pts',(-109.637396498998,-2.74664151170901,
2.7631835786059));
#52085=CARTESIAN_POINT('Ctrl Pts',(-109.504814144533,-4.34329544588056,
0.487898524808049));
#52086=CARTESIAN_POINT('Ctrl Pts',(-109.305940612836,-2.75520708479667,
-3.39822806350164));
#52087=CARTESIAN_POINT('Ctrl Pts',(-109.107067081138,1.36785846604787,-4.15091025735692));
#52088=CARTESIAN_POINT('Ctrl Pts',(-108.908193549441,4.23233807130361,-1.09535677627866));
#52089=CARTESIAN_POINT('Ctrl Pts',(-108.709320017743,3.20908102854513,2.96956032317362));
#52090=CARTESIAN_POINT('Ctrl Pts',(-108.510446486046,-0.763185572783635,
4.30448238078623));
#52091=CARTESIAN_POINT('Ctrl Pts',(-108.311572954348,-4.03397135422629,
1.68526123531646));
#52092=CARTESIAN_POINT('Ctrl Pts',(-108.112699422651,-3.59847596118754,
-2.48281775018356));
#52093=CARTESIAN_POINT('Ctrl Pts',(-107.913825890954,0.143380670774777,
-4.3694476002038));
#52094=CARTESIAN_POINT('Ctrl Pts',(-107.714952359256,3.75345958488109,-2.24154240806525));
#52095=CARTESIAN_POINT('Ctrl Pts',(-107.516078827559,3.91487291942144,1.9459613663452));
#52096=CARTESIAN_POINT('Ctrl Pts',(-107.317205295861,0.479281964767665,
4.34547751537191));
#52097=CARTESIAN_POINT('Ctrl Pts',(-107.118331764164,-3.39666841093264,
2.75237818021938));
#52098=CARTESIAN_POINT('Ctrl Pts',(-106.919458232466,-4.15175596517978,
-1.36962150618047));
#52099=CARTESIAN_POINT('Ctrl Pts',(-106.720584700769,-1.09219997809354,
-4.23320504153245));
#52100=CARTESIAN_POINT('Ctrl Pts',(-106.521711169071,2.97087072510216,-3.20731379323168));
#52101=CARTESIAN_POINT('Ctrl Pts',(-106.322837637374,4.30429976488753,0.765465383938776));
#52102=CARTESIAN_POINT('Ctrl Pts',(-106.123964105677,1.68292909980025,4.03493263721933));
#52103=CARTESIAN_POINT('Ctrl Pts',(-105.925090573979,-2.4847201490054,3.59709589973779));
#52104=CARTESIAN_POINT('Ctrl Pts',(-105.726217042282,-4.36940349125203,
-0.145760148682));
#52105=CARTESIAN_POINT('Ctrl Pts',(-105.527343510584,-2.2394698980649,-3.75469136069795));
#52106=CARTESIAN_POINT('Ctrl Pts',(-105.328469978887,1.94809321659027,-3.91380450068533));
#52107=CARTESIAN_POINT('Ctrl Pts',(-105.129596447189,4.34574429399991,-0.476905997778922));
#52108=CARTESIAN_POINT('Ctrl Pts',(-104.930722915492,2.7505165857232,3.39817469839221));
#52109=CARTESIAN_POINT('Ctrl Pts',(-104.731849383794,-1.37189140623665,
4.15100551315273));
#52110=CARTESIAN_POINT('Ctrl Pts',(-104.532975852097,-4.23380275878313,
1.08988393459526));
#52111=CARTESIAN_POINT('Ctrl Pts',(-104.334102320399,-3.20568744261217,
-2.97262523841459));
#52112=CARTESIAN_POINT('Ctrl Pts',(-104.135228788702,0.767820077559129,
-4.30388024007402));
#52113=CARTESIAN_POINT('Ctrl Pts',(-103.936355257005,4.03585293414859,-1.68072123941791));
#52114=CARTESIAN_POINT('Ctrl Pts',(-103.737481725307,3.59573582801791,2.48668788662542));
#52115=CARTESIAN_POINT('Ctrl Pts',(-103.53860819361,-0.148150739858707,
4.3693230767846));
#52116=CARTESIAN_POINT('Ctrl Pts',(-103.339734661912,-3.75591610379247,
2.23741525247945));
#52117=CARTESIAN_POINT('Ctrl Pts',(-103.140861130215,-3.91273803962465,
-1.9502342997724));
#52118=CARTESIAN_POINT('Ctrl Pts',(-102.941987598517,-0.474528230741329,
-4.34600457305979));
#52119=CARTESIAN_POINT('Ctrl Pts',(-102.74311406682,3.39967909088784,-2.74865692107253));
#52120=CARTESIAN_POINT('Ctrl Pts',(-102.544240535122,4.15025428333885,1.37416235372989));
#52121=CARTESIAN_POINT('Ctrl Pts',(-102.345367003425,1.08756731865623,4.23439843639973));
#52122=CARTESIAN_POINT('Ctrl Pts',(-102.146493471728,-2.97437873148058,
3.20406054132907));
#52123=CARTESIAN_POINT('Ctrl Pts',(-101.94761994003,-4.30345949592243,-0.77017475792313));
#52124=CARTESIAN_POINT('Ctrl Pts',(-101.748746408333,-1.67851283933561,
-4.03677190821751));
#52125=CARTESIAN_POINT('Ctrl Pts',(-101.549872876635,2.48865486047723,-3.59437474064827));
#52126=CARTESIAN_POINT('Ctrl Pts',(-101.350999344938,4.36924136459678,0.150541318859443));
#52127=CARTESIAN_POINT('Ctrl Pts',(-101.15212581324,2.23535993168143,3.75713970549685));
#52128=CARTESIAN_POINT('Ctrl Pts',(-100.953252281543,-1.95237479626607,
3.91167041629182));
#52129=CARTESIAN_POINT('Ctrl Pts',(-100.754378749845,-4.34626355264668,
0.472150316872331));
#52130=CARTESIAN_POINT('Ctrl Pts',(-100.555505218148,-2.74679643279182,
-3.40118246314275));
#52131=CARTESIAN_POINT('Ctrl Pts',(-100.356631686451,1.37643288943393,-4.14950181246763));
#52132=CARTESIAN_POINT('Ctrl Pts',(-100.157758154753,4.23499284665589,-1.08525037643902));
#52133=CARTESIAN_POINT('Ctrl Pts',(-99.9588846230556,3.20243268077579,2.97613133377659));
#52134=CARTESIAN_POINT('Ctrl Pts',(-99.7600110913579,-0.772529207668281,
4.30303746370945));
#52135=CARTESIAN_POINT('Ctrl Pts',(-99.5611375596606,-4.0376896738937,1.67630393667729));
#52136=CARTESIAN_POINT('Ctrl Pts',(-99.362264027963,-3.59301257726815,-2.49062108928285));
#52137=CARTESIAN_POINT('Ctrl Pts',(-99.1633904962658,0.152931852785523,
-4.36915834448594));
#52138=CARTESIAN_POINT('Ctrl Pts',(-98.9645169645681,3.75836218248909,-2.2333039417024));
#52139=CARTESIAN_POINT('Ctrl Pts',(-98.7656434328708,3.91060162197971,1.95451470829903));
#52140=CARTESIAN_POINT('Ctrl Pts',(-98.5667699011732,0.469772261664343,
4.34652123116388));
#52141=CARTESIAN_POINT('Ctrl Pts',(-98.367896369476,-3.40268481723872,2.74493512224255));
#52142=CARTESIAN_POINT('Ctrl Pts',(-98.1690228377782,-4.14874809942346,
-1.37870301309521));
#52143=CARTESIAN_POINT('Ctrl Pts',(-97.970149306081,-1.08293310934729,-4.23558598914802));
#52144=CARTESIAN_POINT('Ctrl Pts',(-97.7712757743834,2.97788304515402,-3.20080386155913));
#52145=CARTESIAN_POINT('Ctrl Pts',(-97.5724022426862,4.30261414336226,0.774883426153052));
#52146=CARTESIAN_POINT('Ctrl Pts',(-97.3735287109885,1.67409453220965,4.03860623086893));
#52147=CARTESIAN_POINT('Ctrl Pts',(-97.1746551792912,-2.49258657250956,
3.59164933830304));
#52148=CARTESIAN_POINT('Ctrl Pts',(-96.9757816475936,-4.36907401644734,
-0.155322340930722));
#52149=CARTESIAN_POINT('Ctrl Pts',(-96.7769081158962,-2.23124728317354,
-3.75958353439823));
#52150=CARTESIAN_POINT('Ctrl Pts',(-96.5780345841988,1.95665403523896,-3.90953165701095));
#52151=CARTESIAN_POINT('Ctrl Pts',(-96.3791610525013,4.34677760852986,-0.467394065827876));
#52152=CARTESIAN_POINT('Ctrl Pts',(-96.1802875208038,2.74307298998427,3.40418615272527));
#52153=CARTESIAN_POINT('Ctrl Pts',(-95.9814139891064,-1.38097272403537,
4.14799314443235));
#52154=CARTESIAN_POINT('Ctrl Pts',(-95.7825404574089,-4.23617786369789,
1.08061551807453));
#52155=CARTESIAN_POINT('Ctrl Pts',(-95.5836669257115,-3.19917408416705,
-2.97963386508839));
#52156=CARTESIAN_POINT('Ctrl Pts',(-95.384793394014,0.77723741267289,-4.30218953500764));
#52157=CARTESIAN_POINT('Ctrl Pts',(-95.1859198623165,4.03952157886872,-1.67188462659408));
#52158=CARTESIAN_POINT('Ctrl Pts',(-94.9870463306192,3.5902850241611,2.49455130956892));
#52159=CARTESIAN_POINT('Ctrl Pts',(-94.7881727989216,-0.157712782579426,
4.36898838050624));
#52160=CARTESIAN_POINT('Ctrl Pts',(-94.5892992672242,-3.76080376085868,
2.22918995671049));
#52161=CARTESIAN_POINT('Ctrl Pts',(-94.3904257355267,-3.90846052170578,
-1.95879277644548));
#52162=CARTESIAN_POINT('Ctrl Pts',(-94.1915522038293,-0.465015730074829,
-4.34703268466786));
#52163=CARTESIAN_POINT('Ctrl Pts',(-93.9926786721319,3.40568646915293,-2.74121003657442));
#52164=CARTESIAN_POINT('Ctrl Pts',(-93.7938051404342,4.14723694772034,1.38324202157495));
#52165=CARTESIAN_POINT('Ctrl Pts',(-93.5949316087372,1.07829760331451,4.23676847012835));
#52166=CARTESIAN_POINT('Ctrl Pts',(-93.3960580770393,-2.9813837930556,3.1975433490874));
#52167=CARTESIAN_POINT('Ctrl Pts',(-93.1971845453423,-4.30176363877268,
-0.779591166523121));
#52168=CARTESIAN_POINT('Ctrl Pts',(-92.9983110136444,-1.66967422049213,
-4.04043571761904));
#52169=CARTESIAN_POINT('Ctrl Pts',(-92.7994374819473,2.49651529987284,-3.58891963525074));
#52170=CARTESIAN_POINT('Ctrl Pts',(-92.6005639502496,4.36890143668827,0.16010317701611));
#52171=CARTESIAN_POINT('Ctrl Pts',(-92.4016904185522,2.2271319629291,3.76202286150513));
#52172=CARTESIAN_POINT('Ctrl Pts',(-92.2028168868548,-1.96093093127833,
3.9073882163849));
#52173=CARTESIAN_POINT('Ctrl Pts',(-92.0039433551572,-4.34728645950153,
0.462637255117168));
#52174=CARTESIAN_POINT('Ctrl Pts',(-91.8050698234599,-2.73934626257066,
-3.40718576607261));
#52175=CARTESIAN_POINT('Ctrl Pts',(-91.6061962917623,1.38551090503464,-4.14647950951377));
#52176=CARTESIAN_POINT('Ctrl Pts',(-91.4073227600651,4.23735780826257,-1.07597936576111));
#52177=CARTESIAN_POINT('Ctrl Pts',(-91.2084492283674,3.19591165680837,2.98313282853178));
#52178=CARTESIAN_POINT('Ctrl Pts',(-91.0095756966701,-0.781944686999132,
4.3013364547849));
#52179=CARTESIAN_POINT('Ctrl Pts',(-90.8107021649725,-4.04134864684625,
1.66746331456547));
#52180=CARTESIAN_POINT('Ctrl Pts',(-90.6118286332753,-3.5875531719807,-2.49847854283336));
#52181=CARTESIAN_POINT('Ctrl Pts',(-90.4129551015775,0.162493523525171,
-4.36881318501945));
#52182=CARTESIAN_POINT('Ctrl Pts',(-90.2140815698803,3.76324083597265,-2.22507330244547));
#52183=CARTESIAN_POINT('Ctrl Pts',(-90.0152080381827,3.90631474136929,1.96306849909743));
#52184=CARTESIAN_POINT('Ctrl Pts',(-89.8163345064852,0.460258641666905,
4.34753893295489));
#52185=CARTESIAN_POINT('Ctrl Pts',(-89.617460974788,-3.40868404303548,2.73748166853095));
#52186=CARTESIAN_POINT('Ctrl Pts',(-89.4185874430904,-4.1457208300394,-1.38777937373523));
#52187=CARTESIAN_POINT('Ctrl Pts',(-89.2197139113929,-1.07366080610832,
-4.23794587792415));
#52188=CARTESIAN_POINT('Ctrl Pts',(-89.0208403796957,2.98488097099337,-3.19427900781841));
#52189=CARTESIAN_POINT('Ctrl Pts',(-88.8219668479979,4.30090798317216,0.78429797339638));
#52190=CARTESIAN_POINT('Ctrl Pts',(-88.6230933163007,1.66525190947596,4.04226036627706));
#52191=CARTESIAN_POINT('Ctrl Pts',(-88.4242197846031,-2.50044103786279,
3.58618563476002));
#52192=CARTESIAN_POINT('Ctrl Pts',(-88.2253462529058,-4.36872362552622,
-0.164883821391037));
#52193=CARTESIAN_POINT('Ctrl Pts',(-88.0264727212081,-2.22301397587585,
-3.76445768389663));
#52194=CARTESIAN_POINT('Ctrl Pts',(-87.8275991895109,1.96520547926291,-3.9052400969803));
#52195=CARTESIAN_POINT('Ctrl Pts',(-87.6287256578132,4.34779010495238,-0.457879890436096));
#52196=CARTESIAN_POINT('Ctrl Pts',(-87.4298521261159,2.73561625501344,3.41018129959302));
#52197=CARTESIAN_POINT('Ctrl Pts',(-87.2309785944184,-1.39004742699766,
4.14496090952432));
#52198=CARTESIAN_POINT('Ctrl Pts',(-87.0321050627209,-4.23853267893703,
1.07134192505021));
#52199=CARTESIAN_POINT('Ctrl Pts',(-86.8332315310236,-3.19264540260626,
-2.98662821991703));
#52200=CARTESIAN_POINT('Ctrl Pts',(-86.634357999326,0.786651025010412,-4.30047822406273));
#52201=CARTESIAN_POINT('Ctrl Pts',(-86.4354844676287,4.04317087563854,-1.66304000588559));
#52202=CARTESIAN_POINT('Ctrl Pts',(-86.2366109359312,3.58481702399811,2.50240278437361));
#52203=CARTESIAN_POINT('Ctrl Pts',(-86.0377374042336,-0.16727406989818,
4.36863275823537));
#52204=CARTESIAN_POINT('Ctrl Pts',(-85.8388638725364,-3.76567340491278,
2.22095398383672));
#52205=CARTESIAN_POINT('Ctrl Pts',(-85.6399903408387,-3.90416428353964,
-1.96734187113503));
#52206=CARTESIAN_POINT('Ctrl Pts',(-85.4411168091414,-0.455501002136817,
-4.34803997541882));
#52207=CARTESIAN_POINT('Ctrl Pts',(-85.2422432774438,3.41167753529698,-2.73375002257656));
#52208=CARTESIAN_POINT('Ctrl Pts',(-85.0433697457464,4.14419974819605,1.3923150641429));
#52209=CARTESIAN_POINT('Ctrl Pts',(-84.844496214049,1.06902272328098,4.23911821112559));
#52210=CARTESIAN_POINT('Ctrl Pts',(-84.6456226823515,-2.98837457477973,
3.19101084166095));
#52211=CARTESIAN_POINT('Ctrl Pts',(-84.4467491506541,-4.30004717758527,
-0.789003841136819));
#52212=CARTESIAN_POINT('Ctrl Pts',(-84.2478756189566,-1.66082760445654,
-4.04408017465809));
#52213=CARTESIAN_POINT('Ctrl Pts',(-84.0490020872592,2.50436378177857,-3.58344734010467));
#52214=CARTESIAN_POINT('Ctrl Pts',(-83.8501285555617,4.36854058317413,0.169664268331013));
#52215=CARTESIAN_POINT('Ctrl Pts',(-83.6512550238642,2.21889332694475,3.76688799865721));
#52216=CARTESIAN_POINT('Ctrl Pts',(-83.4523814921669,-1.96947767407428,
3.90308730136935));
#52217=CARTESIAN_POINT('Ctrl Pts',(-83.2535079604693,-4.34828854427934,
0.453121977481246));
#52218=CARTESIAN_POINT('Ctrl Pts',(-83.0546344287718,-2.73188297177902,
-3.41317274969951));
#52219=CARTESIAN_POINT('Ctrl Pts',(-82.8557608970745,1.39458228449222,-4.14343734628245));
#52220=CARTESIAN_POINT('Ctrl Pts',(-82.6568873653769,4.23970247431449,-1.06670320149481));
#52221=CARTESIAN_POINT('Ctrl Pts',(-82.4580138336795,3.18937532547179,2.99012003505869));
#52222=CARTESIAN_POINT('Ctrl Pts',(-82.2591403019821,-0.791356421071236,
4.29961484386878));
#52223=CARTESIAN_POINT('Ctrl Pts',(-82.0602667702846,-4.04498826306357,
1.65861470585109));
#52224=CARTESIAN_POINT('Ctrl Pts',(-81.8613932385872,-3.58207658348971,
-2.50632402949067));
#52225=CARTESIAN_POINT('Ctrl Pts',(-81.6625197068897,0.172054415974101,
-4.36844710037005));
#52226=CARTESIAN_POINT('Ctrl Pts',(-81.4636461751922,3.76810146476629,-2.21683200581681));
#52227=CARTESIAN_POINT('Ctrl Pts',(-81.2647726434949,3.90200915079183,1.97161288744128));
#52228=CARTESIAN_POINT('Ctrl Pts',(-81.0658991117974,0.450742817181481,
4.34853581145962));
#52229=CARTESIAN_POINT('Ctrl Pts',(-80.8670255800998,-3.41466694235303,
2.73001510317963));
#52230=CARTESIAN_POINT('Ctrl Pts',(-80.6681520484026,-4.14267370401169,
-1.39684908736692));
#52231=CARTESIAN_POINT('Ctrl Pts',(-80.4692785167048,-1.0643833603861,-4.24028546832885));
#52232=CARTESIAN_POINT('Ctrl Pts',(-80.2704049850077,2.99186460023139,-3.18773885452838));
#52233=CARTESIAN_POINT('Ctrl Pts',(-80.07153145331,4.29918122304274,0.793708764109494));
#52234=CARTESIAN_POINT('Ctrl Pts',(-79.8726579216127,1.65640131073161,4.04589514058312));
#52235=CARTESIAN_POINT('Ctrl Pts',(-79.6737843899151,-2.5082835269231,3.58070475456353));
#52236=CARTESIAN_POINT('Ctrl Pts',(-79.4749108582177,-4.36835230985113,
-0.174444512111902));
#52237=CARTESIAN_POINT('Ctrl Pts',(-79.2760373265202,-2.21477002106995,
-3.76931380287679));
#52238=CARTESIAN_POINT('Ctrl Pts',(-79.0771637948228,1.97374751059685,-3.90092983212983));
#52239=CARTESIAN_POINT('Ctrl Pts',(-78.8782902631254,4.3487817768856,-0.448363521949776));
#52240=CARTESIAN_POINT('Ctrl Pts',(-78.6794167314278,2.7281464173376,3.41616011281022));
#52241=CARTESIAN_POINT('Ctrl Pts',(-78.4805431997305,-1.39911547208838,
4.14190882161239));
#52242=CARTESIAN_POINT('Ctrl Pts',(-78.2816696680329,-4.24086719299416,
1.06206320064932));
#52243=CARTESIAN_POINT('Ctrl Pts',(-78.0827961363356,-3.18610142932061,
-2.9936082697756));
#52244=CARTESIAN_POINT('Ctrl Pts',(-77.883922604638,0.796060869547362,-4.29874631523692));
#52245=CARTESIAN_POINT('Ctrl Pts',(-77.6850490729406,4.04680080694526,-1.65418741976074));
#52246=CARTESIAN_POINT('Ctrl Pts',(-77.4861755412432,3.57933185373683,2.51024227348926));
#52247=CARTESIAN_POINT('Ctrl Pts',(-77.2873020095457,-0.176834556028938,
4.36825621164575));
#52248=CARTESIAN_POINT('Ctrl Pts',(-77.0884284778483,-3.77052501262576,
2.21270737332146));
#52249=CARTESIAN_POINT('Ctrl Pts',(-76.8895549461508,-3.89984934570645,
-1.97588154290197));
#52250=CARTESIAN_POINT('Ctrl Pts',(-76.6906814144534,-0.445984092498367,
-4.34902644048364));
#52251=CARTESIAN_POINT('Ctrl Pts',(-76.4918078827558,3.41765226062408,-2.72627691481233));
#52252=CARTESIAN_POINT('Ctrl Pts',(-76.2929343510585,4.14114269931356,1.40138143797816));
#52253=CARTESIAN_POINT('Ctrl Pts',(-76.094060819361,1.05974272297901,4.24144764813627));
#52254=CARTESIAN_POINT('Ctrl Pts',(-75.8951872876635,-2.99535104316932,
3.18446305033865));
#52255=CARTESIAN_POINT('Ctrl Pts',(-75.6963137559662,-4.29831012058151,
-0.79841273668073));
#52256=CARTESIAN_POINT('Ctrl Pts',(-75.4974402242686,-1.65197303360122,
-4.04770526187887));
#52257=CARTESIAN_POINT('Ctrl Pts',(-75.2985666925712,2.5122002686028,-3.57795788142059));
#52258=CARTESIAN_POINT('Ctrl Pts',(-75.0996931608737,4.36815880578268,0.179224547009723));
#52259=CARTESIAN_POINT('Ctrl Pts',(-74.9008196291763,2.21064406318877,3.77173509365066));
#52260=CARTESIAN_POINT('Ctrl Pts',(-74.7019460974789,-1.97801498371782,
3.89876769184514));
#52261=CARTESIAN_POINT('Ctrl Pts',(-74.5030725657813,-4.34926980218053,
0.443604529539567));
#52262=CARTESIAN_POINT('Ctrl Pts',(-74.3041990340839,-2.72440659616345,
-3.41914338534794));
#52263=CARTESIAN_POINT('Ctrl Pts',(-74.1053255023865,1.40364698435792,-4.1403753373445));
#52264=CARTESIAN_POINT('Ctrl Pts',(-73.9064519706889,4.24202683358142,-1.05742192806981));
#52265=CARTESIAN_POINT('Ctrl Pts',(-73.7075784389916,3.18282371807295,2.99709291989086));
#52266=CARTESIAN_POINT('Ctrl Pts',(-73.508704907294,-0.800764364805553,
4.29787263920711));
#52267=CARTESIAN_POINT('Ctrl Pts',(-73.3098313755967,-4.04860850511319,
1.64975815291593));
#52268=CARTESIAN_POINT('Ctrl Pts',(-73.1109578438992,-3.57658283802612,
-2.51415751167756));
#52269=CARTESIAN_POINT('Ctrl Pts',(-72.9120843122017,0.181614484338818,
-4.36806009229109));
#52270=CARTESIAN_POINT('Ctrl Pts',(-72.7132107805044,3.7729440455892,-2.20858009128957));
#52271=CARTESIAN_POINT('Ctrl Pts',(-72.5143372488068,3.8976848708697,1.98014783240569));
#52272=CARTESIAN_POINT('Ctrl Pts',(-72.3154637171094,0.441224833785749,
4.34951186190338));
#52273=CARTESIAN_POINT('Ctrl Pts',(-72.1165901854119,-3.42063348653541,
2.72253546195091));
#52274=CARTESIAN_POINT('Ctrl Pts',(-71.9177166537145,-4.13960673593495,
-1.40591211054947));
#52275=CARTESIAN_POINT('Ctrl Pts',(-71.718843122017,-1.05510081661648,-4.24260474915622));
#52276=CARTESIAN_POINT('Ctrl Pts',(-71.5199695903195,2.99883389941879,-3.18118343301426));
#52277=CARTESIAN_POINT('Ctrl Pts',(-71.3210960586221,4.29743387124465,0.803115753217863));
#52278=CARTESIAN_POINT('Ctrl Pts',(-71.1222225269246,1.64754277836791,4.04951053637785));
#52279=CARTESIAN_POINT('Ctrl Pts',(-70.9233489952272,-2.51611400212766,
3.57520672396504));
#52280=CARTESIAN_POINT('Ctrl Pts',(-70.7244754635297,-4.36796007120051,
-0.184004367300773));
#52281=CARTESIAN_POINT('Ctrl Pts',(-70.5256019318323,-2.20651545824171,
-3.77415186807951));
#52282=CARTESIAN_POINT('Ctrl Pts',(-70.3267284001348,1.9822800883272,-3.89660088310427));
#52283=CARTESIAN_POINT('Ctrl Pts',(-70.1278548684374,4.34975261957975,-0.438845005949189));
#52284=CARTESIAN_POINT('Ctrl Pts',(-69.92898133674,2.72066351273476,3.42212256374044));
#52285=CARTESIAN_POINT('Ctrl Pts',(-69.7301078050424,-1.40817681587473,
4.13883689531498));
#52286=CARTESIAN_POINT('Ctrl Pts',(-69.5312342733451,-4.24318139468768,
1.05277938931384));
#52287=CARTESIAN_POINT('Ctrl Pts',(-69.3323607416474,-3.1795421956536,-3.00057398123192));
#52288=CARTESIAN_POINT('Ctrl Pts',(-69.1334872099503,0.805466901213757,
-4.2969938168255));
#52289=CARTESIAN_POINT('Ctrl Pts',(-68.9346136782525,4.0504113554028,-1.64532691062035));
#52290=CARTESIAN_POINT('Ctrl Pts',(-68.7357401465554,3.5738295396493,2.5180697393674));
#52291=CARTESIAN_POINT('Ctrl Pts',(-68.5368666148576,-0.186394195180171,
4.36785874254088));
#52292=CARTESIAN_POINT('Ctrl Pts',(-68.3379930831604,-3.77535856076001,
2.20445016466324));
#52293=CARTESIAN_POINT('Ctrl Pts',(-68.1391195514628,-3.89551572887335,
-1.98441175084401));
#52294=CARTESIAN_POINT('Ctrl Pts',(-67.9402460197655,-0.436465046742345,
-4.34999207513758));
#52295=CARTESIAN_POINT('Ctrl Pts',(-67.7413724880679,3.42361061651726,-2.7187907490754));
#52296=CARTESIAN_POINT('Ctrl Pts',(-67.5424989563705,4.13806581571506,1.41044109965575));
#52297=CARTESIAN_POINT('Ctrl Pts',(-67.343625424673,1.05045764685681,4.24375677000317));
#52298=CARTESIAN_POINT('Ctrl Pts',(-67.1447518929755,-3.00231316480936,
3.17790000648228));
#52299=CARTESIAN_POINT('Ctrl Pts',(-66.9458783612782,-4.29655247608139,
-0.807817808089409));
#52300=CARTESIAN_POINT('Ctrl Pts',(-66.7470048295806,-1.64311055033657,
-4.0513109619184));
#52301=CARTESIAN_POINT('Ctrl Pts',(-66.5481312978833,2.52002472281131,-3.57245128549116));
#52302=CARTESIAN_POINT('Ctrl Pts',(-66.3492577661856,4.36775610634255,0.188783967261603));
#52303=CARTESIAN_POINT('Ctrl Pts',(-66.1503842344884,2.20238421117243,3.77656412326947));
#52304=CARTESIAN_POINT('Ctrl Pts',(-65.9515107027907,-1.98654281931798,
3.89442940850179));
#52305=CARTESIAN_POINT('Ctrl Pts',(-65.7526371710935,-4.35023022850515,
0.434084956877671));
#52306=CARTESIAN_POINT('Ctrl Pts',(-65.5537636393959,-2.71691717153346,
-3.42509764442042));
#52307=CARTESIAN_POINT('Ctrl Pts',(-65.3548901076986,1.41270496121471,-4.137293497366));
#52308=CARTESIAN_POINT('Ctrl Pts',(-65.156016576001,4.24433087493045,-1.04813558994043));
#52309=CARTESIAN_POINT('Ctrl Pts',(-64.9571430443036,3.17625686599191,3.00405144963047));
#52310=CARTESIAN_POINT('Ctrl Pts',(-64.7582695126061,-0.810168473141068,
4.29610984914443));
#52311=CARTESIAN_POINT('Ctrl Pts',(-64.5593959809086,-4.05220935565532,
1.64089369818005));
#52312=CARTESIAN_POINT('Ctrl Pts',(-64.3605224492113,-3.57107196190321,
-2.52197895187418));
#52313=CARTESIAN_POINT('Ctrl Pts',(-64.1616489175137,0.191173682829687,
-4.36765216263623));
#52314=CARTESIAN_POINT('Ctrl Pts',(-63.9627753858163,3.777768555247,-2.20031759838772));
#52315=CARTESIAN_POINT('Ctrl Pts',(-63.7639018541189,3.89334192231479,1.98867329311118));
#52316=CARTESIAN_POINT('Ctrl Pts',(-63.5650283224214,0.431704737067659,
4.3504670796112));
#52317=CARTESIAN_POINT('Ctrl Pts',(-63.3661547907239,-3.42658364700476,
2.71504278066981));
#52318=CARTESIAN_POINT('Ctrl Pts',(-63.1672812590265,-4.13651994049901,
-1.4149683998739));
#52319=CARTESIAN_POINT('Ctrl Pts',(-62.968407727329,-1.04581321925983,-4.24490370929767));
#52320=CARTESIAN_POINT('Ctrl Pts',(-62.7695341956316,3.00578883517485,-3.17461277467437));
#52321=CARTESIAN_POINT('Ctrl Pts',(-62.5706606639341,4.29566593614713,0.812518895664999));
#52322=CARTESIAN_POINT('Ctrl Pts',(-62.3717871322366,1.63867635481445,4.05310653634465));
#52323=CARTESIAN_POINT('Ctrl Pts',(-62.1729136005392,-2.52393242597099,
3.56969156929837));
#52324=CARTESIAN_POINT('Ctrl Pts',(-61.9740400688417,-4.36754691145306,
-0.193563341169043));
#52325=CARTESIAN_POINT('Ctrl Pts',(-61.7751665371444,-2.19825032692777,
-3.77897185633205));
#52326=CARTESIAN_POINT('Ctrl Pts',(-61.5762930054469,1.99080317158582,-3.89225327063788));
#52327=CARTESIAN_POINT('Ctrl Pts',(-61.3774194737493,4.35070262838482,-0.429324388024834));
#52328=CARTESIAN_POINT('Ctrl Pts',(-61.178545942052,2.71316757704555,3.42806862382544));
#52329=CARTESIAN_POINT('Ctrl Pts',(-60.9796724103545,-1.41723141495577,
4.13574514534565));
#52330=CARTESIAN_POINT('Ctrl Pts',(-60.780798878657,-4.24547527293333,1.0434905355102));
#52331=CARTESIAN_POINT('Ctrl Pts',(-60.5819253469596,-3.1729677330218,-3.00752532092253));
#52332=CARTESIAN_POINT('Ctrl Pts',(-60.3830518152621,0.814869074957788,
-4.29522073722237));
#52333=CARTESIAN_POINT('Ctrl Pts',(-60.1841782835647,4.05400250371783,-1.63645852090336));
#52334=CARTESIAN_POINT('Ctrl Pts',(-59.9853047518672,3.56831010808978,2.52588514451706));
#52335=CARTESIAN_POINT('Ctrl Pts',(-59.7864312201697,-0.195952941564444,
4.36744035282451));
#52336=CARTESIAN_POINT('Ctrl Pts',(-59.5875576884724,-3.78017402616446,
2.1961823974113));
#52337=CARTESIAN_POINT('Ctrl Pts',(-59.3886841567748,-3.8911634537969,-1.99293245410441));
#52338=CARTESIAN_POINT('Ctrl Pts',(-59.1898106250775,-0.426943910461734,
-4.35093687475548));
#52339=CARTESIAN_POINT('Ctrl Pts',(-58.9909370933799,3.42955257443794,-2.71129156122203));
#52340=CARTESIAN_POINT('Ctrl Pts',(-58.7920635616825,4.13496911213787,1.41949400578286));
#52341=CARTESIAN_POINT('Ctrl Pts',(-58.5931900299851,1.04116753938684,4.24604556566634));
#52342=CARTESIAN_POINT('Ctrl Pts',(-58.3943164982875,-3.00926090635356,
3.17132174152668));
#52343=CARTESIAN_POINT('Ctrl Pts',(-58.1954429665903,-4.29477425250343,
-0.81721901031565));
#52344=CARTESIAN_POINT('Ctrl Pts',(-57.9965694348925,-1.63424019711096,
-4.05489725750658));
#52345=CARTESIAN_POINT('Ctrl Pts',(-57.7976959031953,2.52783710692763,-3.56692757869113));
#52346=CARTESIAN_POINT('Ctrl Pts',(-57.5988223714977,4.36733248678251,0.198342483300303));
#52347=CARTESIAN_POINT('Ctrl Pts',(-57.3999488398004,2.1941138104576,3.78137506438423));
#52348=CARTESIAN_POINT('Ctrl Pts',(-57.2010753081028,-1.99506114002947,
3.89007247211823));
#52349=CARTESIAN_POINT('Ctrl Pts',(-57.0022017764055,-4.35116981865314,
0.424563305090861));
#52350=CARTESIAN_POINT('Ctrl Pts',(-56.8033282447079,-2.70941473376068,
-3.43103549839809));
#52351=CARTESIAN_POINT('Ctrl Pts',(-56.6044547130105,1.42175617167791,-4.1341918411079));
#52352=CARTESIAN_POINT('Ctrl Pts',(-56.4055811813131,4.24661458732599,-1.03884423158519));
#52353=CARTESIAN_POINT('Ctrl Pts',(-56.2067076496156,3.16967480068174,3.01099559094843));
#52354=CARTESIAN_POINT('Ctrl Pts',(-56.0078341179182,-0.819568701035232,
4.29432648212395));
#52355=CARTESIAN_POINT('Ctrl Pts',(-55.8089605862207,-4.05579079744309,
1.6320213841012));
#52356=CARTESIAN_POINT('Ctrl Pts',(-55.6100870545232,-3.56554398151623,
-2.52978831261849));
#52357=CARTESIAN_POINT('Ctrl Pts',(-55.4112135228258,0.200731965661421,
-4.36722331335934));
#52358=CARTESIAN_POINT('Ctrl Pts',(-55.2123399911283,3.78257497063191,-2.19204456668579));
#52359=CARTESIAN_POINT('Ctrl Pts',(-55.0134664594309,3.88898032592836,1.99718922872367));
#52360=CARTESIAN_POINT('Ctrl Pts',(-54.8145929277334,0.422182572625175,
4.35140146000794));
#52361=CARTESIAN_POINT('Ctrl Pts',(-54.6157193960359,-3.43251739526182,
2.70753709522368));
#52362=CARTESIAN_POINT('Ctrl Pts',(-54.4168458643385,-4.13341333248855,
-1.42401791196362));
#52363=CARTESIAN_POINT('Ctrl Pts',(-54.2179723326411,-1.0365206128007,-4.24718233774192));
#52364=CARTESIAN_POINT('Ctrl Pts',(-54.0190988009436,3.01272937418784,-3.16802691097999));
#52365=CARTESIAN_POINT('Ctrl Pts',(-53.8202252692461,4.293877426218,0.821918146413134));
#52366=CARTESIAN_POINT('Ctrl Pts',(-53.6213517375487,1.62980208253829,4.05668312325988));
#52367=CARTESIAN_POINT('Ctrl Pts',(-53.4224782058512,-2.53173876100551,
3.56415931697925));
#52368=CARTESIAN_POINT('Ctrl Pts',(-53.2236046741539,-4.36711283258768,
-0.203121387932494));
#52369=CARTESIAN_POINT('Ctrl Pts',(-53.0247311424563,-2.18997466671529,
-3.78377374454828));
#52370=CARTESIAN_POINT('Ctrl Pts',(-52.825857610759,1.99931671955004,-3.88788701555426));
#52371=CARTESIAN_POINT('Ctrl Pts',(-52.6269840790614,4.3516317987506,-0.419801713777189));
#52372=CARTESIAN_POINT('Ctrl Pts',(-52.4281105473641,2.70565864617292,3.43399826458561));
#52373=CARTESIAN_POINT('Ctrl Pts',(-52.2292370156665,-1.42627922596299,
4.13263358651281));
#52374=CARTESIAN_POINT('Ctrl Pts',(-52.0303634839691,-4.24774881674419,
1.03419668372898));
#52375=CARTESIAN_POINT('Ctrl Pts',(-51.8314899522716,-3.16637807291474,
-3.0144622555528));
#52376=CARTESIAN_POINT('Ctrl Pts',(-51.6326164205741,0.824267345746038,
-4.29342708491998));
#52377=CARTESIAN_POINT('Ctrl Pts',(-51.4337428888768,4.05757423468981,-1.6275822930866));
#52378=CARTESIAN_POINT('Ctrl Pts',(-51.2348693571792,3.5627735854947,2.53368845150483));
#52379=CARTESIAN_POINT('Ctrl Pts',(-51.0359958254819,-0.205510749398244,
4.36700104450061));
#52380=CARTESIAN_POINT('Ctrl Pts',(-50.8371222937843,-3.78497138577449,
2.18790411116576));
#52381=CARTESIAN_POINT('Ctrl Pts',(-50.6382487620869,-3.8867925413232,-2.00144361187171));
#52382=CARTESIAN_POINT('Ctrl Pts',(-50.4393752303894,-0.417420729259616,
-4.35186083481216));
#52383=CARTESIAN_POINT('Ctrl Pts',(-50.240501698692,3.43547810592614,-2.70377938717074));
#52384=CARTESIAN_POINT('Ctrl Pts',(-50.0416281669945,4.1318526034141,1.42854011299908));
#52385=CARTESIAN_POINT('Ctrl Pts',(-49.8427546352971,1.03187244506569,4.24831402416321));
#52386=CARTESIAN_POINT('Ctrl Pts',(-49.6438811035996,-3.01619423452454,
3.16472828697957));
#52387=CARTESIAN_POINT('Ctrl Pts',(-49.4450075719022,-4.29297545836471,
-0.826616298330698));
#52388=CARTESIAN_POINT('Ctrl Pts',(-49.2461340402047,-1.62536201641063,
-4.05846413146615));
#52389=CARTESIAN_POINT('Ctrl Pts',(-49.0472605085073,2.5356373835328,-3.5613867874774));
#52390=CARTESIAN_POINT('Ctrl Pts',(-48.8483869768098,4.36688794913159,0.207900049343396));
#52391=CARTESIAN_POINT('Ctrl Pts',(-48.6495134451124,2.18583290065701,3.78616789395201));
#52392=CARTESIAN_POINT('Ctrl Pts',(-48.4506399134149,-2.00356990505197,
3.88569690356282));
#52393=CARTESIAN_POINT('Ctrl Pts',(-48.2517663817174,-4.35208856812407,
0.415039619785222));
#52394=CARTESIAN_POINT('Ctrl Pts',(-48.05289285002,-2.7018993187797,-3.43695691884043));
#52395=CARTESIAN_POINT('Ctrl Pts',(-47.8540193183225,1.43080057239508,-4.13107038342622));
#52396=CARTESIAN_POINT('Ctrl Pts',(-47.655145786625,4.24887795982979,-1.02954789750662));
#52397=CARTESIAN_POINT('Ctrl Pts',(-47.4562722549277,3.16307755366836,3.01792531058458));
#52398=CARTESIAN_POINT('Ctrl Pts',(-47.2573987232301,-0.828965003463952,
4.2925225466874));
#52399=CARTESIAN_POINT('Ctrl Pts',(-47.0585251915328,-4.05935281332248,
1.62314125317501));
#52400=CARTESIAN_POINT('Ctrl Pts',(-46.8596516598352,-3.55999892334251,
-2.53758555650599));
#52401=CARTESIAN_POINT('Ctrl Pts',(-46.6607781281379,0.210289287052714,
-4.36677354651447));
#52402=CARTESIAN_POINT('Ctrl Pts',(-46.4619045964403,3.78736326872267,-2.18376103580909));
#52403=CARTESIAN_POINT('Ctrl Pts',(-46.2630310647429,3.88460010260112,2.00569559845433));
#52404=CARTESIAN_POINT('Ctrl Pts',(-46.0641575330454,0.412658386066791,
4.35231499861814));
#52405=CARTESIAN_POINT('Ctrl Pts',(-45.865284001348,-3.43843470288575,2.70001844156262));
#52406=CARTESIAN_POINT('Ctrl Pts',(-45.6664104696505,-4.13028692678332,
-1.43306060347432));
#52407=CARTESIAN_POINT('Ctrl Pts',(-45.4675369379531,-1.02722304174763,
-4.24944062357511));
#52408=CARTESIAN_POINT('Ctrl Pts',(-45.2686634062556,3.01965548321474,-3.16142587347527));
#52409=CARTESIAN_POINT('Ctrl Pts',(-45.0697898745582,4.29206835002362,0.831313460442701));
#52410=CARTESIAN_POINT('Ctrl Pts',(-44.8709163428607,1.62092000404456,4.06024027999278));
#52411=CARTESIAN_POINT('Ctrl Pts',(-44.6720428111633,-2.53953296984122,
3.55860999350548));
#52412=CARTESIAN_POINT('Ctrl Pts',(-44.4731692794658,-4.3666578366835,-0.212678461810957));
#52413=CARTESIAN_POINT('Ctrl Pts',(-44.2742957477684,-2.18168851724219,
-3.78855750972863));
#52414=CARTESIAN_POINT('Ctrl Pts',(-44.0754222160709,2.00782069144243,-3.88350213876641));
#52415=CARTESIAN_POINT('Ctrl Pts',(-43.8765486843735,4.3525401262266,-0.410277028817174));
#52416=CARTESIAN_POINT('Ctrl Pts',(-43.677675152676,2.69813675608252,3.43991145761977));
#52417=CARTESIAN_POINT('Ctrl Pts',(-43.4788016209786,-1.43532020556023,
4.12950223371992));
#52418=CARTESIAN_POINT('Ctrl Pts',(-43.2799280892811,-4.25000201523073,
1.02489787848468));
#52419=CARTESIAN_POINT('Ctrl Pts',(-43.0810545575836,-3.15977324689472,
-3.02138475189707));
#52420=CARTESIAN_POINT('Ctrl Pts',(-42.8821810258862,0.83366166856392,-4.29161286850933));
#52421=CARTESIAN_POINT('Ctrl Pts',(-42.6833074941888,4.06112653121138,-1.61869826968422));
#52422=CARTESIAN_POINT('Ctrl Pts',(-42.4844339624912,3.55721999838211,2.54147962295552));
#52423=CARTESIAN_POINT('Ctrl Pts',(-42.2855604307939,-0.215067572902925,
4.36654081967332));
#52424=CARTESIAN_POINT('Ctrl Pts',(-42.0866868990963,-3.78975061661238,
2.17961534557676));
#52425=CARTESIAN_POINT('Ctrl Pts',(-41.887813367399,-3.88240301238739,-2.00994518338014));
#52426=CARTESIAN_POINT('Ctrl Pts',(-41.6889398357014,-0.407895548749227,
-4.35276395088204));
#52427=CARTESIAN_POINT('Ctrl Pts',(-41.4900663040041,3.44138718260039,-2.69625426290272));
#52428=CARTESIAN_POINT('Ctrl Pts',(-41.2911927723065,4.12871630447095,1.43757937797641));
#52429=CARTESIAN_POINT('Ctrl Pts',(-41.0923192406092,1.0225724084138,4.25056213462861));
#52430=CARTESIAN_POINT('Ctrl Pts',(-40.8934457089116,-3.02311311611391,
3.15811967442143));
#52431=CARTESIAN_POINT('Ctrl Pts',(-40.6945721772142,-4.29115610228089,
-0.83600962712466));
#52432=CARTESIAN_POINT('Ctrl Pts',(-40.4956986455168,-1.61647605075906,
-4.06201156671298));
#52433=CARTESIAN_POINT('Ctrl Pts',(-40.2968251138193,2.54342551526614,-3.55582893838847));
#52434=CARTESIAN_POINT('Ctrl Pts',(-40.0979515821218,4.36642249551896,0.217456619613414));
#52435=CARTESIAN_POINT('Ctrl Pts',(-39.8990780504244,2.1775415214334,3.79094258901677));
#52436=CARTESIAN_POINT('Ctrl Pts',(-39.7002045187269,-2.01206907363145,
3.88130272379308));
#52437=CARTESIAN_POINT('Ctrl Pts',(-39.5013309870295,-4.35298647251748,
0.40551394657586));
#52438=CARTESIAN_POINT('Ctrl Pts',(-39.302457455332,-2.69437096258673,-3.44286187738583));
#52439=CARTESIAN_POINT('Ctrl Pts',(-39.1035839236346,1.43983812004655,-4.12792913927167));
#52440=CARTESIAN_POINT('Ctrl Pts',(-38.9047103919372,4.25112098160105,-1.02024663223114));
#52441=CARTESIAN_POINT('Ctrl Pts',(-38.7058368602396,3.15646515655044,3.02484057534785));
#52442=CARTESIAN_POINT('Ctrl Pts',(-38.5069633285422,-0.83835733542206,
4.29069805147503));
#52443=CARTESIAN_POINT('Ctrl Pts',(-38.3080897968448,-4.06289538623264,
1.61425334793433));
#52444=CARTESIAN_POINT('Ctrl Pts',(-38.1092162651473,-3.55443681394101,
-2.54537064619057));
#52445=CARTESIAN_POINT('Ctrl Pts',(-37.9103427334499,0.219845601227261,
-4.36630286425583));
#52446=CARTESIAN_POINT('Ctrl Pts',(-37.7114692017524,3.79213342658497,-2.17546704543292));
#52447=CARTESIAN_POINT('Ctrl Pts',(-37.5125956700549,3.88020127331285,2.01419236156059));
#52448=CARTESIAN_POINT('Ctrl Pts',(-37.3137221383575,0.403132223010095,
4.35320769106624));
#52449=CARTESIAN_POINT('Ctrl Pts',(-37.11484860666,-3.44433554153461,2.69248685569843));
#52450=CARTESIAN_POINT('Ctrl Pts',(-36.9159750749626,-4.12714073835777,
-1.44209643109444));
#52451=CARTESIAN_POINT('Ctrl Pts',(-36.7171015432651,-1.01792055063294,
-4.25167855598078));
#52452=CARTESIAN_POINT('Ctrl Pts',(-36.5182280115677,3.02656712908178,-3.15480969377699));
#52453=CARTESIAN_POINT('Ctrl Pts',(-36.3193544798703,4.29023871622889,0.840704792753313));
#52454=CARTESIAN_POINT('Ctrl Pts',(-36.1204809481727,1.61203016187539,4.06377798950578));
#52455=CARTESIAN_POINT('Ctrl Pts',(-35.9216074164753,-2.54731501514653,
3.55304362545645));
#52456=CARTESIAN_POINT('Ctrl Pts',(-35.7227338847778,-4.36618192591977,
-0.222234517029311));
#52457=CARTESIAN_POINT('Ctrl Pts',(-35.5238603530804,-2.17339191819631,
-3.79332312896049));
#52458=CARTESIAN_POINT('Ctrl Pts',(-35.3249868213829,2.01631504653193,-3.87909866127643));
#52459=CARTESIAN_POINT('Ctrl Pts',(-35.1261132896855,4.3534276064622,-0.400750378764763));
#52460=CARTESIAN_POINT('Ctrl Pts',(-34.9272397579881,2.69060194280166,3.44580817460567));
#52461=CARTESIAN_POINT('Ctrl Pts',(-34.7283662262906,-1.44435431044416,
4.12635110196515));
#52462=CARTESIAN_POINT('Ctrl Pts',(-34.5294926945932,-4.25223485760088,
1.01559416431552));
#52463=CARTESIAN_POINT('Ctrl Pts',(-34.3306191628957,-3.15315328659669,
-3.02829277679886));
#52464=CARTESIAN_POINT('Ctrl Pts',(-34.1317456311983,0.843051998415699,
-4.28977809667994));
#52465=CARTESIAN_POINT('Ctrl Pts',(-33.9328720995008,4.0646593762682,-1.60980649324777));
#52466=CARTESIAN_POINT('Ctrl Pts',(-33.7339985678033,3.55164937335186,2.54925862155197));
#52467=CARTESIAN_POINT('Ctrl Pts',(-33.5351250361059,-0.224623366304428,
4.36605968054695));
#52468=CARTESIAN_POINT('Ctrl Pts',(-33.3362515044084,-3.7945116957872,2.17131614034479));
#52469=CARTESIAN_POINT('Ctrl Pts',(-33.1373779727109,-3.8779948880139,-2.01843712791005));
#52470=CARTESIAN_POINT('Ctrl Pts',(-32.9385044410135,-0.398368414552949,
-4.35364621863948));
#52471=CARTESIAN_POINT('Ctrl Pts',(-32.7396309093161,3.44727977615813,-2.68871622446075));
#52472=CARTESIAN_POINT('Ctrl Pts',(-32.5407573776186,4.12556023033026,1.44661175741973));
#52473=CARTESIAN_POINT('Ctrl Pts',(-32.3418838459212,1.01326747397528,4.25278988629482));
#52474=CARTESIAN_POINT('Ctrl Pts',(-32.1430103142237,-3.03001751798249,
3.15149593550537));
#52475=CARTESIAN_POINT('Ctrl Pts',(-31.9441367825262,-4.28931619296609,
-0.845398951706575));
#52476=CARTESIAN_POINT('Ctrl Pts',(-31.7452632508288,-1.60758234271713,
-4.06553954625603));
#52477=CARTESIAN_POINT('Ctrl Pts',(-31.5463897191313,2.55120146482505,-3.55025405804461));
#52478=CARTESIAN_POINT('Ctrl Pts',(-31.3475161874339,4.36593612817399,0.227012148337509));
#52479=CARTESIAN_POINT('Ctrl Pts',(-31.1486426557364,2.16923971249975,3.79569912670929));
#52480=CARTESIAN_POINT('Ctrl Pts',(-30.949769124039,-2.02055860505967,3.87688995385567));
#52481=CARTESIAN_POINT('Ctrl Pts',(-30.7508955923414,-4.35386352753264,
0.395986331087709));
#52482=CARTESIAN_POINT('Ctrl Pts',(-30.5520220606441,-2.68682970124021,
-3.44875034575145));
#52483=CARTESIAN_POINT('Ctrl Pts',(-30.3531485289466,1.44886877134539,-4.12476812368983));
#52484=CARTESIAN_POINT('Ctrl Pts',(-30.1542749972492,4.25334364189643,-1.01094048030875));
#52485=CARTESIAN_POINT('Ctrl Pts',(-29.9554014655517,3.14983764099918,3.03174135211637));
#52486=CARTESIAN_POINT('Ctrl Pts',(-29.7565279338542,-0.847745651923367,
4.28885300522561));
#52487=CARTESIAN_POINT('Ctrl Pts',(-29.5576544021568,-4.06641849920581,
1.60535771094929));
#52488=CARTESIAN_POINT('Ctrl Pts',(-29.3587808704593,-3.54885767995239,
-2.55314354438418));
#52489=CARTESIAN_POINT('Ctrl Pts',(-29.1599073387619,0.229400862413447,
-4.36581126883786));
#52490=CARTESIAN_POINT('Ctrl Pts',(-28.9610338070644,3.7968854213713,-2.16716263528277));
#52491=CARTESIAN_POINT('Ctrl Pts',(-28.762160275367,3.8757838591325,2.02267947734574));
#52492=CARTESIAN_POINT('Ctrl Pts',(-28.5632867436695,0.393604129082132,
4.35407953307663));
#52493=CARTESIAN_POINT('Ctrl Pts',(-28.3644132119721,-3.45021988294541,
2.68494237370479));
#52494=CARTESIAN_POINT('Ctrl Pts',(-28.1655396802746,-4.123974782281,-1.45112535154548));
#52495=CARTESIAN_POINT('Ctrl Pts',(-27.9666661485772,-1.00861318401251,
-4.25389612423997));
#52496=CARTESIAN_POINT('Ctrl Pts',(-27.7677926168797,3.03346427868447,-3.14817840357452));
#52497=CARTESIAN_POINT('Ctrl Pts',(-27.5689190851823,4.28838853359714,0.850092098363576));
#52498=CARTESIAN_POINT('Ctrl Pts',(-27.3700455534848,1.60313259861021,4.06729623485442));
#52499=CARTESIAN_POINT('Ctrl Pts',(-27.1711720217873,-2.55508485964799,
3.54746023949322));
#52500=CARTESIAN_POINT('Ctrl Pts',(-26.9722984900899,-4.36568510257594,
-0.231789507817176));
#52501=CARTESIAN_POINT('Ctrl Pts',(-26.7734249583924,-2.16508490931564,
-3.79807057941811));
#52502=CARTESIAN_POINT('Ctrl Pts',(-26.574551426695,2.02479974413336,-3.87467660417552));
#52503=CARTESIAN_POINT('Ctrl Pts',(-26.3756778949975,4.35429423520678,-0.391221809249338));
#52504=CARTESIAN_POINT('Ctrl Pts',(-26.1768043633001,2.68305424241945,3.45168838730009));
#52505=CARTESIAN_POINT('Ctrl Pts',(-25.9779308316026,-1.45338149734449,
4.12318020634126));
#52506=CARTESIAN_POINT('Ctrl Pts',(-25.7790572999052,-4.25444733316004,
1.00628558578325));
#52507=CARTESIAN_POINT('Ctrl Pts',(-25.5801837682078,-3.1465182237281,-3.035186297171));
#52508=CARTESIAN_POINT('Ctrl Pts',(-25.3813102365102,0.852438290324783,
-4.28792277821976));
#52509=CARTESIAN_POINT('Ctrl Pts',(-25.1824367048128,4.06817275293909,-1.60090700636595));
#52510=CARTESIAN_POINT('Ctrl Pts',(-24.9835631731153,3.54606173708543,2.55702541003533));
#52511=CARTESIAN_POINT('Ctrl Pts',(-24.7846896414179,-0.23417808383365,
4.36555762942601));
#52512=CARTESIAN_POINT('Ctrl Pts',(-24.5858161097204,-3.79925460049492,
2.16300653522032));
#52513=CARTESIAN_POINT('Ctrl Pts',(-24.386942578023,-3.87356818931619,-2.0269194047878));
#52514=CARTESIAN_POINT('Ctrl Pts',(-24.1880690463255,-0.388839372302486,
-4.35450763385882));
#52515=CARTESIAN_POINT('Ctrl Pts',(-23.9891955146281,3.4531558583759,-2.68116530794941));
#52516=CARTESIAN_POINT('Ctrl Pts',(-23.7903219829307,4.12238439610845,1.45563720806703));
#52517=CARTESIAN_POINT('Ctrl Pts',(-23.5914484512331,1.00395768631775,4.25499726849163));
#52518=CARTESIAN_POINT('Ctrl Pts',(-23.3925749195357,-3.03690740706049,
3.14485710195691));
#52519=CARTESIAN_POINT('Ctrl Pts',(-23.1937013878383,-4.28745573923285,
-0.854784227104649));
#52520=CARTESIAN_POINT('Ctrl Pts',(-22.9948278561408,-1.5986809348828,-4.06904805319745));
#52521=CARTESIAN_POINT('Ctrl Pts',(-22.7959543244434,2.5589651949653,-3.54466217314766));
#52522=CARTESIAN_POINT('Ctrl Pts',(-22.5970807927458,4.36542884942622,0.23656658974783));
#52523=CARTESIAN_POINT('Ctrl Pts',(-22.3982072610485,2.16092751361901,3.80043748424731));
#52524=CARTESIAN_POINT('Ctrl Pts',(-22.199333729351,-2.02903845867456,3.87245861488632));
#52525=CARTESIAN_POINT('Ctrl Pts',(-22.0004601976535,-4.35471972896887,
0.386456818954767));
#52526=CARTESIAN_POINT('Ctrl Pts',(-21.8015866659561,-2.67927557086015,
-3.45462229573354));
#52527=CARTESIAN_POINT('Ctrl Pts',(-21.6027131342586,1.45789248303785,-4.12158735182083));
#52528=CARTESIAN_POINT('Ctrl Pts',(-21.4038396025612,4.25554593007011,-1.00162948631287));
#52529=CARTESIAN_POINT('Ctrl Pts',(-21.2049660708637,3.14319503875821,3.0386276078377));
#52530=CARTESIAN_POINT('Ctrl Pts',(-21.0060925391664,-0.857129908000908,
4.28698741677627));
#52531=CARTESIAN_POINT('Ctrl Pts',(-20.8072190074687,-4.06992213536745,
1.5964543848271));
#52532=CARTESIAN_POINT('Ctrl Pts',(-20.6083454757714,-3.54326154809888,
-2.5609042138572));
#52533=CARTESIAN_POINT('Ctrl Pts',(-20.4094719440739,0.238955024844702,
-4.36529876261513));
#52534=CARTESIAN_POINT('Ctrl Pts',(-20.2105984123765,3.80161923032118,-2.15884784513404));
#52535=CARTESIAN_POINT('Ctrl Pts',(-20.011724880679,3.87134788121805,2.03115690515927));
#52536=CARTESIAN_POINT('Ctrl Pts',(-19.8128513489816,0.384074149919422,
4.35493052047343));
#52537=CARTESIAN_POINT('Ctrl Pts',(-19.6139778172841,-3.45608769893403,
2.67738503171736));
#52538=CARTESIAN_POINT('Ctrl Pts',(-19.4151042855866,-4.12078907371697,
-1.4601473215818));
#52539=CARTESIAN_POINT('Ctrl Pts',(-19.2162307538892,-0.999300986465579,
-4.25609331773125));
#52540=CARTESIAN_POINT('Ctrl Pts',(-19.0173572221917,3.04034689898769,-3.14153203462953));
#52541=CARTESIAN_POINT('Ctrl Pts',(-18.8184836904943,4.28651781099017,0.859475332311362));
#52542=CARTESIAN_POINT('Ctrl Pts',(-18.6196101587968,1.59422735686541,4.07079499918746));
#52543=CARTESIAN_POINT('Ctrl Pts',(-18.4207366270994,-2.56284246613059,
3.54185986235838));
#52544=CARTESIAN_POINT('Ctrl Pts',(-18.2218630954019,-4.36516736903167,
-0.241343388409285));
#52545=CARTESIAN_POINT('Ctrl Pts',(-18.0229895637045,-2.156767530388,-3.80279983836275));
#52546=CARTESIAN_POINT('Ctrl Pts',(-17.824116032007,2.03327474360769,-3.87023598864389));
#52547=CARTESIAN_POINT('Ctrl Pts',(-17.6252425003096,4.35514000830941,-0.381691365909796));
#52548=CARTESIAN_POINT('Ctrl Pts',(-17.4263689686121,2.67549369108707,3.45755206753867));
#52549=CARTESIAN_POINT('Ctrl Pts',(-17.2274954369147,-1.46240172302391,
4.11998956203585));
#52550=CARTESIAN_POINT('Ctrl Pts',(-17.0286219052172,-4.25663943131118,
0.996972187472916));
#52551=CARTESIAN_POINT('Ctrl Pts',(-16.8297483735197,-3.13986809006872,
-3.04206527999579));
#52552=CARTESIAN_POINT('Ctrl Pts',(-16.6308748418223,0.861820499333901,
-4.28604692201515));
#52553=CARTESIAN_POINT('Ctrl Pts',(-16.4320013101249,4.07166664439615,-1.59199985166439));
#52554=CARTESIAN_POINT('Ctrl Pts',(-16.2331277784274,3.54045711634576,2.56477995120524));
#52555=CARTESIAN_POINT('Ctrl Pts',(-16.0342542467299,-0.243731679726614,
4.36503466871517));
#52556=CARTESIAN_POINT('Ctrl Pts',(-15.8353807150324,-3.8039793080186,2.15468657000362));
#52557=CARTESIAN_POINT('Ctrl Pts',(-15.636507183335,-3.8691229374967,-2.035391973386));
#52558=CARTESIAN_POINT('Ctrl Pts',(-15.4376336516376,-0.379308467639,-4.35534819241408));
#52559=CARTESIAN_POINT('Ctrl Pts',(-15.2387601199401,3.45901540110913,-2.6736015495353));
#52560=CARTESIAN_POINT('Ctrl Pts',(-15.0398865882427,4.11918881701681,1.46465568668931));
#52561=CARTESIAN_POINT('Ctrl Pts',(-14.8410130565452,0.994643090032016,
4.25718427064641));
#52562=CARTESIAN_POINT('Ctrl Pts',(-14.6421395248478,-3.04378275034757,
3.13820320557389));
#52563=CARTESIAN_POINT('Ctrl Pts',(-14.4432659931503,-4.28557474999217,
-0.864165408366494));
#52564=CARTESIAN_POINT('Ctrl Pts',(-14.2443924614529,-1.58977186989086,
-4.07253707073262));
#52565=CARTESIAN_POINT('Ctrl Pts',(-14.0455189297554,2.56671666850115,-3.53905331048093));
#52566=CARTESIAN_POINT('Ctrl Pts',(-13.8466453980579,4.36490066170536,0.246119898081736));
#52567=CARTESIAN_POINT('Ctrl Pts',(-13.6477718663605,2.15260496460386,3.80515763893567));
#52568=CARTESIAN_POINT('Ctrl Pts',(-13.448898334663,-2.03750859386031,3.86800872810968));
#52569=CARTESIAN_POINT('Ctrl Pts',(-13.2500248029656,-4.35555507272516,
0.376925455820456));
#52570=CARTESIAN_POINT('Ctrl Pts',(-13.0511512712682,-2.67170860762853,
-3.46047769920734));
#52571=CARTESIAN_POINT('Ctrl Pts',(-12.8522777395706,1.46690921190324,-4.11838683889956));
#52572=CARTESIAN_POINT('Ctrl Pts',(-12.6534042078732,4.25772783557386,-0.992313694840112));
#52573=CARTESIAN_POINT('Ctrl Pts',(-12.4545306761757,3.13653738164341,3.04549930952892));
#52574=CARTESIAN_POINT('Ctrl Pts',(-12.2556571444783,-0.866510058707176,
4.28510129506258));
#52575=CARTESIAN_POINT('Ctrl Pts',(-12.0567836127808,-4.07340627793628,
1.58754341221176));
#52576=CARTESIAN_POINT('Ctrl Pts',(-11.8579100810834,-3.53764844518413,
-2.56865261743856));
#52577=CARTESIAN_POINT('Ctrl Pts',(-11.6590365493859,0.248508042759728,
-4.36476534804237));
#52578=CARTESIAN_POINT('Ctrl Pts',(-11.4601630176885,3.8063348307612,-2.15052271481186));
#52579=CARTESIAN_POINT('Ctrl Pts',(-11.261289485991,3.86689336081636,2.03962460439701));
#52580=CARTESIAN_POINT('Ctrl Pts',(-11.0624159542936,0.374542331167539,
4.35576064918068));
#52581=CARTESIAN_POINT('Ctrl Pts',(-10.8635424225961,-3.46193896139555,
2.66981486593344));
#52582=CARTESIAN_POINT('Ctrl Pts',(-10.6646688908987,-4.11758362792416,
-1.46916229799113));
#52583=CARTESIAN_POINT('Ctrl Pts',(-10.4657953592012,-0.989984002594516,
-4.25827012593079));
#52584=CARTESIAN_POINT('Ctrl Pts',(-10.2669218275038,3.04721495702597,-3.13487061877597));
#52585=CARTESIAN_POINT('Ctrl Pts',(-10.0680482958063,4.2846265573681,0.868854449654062));
#52586=CARTESIAN_POINT('Ctrl Pts',(-9.86917476410884,1.58531447929421,4.07427426574695));
#52587=CARTESIAN_POINT('Ctrl Pts',(-9.67030123241142,-2.57058779743794,
3.53624252087591));
#52588=CARTESIAN_POINT('Ctrl Pts',(-9.47142770071392,-4.36462872776664,
-0.250896113045607));
#52589=CARTESIAN_POINT('Ctrl Pts',(-9.27255416901652,-2.14843982125103,
-3.80751088314276));
#52590=CARTESIAN_POINT('Ctrl Pts',(-9.07368063731904,2.04174000436261,-3.86577683595071));
#52591=CARTESIAN_POINT('Ctrl Pts',(-8.87480710562161,4.35596492171907,-0.37215909439371));
#52592=CARTESIAN_POINT('Ctrl Pts',(-8.67593357392413,2.667920325017,3.46339918723626));
#52593=CARTESIAN_POINT('Ctrl Pts',(-8.4770600422267,-1.47141494427834,4.11677918433113));
#52594=CARTESIAN_POINT('Ctrl Pts',(-8.27818651052922,-4.25881114155487,
0.987654013992727));
#52595=CARTESIAN_POINT('Ctrl Pts',(-8.07931297883178,-3.1332029174706,-3.04892969232504));
#52596=CARTESIAN_POINT('Ctrl Pts',(-7.88043944713431,0.871198580505213,
-4.28415053705085));
#52597=CARTESIAN_POINT('Ctrl Pts',(-7.68156591543687,4.07514103390481,-1.58308507180563));
#52598=CARTESIAN_POINT('Ctrl Pts',(-7.48269238373942,3.53483553797703,2.57252220791998));
#52599=CARTESIAN_POINT('Ctrl Pts',(-7.28381885204197,-0.253284108224254,
4.36449080091907));
#52600=CARTESIAN_POINT('Ctrl Pts',(-7.0849453203445,-3.808685795729,2.14635628454501));
#52601=CARTESIAN_POINT('Ctrl Pts',(-6.88607178864706,-3.86465915384566,
-2.0438547931245));
#52602=CARTESIAN_POINT('Ctrl Pts',(-6.68719825694959,-0.36977574621432,
-4.35616789027829));
#52603=CARTESIAN_POINT('Ctrl Pts',(-6.48832472525215,3.46485837629675,-2.66602498544807));
#52604=CARTESIAN_POINT('Ctrl Pts',(-6.28945119355468,4.11597350835323,1.47366715009494));
#52605=CARTESIAN_POINT('Ctrl Pts',(-6.09057766185723,0.985323729746626,
4.25935088227696));
#52606=CARTESIAN_POINT('Ctrl Pts',(-5.89170413015977,-3.05064351494095,
3.13153427823985));
#52607=CARTESIAN_POINT('Ctrl Pts',(-5.69283059846234,-4.28367323420068,
-0.873542450584943));
#52608=CARTESIAN_POINT('Ctrl Pts',(-5.49395706676489,-1.58085519051244,
-4.07600658210169));
#52609=CARTESIAN_POINT('Ctrl Pts',(-5.29508353506742,2.57445584849332,-3.53342749700076));
#52610=CARTESIAN_POINT('Ctrl Pts',(-5.09621000336997,4.36435156718664,0.255672027754977));
#52611=CARTESIAN_POINT('Ctrl Pts',(-4.89733647167251,2.14427210598631,3.80985956783942));
#52612=CARTESIAN_POINT('Ctrl Pts',(-4.69846293997507,-2.04596897131221,
3.86354031545655));
#52613=CARTESIAN_POINT('Ctrl Pts',(-4.49958940827759,-4.35636955241326,
0.367392286171182));
#52614=CARTESIAN_POINT('Ctrl Pts',(-4.30071587658015,-2.66412885229606,
-3.46631652592691));
#52615=CARTESIAN_POINT('Ctrl Pts',(-4.10184234488268,1.47591892326601,-4.11516660441047));
#52616=CARTESIAN_POINT('Ctrl Pts',(-3.90296881318523,4.25988933188569,-0.982993142664311));
#52617=CARTESIAN_POINT('Ctrl Pts',(-3.70409528148781,3.12986473188877,3.0523564094626));
#52618=CARTESIAN_POINT('Ctrl Pts',(-3.50522174979033,-0.875886116413711,
4.28319467709064));
#52619=CARTESIAN_POINT('Ctrl Pts',(-3.3063482180929,-4.07687080203127,1.57862478296689));
#52620=CARTESIAN_POINT('Ctrl Pts',(-3.10747468639542,-3.53201860238364,
-2.57638861828632));
#52621=CARTESIAN_POINT('Ctrl Pts',(-2.90860115469799,0.258060256144617,
-4.36421121598415));
#52622=CARTESIAN_POINT('Ctrl Pts',(-2.70972762300051,3.81103147174565,-2.14218692862399));
#52623=CARTESIAN_POINT('Ctrl Pts',(-2.51085409130307,3.86242169455405,2.04808186311882));
#52624=CARTESIAN_POINT('Ctrl Pts',(-2.3119805596056,0.365006121651707,4.35657118292956));
#52625=CARTESIAN_POINT('Ctrl Pts',(-2.11310702790815,-3.46776873896351,
2.66222951892241));
#52626=CARTESIAN_POINT('Ctrl Pts',(-1.91423349621071,-4.11436771876071,
-1.47816571782307));
#52627=CARTESIAN_POINT('Ctrl Pts',(-1.71535996451324,-0.980644795081548,
-4.2604350726622));
#52628=CARTESIAN_POINT('Ctrl Pts',(-1.51648643281581,3.05403541042053,-3.12817807350787));
#52629=CARTESIAN_POINT('Ctrl Pts',(-1.31761290111834,4.28277711056433,0.878198978078091));
#52630=CARTESIAN_POINT('Ctrl Pts',(-1.1187393694209,1.57627631789302,4.0777914718176));
#52631=CARTESIAN_POINT('Ctrl Pts',(-0.919865837723429,-2.57809858195644,
3.53049975027877));
#52632=CARTESIAN_POINT('Ctrl Pts',(-0.720992306025984,-4.36448889159331,
-0.260242724958486));
#52633=CARTESIAN_POINT('Ctrl Pts',(-0.522118774328522,-2.13930861817419,
-3.81259106820431));
#52634=CARTESIAN_POINT('Ctrl Pts',(-0.323245242631061,2.04869198938347,
-3.86056393295148));
#52635=CARTESIAN_POINT('Ctrl Pts',(-0.124371710933644,4.35965501372303,
-0.364044245942155));
#52636=CARTESIAN_POINT('Ctrl Pts',(0.0745018207638594,2.65450071084487,
3.47215873439577));
#52637=CARTESIAN_POINT('Ctrl Pts',(0.207084175228801,-0.0927661781443274,
3.89494769144758));
#52638=CARTESIAN_POINT('Ctrl Pts',(0.273375352461282,-1.251650112727,3.47787809703136));
#52639=CARTESIAN_POINT('Ctrl Pts',(-109.567,-1.74869447532986,3.5228619944515));
#52640=CARTESIAN_POINT('Ctrl Pts',(-109.500708822768,-2.92256775530673,
2.9401693648038));
#52641=CARTESIAN_POINT('Ctrl Pts',(-109.368126468303,-4.62148961478483,
0.519149110062505));
#52642=CARTESIAN_POINT('Ctrl Pts',(-109.169252936605,-2.93168196537142,
-3.61588934021046));
#52643=CARTESIAN_POINT('Ctrl Pts',(-108.970379404908,1.45547172051883,-4.41678188493319));
#52644=CARTESIAN_POINT('Ctrl Pts',(-108.77150587321,4.50342526464322,-1.16551591507676));
#52645=CARTESIAN_POINT('Ctrl Pts',(-108.572632341513,3.41462717220614,3.15976482950097));
#52646=CARTESIAN_POINT('Ctrl Pts',(-108.373758809815,-0.812068679813194,
4.58019051839891));
#52647=CARTESIAN_POINT('Ctrl Pts',(-108.174885278118,-4.2923528809395,1.79320458261704));
#52648=CARTESIAN_POINT('Ctrl Pts',(-107.976011746421,-3.82896339678044,
-2.64184571159234));
#52649=CARTESIAN_POINT('Ctrl Pts',(-107.777138214723,0.152564403965833,
-4.64931685129564));
#52650=CARTESIAN_POINT('Ctrl Pts',(-107.578264683026,3.99387393908369,-2.38511634519291));
#52651=CARTESIAN_POINT('Ctrl Pts',(-107.379391151328,4.16562602423641,2.07060292291838));
#52652=CARTESIAN_POINT('Ctrl Pts',(-107.180517619631,0.509980647258628,
4.62381144888953));
#52653=CARTESIAN_POINT('Ctrl Pts',(-106.981644087933,-3.61422978970552,
2.92867186548573));
#52654=CARTESIAN_POINT('Ctrl Pts',(-106.782770556236,-4.41768176152901,
-1.45734768584626));
#52655=CARTESIAN_POINT('Ctrl Pts',(-106.583897024538,-1.16215691953748,
-4.50434776553196));
#52656=CARTESIAN_POINT('Ctrl Pts',(-106.385023492841,3.16115916451212,-3.41274674299064));
#52657=CARTESIAN_POINT('Ctrl Pts',(-106.186149961143,4.5799962056956,0.814494516072427));
#52658=CARTESIAN_POINT('Ctrl Pts',(-105.987276429446,1.79072307054798,4.29337573545735));
#52659=CARTESIAN_POINT('Ctrl Pts',(-105.788402897749,-2.64386996172864,
3.82749494045799));
#52660=CARTESIAN_POINT('Ctrl Pts',(-105.589529366051,-4.64926991710361,
-0.155096290772498));
#52661=CARTESIAN_POINT('Ctrl Pts',(-105.390655834354,-2.38291108801837,
-3.99518461187035));
#52662=CARTESIAN_POINT('Ctrl Pts',(-105.191782302656,2.07287132116358,-4.16448917178079));
#52663=CARTESIAN_POINT('Ctrl Pts',(-104.992908770959,4.62409531506305,-0.507452496249705));
#52664=CARTESIAN_POINT('Ctrl Pts',(-104.794035239261,2.92669103324941,3.61583255699087));
#52665=CARTESIAN_POINT('Ctrl Pts',(-104.595161707564,-1.45976297618673,
4.41688324199641));
#52666=CARTESIAN_POINT('Ctrl Pts',(-104.396288175866,-4.50498376741142,
1.15969253020268));
#52667=CARTESIAN_POINT('Ctrl Pts',(-104.197414644169,-3.41101622233145,
-3.16302605686458));
#52668=CARTESIAN_POINT('Ctrl Pts',(-103.998541112471,0.817000031123855,
-4.57954980972901));
#52669=CARTESIAN_POINT('Ctrl Pts',(-103.799667580774,4.29435497869652,-1.78837379360953));
#52670=CARTESIAN_POINT('Ctrl Pts',(-103.600794049077,3.82604775423565,2.64596373570485));
#52671=CARTESIAN_POINT('Ctrl Pts',(-103.401920517379,-0.157640002669139,
4.64918435197667));
#52672=CARTESIAN_POINT('Ctrl Pts',(-103.203046985682,-3.99648780147895,
2.38072483949959));
#52673=CARTESIAN_POINT('Ctrl Pts',(-103.004173453984,-4.16335440239243,
-2.07514954372844));
#52674=CARTESIAN_POINT('Ctrl Pts',(-102.805299922287,-0.504922429896287,
-4.62437226536201));
#52675=CARTESIAN_POINT('Ctrl Pts',(-102.606426390589,3.6174333079372,-2.92471225446792));
#52676=CARTESIAN_POINT('Ctrl Pts',(-102.407552858892,4.41608389485863,1.46217938105407));
#52677=CARTESIAN_POINT('Ctrl Pts',(-102.208679327194,1.15722753176151,4.50561759901536));
#52678=CARTESIAN_POINT('Ctrl Pts',(-102.009805795497,-3.16489186362239,
3.4092851157379));
#52679=CARTESIAN_POINT('Ctrl Pts',(-101.810932263799,-4.57910211632402,
-0.819505532069846));
#52680=CARTESIAN_POINT('Ctrl Pts',(-101.612058732102,-1.78602394240258,
-4.29533281434428));
#52681=CARTESIAN_POINT('Ctrl Pts',(-101.413185200404,2.64805669699241,-3.82459948730979));
#52682=CARTESIAN_POINT('Ctrl Pts',(-101.214311668707,4.64909740600855,0.160183701609936));
#52683=CARTESIAN_POINT('Ctrl Pts',(-101.015438137009,2.37853787251991,3.99778977658976));
#52684=CARTESIAN_POINT('Ctrl Pts',(-100.816564605312,-2.0774271420266,4.16221839628679));
#52685=CARTESIAN_POINT('Ctrl Pts',(-100.617691073615,-4.6246478329549,0.50239220730669));
#52686=CARTESIAN_POINT('Ctrl Pts',(-100.418817541917,-2.92273259930173,
-3.61903297329493));
#52687=CARTESIAN_POINT('Ctrl Pts',(-100.21994401022,1.46459534775654,-4.41528322717206));
#52688=CARTESIAN_POINT('Ctrl Pts',(-100.021070478522,4.50625008208266,-1.15476218614357));
#52689=CARTESIAN_POINT('Ctrl Pts',(-99.8221969468247,3.40755298843155,3.16675672255514));
#52690=CARTESIAN_POINT('Ctrl Pts',(-99.6233234151276,-0.822010787625527,
4.57865305235549));
#52691=CARTESIAN_POINT('Ctrl Pts',(-99.4244498834296,-4.29630936420008,
1.78367355642891));
#52692=CARTESIAN_POINT('Ctrl Pts',(-99.2255763517326,-3.82315007545343,
-2.65014886551254));
#52693=CARTESIAN_POINT('Ctrl Pts',(-99.0267028200349,0.162727352588974,
-4.64900906834309));
#52694=CARTESIAN_POINT('Ctrl Pts',(-98.8278292883376,3.99909055494903,-2.37635019349726));
#52695=CARTESIAN_POINT('Ctrl Pts',(-98.62895575664,4.161081144199,2.07970411842853));
#52696=CARTESIAN_POINT('Ctrl Pts',(-98.4300822249428,0.499861834325147,
4.62492201614277));
#52697=CARTESIAN_POINT('Ctrl Pts',(-98.2312086932451,-3.62063155527922,
2.92075206919953));
#52698=CARTESIAN_POINT('Ctrl Pts',(-98.0323351615478,-4.41448123774961,
-1.46701087602433));
#52699=CARTESIAN_POINT('Ctrl Pts',(-97.8334616298503,-1.15229649484245,
-4.50688121618384));
#52700=CARTESIAN_POINT('Ctrl Pts',(-97.6345880981527,3.16862063350473,-3.4058198410581));
#52701=CARTESIAN_POINT('Ctrl Pts',(-97.4357145664554,4.57820261774596,0.824515797108271));
#52702=CARTESIAN_POINT('Ctrl Pts',(-97.236841034758,1.78132263650433,4.29728462793591));
#52703=CARTESIAN_POINT('Ctrl Pts',(-97.0379675030604,-2.65224024069837,
3.82169951911937));
#52704=CARTESIAN_POINT('Ctrl Pts',(-96.8390939713631,-4.64891933897527,
-0.165270954854797));
#52705=CARTESIAN_POINT('Ctrl Pts',(-96.6402204396655,-2.3741618031032,-4.00039013616206));
#52706=CARTESIAN_POINT('Ctrl Pts',(-96.4413469079682,2.08198047226141,-4.15994264647233));
#52707=CARTESIAN_POINT('Ctrl Pts',(-96.2424733762706,4.62519481483885,-0.49733131170768));
#52708=CARTESIAN_POINT('Ctrl Pts',(-96.0435998445732,2.9187706647567,3.62222905341074));
#52709=CARTESIAN_POINT('Ctrl Pts',(-95.8447263128757,-1.46942596513563,
4.41367792683178));
#52710=CARTESIAN_POINT('Ctrl Pts',(-95.6458527811783,-4.50751100112929,
1.14983045859604));
#52711=CARTESIAN_POINT('Ctrl Pts',(-95.4469792494808,-3.40408567413676,
-3.17048359591309));
#52712=CARTESIAN_POINT('Ctrl Pts',(-95.2481057177833,0.827020559768415,
-4.5777508126303));
#52713=CARTESIAN_POINT('Ctrl Pts',(-95.049232186086,4.29825860525972,-1.7789711833326));
#52714=CARTESIAN_POINT('Ctrl Pts',(-94.8503586543885,3.8202478187419,2.6543308219238));
#52715=CARTESIAN_POINT('Ctrl Pts',(-94.6514851226909,-0.167814507645974,
4.64882821793195));
#52716=CARTESIAN_POINT('Ctrl Pts',(-94.4526115909937,-4.00168851983982,
2.37197270199285));
#52717=CARTESIAN_POINT('Ctrl Pts',(-94.2537380592959,-4.1588029034476,-2.08425620284382));
#52718=CARTESIAN_POINT('Ctrl Pts',(-94.0548645275989,-0.494800640211771,
-4.62546622896147));
#52719=CARTESIAN_POINT('Ctrl Pts',(-93.8559909959011,3.62382546721121,-2.91678838656638));
#52720=CARTESIAN_POINT('Ctrl Pts',(-93.6571174642038,4.41287329465908,1.47184061436746));
#52721=CARTESIAN_POINT('Ctrl Pts',(-93.4582439325062,1.14736407814257,4.50813943673051));
#52722=CARTESIAN_POINT('Ctrl Pts',(-93.2593704008089,-3.17234560922253,
3.4023504881866));
#52723=CARTESIAN_POINT('Ctrl Pts',(-93.0604968691113,-4.57729763714377,
-0.829525074856124));
#52724=CARTESIAN_POINT('Ctrl Pts',(-92.8616233374139,-1.77661919761762,
-4.29923129587995));
#52725=CARTESIAN_POINT('Ctrl Pts',(-92.6627498057165,2.65642060856304,-3.81879497475558));
#52726=CARTESIAN_POINT('Ctrl Pts',(-92.4638762740189,4.64873570524042,0.170358010201121));
#52727=CARTESIAN_POINT('Ctrl Pts',(-92.2650027423217,2.36978289082147,4.00298570559363));
#52728=CARTESIAN_POINT('Ctrl Pts',(-92.0661292106241,-2.0865313094945,4.15766191546598));
#52729=CARTESIAN_POINT('Ctrl Pts',(-91.8672556789266,-4.6257362584294,0.492269820595009));
#52730=CARTESIAN_POINT('Ctrl Pts',(-91.6683821472293,-2.91480523522198,
-3.62542079620279));
#52731=CARTESIAN_POINT('Ctrl Pts',(-91.4695086155317,1.47425482299701,-4.41206734147235));
#52732=CARTESIAN_POINT('Ctrl Pts',(-91.2706350838344,4.50876652279934,-1.14489735422035));
#52733=CARTESIAN_POINT('Ctrl Pts',(-91.0717615521368,3.4006142837271,3.17420667287565));
#52734=CARTESIAN_POINT('Ctrl Pts',(-90.8728880204394,-0.83202934162167,
4.57684309142205));
#52735=CARTESIAN_POINT('Ctrl Pts',(-90.6740144887419,-4.30020269950541,
1.77426668006346));
#52736=CARTESIAN_POINT('Ctrl Pts',(-90.4751409570445,-3.81734098759532,
-2.65850959999049));
#52737=CARTESIAN_POINT('Ctrl Pts',(-90.276267425347,0.172901461758815,-4.64864180092837));
#52738=CARTESIAN_POINT('Ctrl Pts',(-90.0773938936496,4.00428169303516,-2.36759237024463));
#52739=CARTESIAN_POINT('Ctrl Pts',(-89.8785203619521,4.15651968286905,2.08880579153238));
#52740=CARTESIAN_POINT('Ctrl Pts',(-89.6796468302546,0.489738853614996,
4.62600490316179));
#52741=CARTESIAN_POINT('Ctrl Pts',(-89.4807732985572,-3.62701503990788,
2.91282121131715));
#52742=CARTESIAN_POINT('Ctrl Pts',(-89.2818997668597,-4.41126006751287,
-1.47666859030155));
#52743=CARTESIAN_POINT('Ctrl Pts',(-89.0830262351625,-1.14243028756782,
-4.50939225914807));
#52744=CARTESIAN_POINT('Ctrl Pts',(-88.8841527034647,3.17606678631533,-3.39887706127799));
#52745=CARTESIAN_POINT('Ctrl Pts',(-88.6852791717675,4.57638717560117,0.834533359315383));
#52746=CARTESIAN_POINT('Ctrl Pts',(-88.4864056400698,1.77191363137438,4.30117281584531));
#52747=CARTESIAN_POINT('Ctrl Pts',(-88.2875321083726,-2.66059779558081,
3.8158858576964));
#52748=CARTESIAN_POINT('Ctrl Pts',(-88.088658576675,-4.64854650502389,-0.175444861557656));
#52749=CARTESIAN_POINT('Ctrl Pts',(-87.8897850449775,-2.36540114091807,
-4.00557648177645));
#52750=CARTESIAN_POINT('Ctrl Pts',(-87.6909115132801,2.0910796482766,-4.15537620599874));
#52751=CARTESIAN_POINT('Ctrl Pts',(-87.4920379815827,4.62627216307823,-0.487207740029394));
#52752=CARTESIAN_POINT('Ctrl Pts',(-87.2931644498852,2.91083631544583,3.62860819784926));
#52753=CARTESIAN_POINT('Ctrl Pts',(-87.0942909181878,-1.47908191555853,
4.4104514730223));
#52754=CARTESIAN_POINT('Ctrl Pts',(-86.8954173864902,-4.51001664558938,
1.1399628789235));
#52755=CARTESIAN_POINT('Ctrl Pts',(-86.696543854793,-3.39713882135932,-3.17792594898473));
#52756=CARTESIAN_POINT('Ctrl Pts',(-86.4976703230953,0.837037127187677,
-4.57592988981764));
#52757=CARTESIAN_POINT('Ctrl Pts',(-86.298796791398,4.30214164460925,-1.76956005225475));
#52758=CARTESIAN_POINT('Ctrl Pts',(-86.0999232597005,3.8144295854944,2.66268519470887));
#52759=CARTESIAN_POINT('Ctrl Pts',(-85.901049728003,-0.177988208836268,
4.64844981755554));
#52760=CARTESIAN_POINT('Ctrl Pts',(-85.7021761963055,-4.0068700714299,2.36320920349774));
#52761=CARTESIAN_POINT('Ctrl Pts',(-85.5033026646083,-4.15423148519735,
-2.09335287904645));
#52762=CARTESIAN_POINT('Ctrl Pts',(-85.3044291329106,-0.484676480595899,
-4.62653803809871));
#52763=CARTESIAN_POINT('Ctrl Pts',(-85.1055556012133,3.63020026954995,-2.90885054820222));
#52764=CARTESIAN_POINT('Ctrl Pts',(-84.9066820695158,4.4096415582427,1.48149479804545));
#52765=CARTESIAN_POINT('Ctrl Pts',(-84.7078085378183,1.13749512902607,4.51063968193637));
#52766=CARTESIAN_POINT('Ctrl Pts',(-84.5089350061209,-3.17978416032731,
3.39539956449144));
#52767=CARTESIAN_POINT('Ctrl Pts',(-84.3100614744233,-4.57547123420834,
-0.839540644489037));
#52768=CARTESIAN_POINT('Ctrl Pts',(-84.1111879427261,-1.76720594340918,
-4.30310918550717));
#52769=CARTESIAN_POINT('Ctrl Pts',(-83.9123144110284,2.66477179674978,-3.81297217142531));
#52770=CARTESIAN_POINT('Ctrl Pts',(-83.7134408793312,4.64835173855226,0.180531502833249));
#52771=CARTESIAN_POINT('Ctrl Pts',(-83.5145673476335,2.36101655863981,4.00816246160827));
#52772=CARTESIAN_POINT('Ctrl Pts',(-83.3156938159363,-2.09562548316145,
4.15308552080756));
#52773=CARTESIAN_POINT('Ctrl Pts',(-83.1168202842386,-4.62680252814361,
0.482145076072292));
#52774=CARTESIAN_POINT('Ctrl Pts',(-82.9179467525412,-2.90686391018077,
-3.63179125453341));
#52775=CARTESIAN_POINT('Ctrl Pts',(-82.7190732208439,1.48390723704007,-4.40883032341654));
#52776=CARTESIAN_POINT('Ctrl Pts',(-82.5201996891462,4.5112613680025,-1.13502703861416));
#52777=CARTESIAN_POINT('Ctrl Pts',(-82.321326157449,3.393659291195,3.1816414197868));
#52778=CARTESIAN_POINT('Ctrl Pts',(-82.1224526257514,-0.842043910469987,
4.57501120891056));
#52779=CARTESIAN_POINT('Ctrl Pts',(-81.923579094054,-4.30407543824946,1.76485130554235));
#52780=CARTESIAN_POINT('Ctrl Pts',(-81.7247055623566,-3.81151361592538,
-2.66685760107894));
#52781=CARTESIAN_POINT('Ctrl Pts',(-81.525832030659,0.18307474278733,-4.64825226804338));
#52782=CARTESIAN_POINT('Ctrl Pts',(-81.3269584989616,4.00945365192469,-2.35882320700066));
#52783=CARTESIAN_POINT('Ctrl Pts',(-81.1280849672642,4.15193831317242,2.09789745994127));
#52784=CARTESIAN_POINT('Ctrl Pts',(-80.9292114355667,0.479613527216301,
4.62706563313381));
#52785=CARTESIAN_POINT('Ctrl Pts',(-80.7303379038692,-3.63338115232342,
2.90487640197613));
#52786=CARTESIAN_POINT('Ctrl Pts',(-80.5314643721718,-4.4080177687866,-1.48631923182023));
#52787=CARTESIAN_POINT('Ctrl Pts',(-80.3325908404743,-1.13255860842666,
-4.51188170360169));
#52788=CARTESIAN_POINT('Ctrl Pts',(-80.1337173087769,3.18349772680722,-3.39191800199096));
#52789=CARTESIAN_POINT('Ctrl Pts',(-79.9348437770794,4.57454981406204,0.844546924381235));
#52790=CARTESIAN_POINT('Ctrl Pts',(-79.7359702453821,1.76249613935908,4.3050404025469));
#52791=CARTESIAN_POINT('Ctrl Pts',(-79.5370967136844,-2.66894260707198,
3.81005391943118));
#52792=CARTESIAN_POINT('Ctrl Pts',(-79.3382231819871,-4.64815140605869,
-0.185617927937138));
#52793=CARTESIAN_POINT('Ctrl Pts',(-79.1393496502896,-2.35662914923688,
-4.0107436419926));
#52794=CARTESIAN_POINT('Ctrl Pts',(-78.9404761185922,2.10016880870579,-4.15078986263536));
#52795=CARTESIAN_POINT('Ctrl Pts',(-78.7416025868947,4.62732735299052,-0.477081834785776));
#52796=CARTESIAN_POINT('Ctrl Pts',(-78.5427290551972,2.90288802418331,3.63496996244397));
#52797=CARTESIAN_POINT('Ctrl Pts',(-78.3438555234999,-1.48873078166386,
4.40720389459616));
#52798=CARTESIAN_POINT('Ctrl Pts',(-78.1449819918022,-4.51250068854823,
1.13008983920251));
#52799=CARTESIAN_POINT('Ctrl Pts',(-77.9461084601051,-3.39017569740059,
-3.18535308083288));
#52800=CARTESIAN_POINT('Ctrl Pts',(-77.7472349284073,0.847049685473463,
-4.57408704980088));
#52801=CARTESIAN_POINT('Ctrl Pts',(-77.5483613967101,4.30600407811059,-1.76014044556444));
#52802=CARTESIAN_POINT('Ctrl Pts',(-77.3494878650125,3.80859308237973,2.67102681410471));
#52803=CARTESIAN_POINT('Ctrl Pts',(-77.1506143333151,-0.188161057521362,
4.64804915262839));
#52804=CARTESIAN_POINT('Ctrl Pts',(-76.9517408016176,-4.01203243142588,
2.35443438600527));
#52805=CARTESIAN_POINT('Ctrl Pts',(-76.7528672699202,-4.14964016954015,
-2.10243952877506));
#52806=CARTESIAN_POINT('Ctrl Pts',(-76.5539937382226,-0.474549999538605,
-4.6275876876354));
#52807=CARTESIAN_POINT('Ctrl Pts',(-76.3551202065254,3.63655768441947,-2.90089877739755));
#52808=CARTESIAN_POINT('Ctrl Pts',(-76.1562466748277,4.40638870108887,1.49114188584904));
#52809=CARTESIAN_POINT('Ctrl Pts',(-75.9573731431305,1.12762073168075,4.51311832265683));
#52810=CARTESIAN_POINT('Ctrl Pts',(-75.7584996114328,-3.18720748130837,
3.38843237794545));
#52811=CARTESIAN_POINT('Ctrl Pts',(-75.5596260797356,-4.57362291626562,
-0.849552192997447));
#52812=CARTESIAN_POINT('Ctrl Pts',(-75.3607525480378,-1.75778422486363,
-4.30696646465206));
#52813=CARTESIAN_POINT('Ctrl Pts',(-75.1618790163406,2.67311022155321,-3.80713110520833));
#52814=CARTESIAN_POINT('Ctrl Pts',(-74.963005484643,4.64794550778309,0.190704130778702));
#52815=CARTESIAN_POINT('Ctrl Pts',(-74.7641319529456,2.35223891796283,4.0133200198387));
#52816=CARTESIAN_POINT('Ctrl Pts',(-74.5652584212482,-2.10470961946934,
4.14848923423098));
#52817=CARTESIAN_POINT('Ctrl Pts',(-74.3663848895507,-4.6278466369905,0.472018022232693));
#52818=CARTESIAN_POINT('Ctrl Pts',(-74.1675113578532,-2.89890866221432,
-3.6381443177746));
#52819=CARTESIAN_POINT('Ctrl Pts',(-73.9686378261559,1.49355254365402,-4.40557218850874));
#52820=CARTESIAN_POINT('Ctrl Pts',(-73.7697642944583,4.5137346057426,-1.1251512866005));
#52821=CARTESIAN_POINT('Ctrl Pts',(-73.570890762761,3.38668804414742,3.18906092767856));
#52822=CARTESIAN_POINT('Ctrl Pts',(-73.3720172310633,-0.852054446204056,
4.5731574135952));
#52823=CARTESIAN_POINT('Ctrl Pts',(-73.1731436993661,-4.3079275618832,1.75542747796197));
#52824=CARTESIAN_POINT('Ctrl Pts',(-72.9742701676685,-3.80566798835464,
-2.6751928287938));
#52825=CARTESIAN_POINT('Ctrl Pts',(-72.7753966359711,0.193247146947877,
-4.64784047155381));
#52826=CARTESIAN_POINT('Ctrl Pts',(-72.5765231042737,4.01460640684562,-2.3500427457668));
#52827=CARTESIAN_POINT('Ctrl Pts',(-72.3776495725761,4.14733705705237,2.10697908010902));
#52828=CARTESIAN_POINT('Ctrl Pts',(-72.1787760408788,0.469485903626064,
4.62810420097833));
#52829=CARTESIAN_POINT('Ctrl Pts',(-71.9799025091812,-3.63972986203442,
2.89691767922942));
#52830=CARTESIAN_POINT('Ctrl Pts',(-71.7810289774839,-4.40475435710021,
-1.49596275435712));
#52831=CARTESIAN_POINT('Ctrl Pts',(-71.5821554457863,-1.12268150470101,
-4.51434953762105));
#52832=CARTESIAN_POINT('Ctrl Pts',(-71.3832819140889,3.19091341938862,-3.38494269652865));
#52833=CARTESIAN_POINT('Ctrl Pts',(-71.1844083823914,4.57269054192897,0.854556444344225));
#52834=CARTESIAN_POINT('Ctrl Pts',(-70.985534850694,1.75307020556499,4.30888736951631));
#52835=CARTESIAN_POINT('Ctrl Pts',(-70.7866613189966,-2.67727463520306,
3.80420373225664));
#52836=CARTESIAN_POINT('Ctrl Pts',(-70.587787787299,-4.64773404397201,-0.195790105267626));
#52837=CARTESIAN_POINT('Ctrl Pts',(-70.3889142556017,-2.34784587007461,
-4.01589159206155));
#52838=CARTESIAN_POINT('Ctrl Pts',(-70.1900407239042,2.10924791001481,-4.14618363834924));
#52839=CARTESIAN_POINT('Ctrl Pts',(-69.9911671922067,4.62836037952177,-0.466953644476603));
#52840=CARTESIAN_POINT('Ctrl Pts',(-69.7922936605093,2.89492582903878,3.64131431672428));
#52841=CARTESIAN_POINT('Ctrl Pts',(-69.5934201288119,-1.49837251723686,
4.4039352071081));
#52842=CARTESIAN_POINT('Ctrl Pts',(-69.3945465971143,-4.51496311810808,
1.12021138672163));
#52843=CARTESIAN_POINT('Ctrl Pts',(-69.195673065417,-3.38319633561165,-3.19276495588401));
#52844=CARTESIAN_POINT('Ctrl Pts',(-68.9967995337194,0.857058186668978,
-4.57222230140667));
#52845=CARTESIAN_POINT('Ctrl Pts',(-68.797926002022,4.30984588726406,-1.75071240837834));
#52846=CARTESIAN_POINT('Ctrl Pts',(-68.5990524703246,3.80273833735267,2.67935564015779));
#52847=CARTESIAN_POINT('Ctrl Pts',(-68.4001789386271,-0.198333004976704,
4.64762622506952));
#52848=CARTESIAN_POINT('Ctrl Pts',(-68.2013054069296,-4.01717557510177,
2.34564829154392));
#52849=CARTESIAN_POINT('Ctrl Pts',(-68.0024318752322,-4.14502897846688,
-2.1115161085075));
#52850=CARTESIAN_POINT('Ctrl Pts',(-67.8035583435347,-0.464421245542407,
-4.62861517254413));
#52851=CARTESIAN_POINT('Ctrl Pts',(-67.6046848118373,3.64289768136986,-2.89293311223871));
#52852=CARTESIAN_POINT('Ctrl Pts',(-67.4058112801398,4.40311473877763,1.50078183157187));
#52853=CARTESIAN_POINT('Ctrl Pts',(-67.2069377484423,1.11774093340179,4.51557534702004));
#52854=CARTESIAN_POINT('Ctrl Pts',(-67.008064216745,-3.19461553661043,3.38144896191918));
#52855=CARTESIAN_POINT('Ctrl Pts',(-66.8091906850474,-4.5717526921685,-0.859559672429393));
#52856=CARTESIAN_POINT('Ctrl Pts',(-66.6103171533501,-1.74835408710783,
-4.31080311483954));
#52857=CARTESIAN_POINT('Ctrl Pts',(-66.4114436216526,2.68143584303501,-3.80127180408139));
#52858=CARTESIAN_POINT('Ctrl Pts',(-66.212570089955,4.64751701487864,0.200875845313876));
#52859=CARTESIAN_POINT('Ctrl Pts',(-66.0136965582578,2.34345001083256,4.0184583555819));
#52860=CARTESIAN_POINT('Ctrl Pts',(-65.81482302656,-2.11378367490808,4.14387307775092));
#52861=CARTESIAN_POINT('Ctrl Pts',(-65.6159494948629,-4.62886857996913,
0.461888707581565));
#52862=CARTESIAN_POINT('Ctrl Pts',(-65.4170759631652,-2.89093952942574,
-3.64447995549718));
#52863=CARTESIAN_POINT('Ctrl Pts',(-65.2182024314679,1.50319069664089,-4.40229295235441));
#52864=CARTESIAN_POINT('Ctrl Pts',(-65.0193288997703,4.51618622417364,-1.11527014548103));
#52865=CARTESIAN_POINT('Ctrl Pts',(-64.820455368073,3.37970057597434,3.19646516101393));
#52866=CARTESIAN_POINT('Ctrl Pts',(-64.6215818363755,-0.862060900876653,
4.57128171435502));
#52867=CARTESIAN_POINT('Ctrl Pts',(-64.422708304678,-4.31175905195616,1.74599524245944));
#52868=CARTESIAN_POINT('Ctrl Pts',(-64.2238347729806,-3.79980413288183,
-2.68351524321201));
#52869=CARTESIAN_POINT('Ctrl Pts',(-64.0249612412831,0.203418625517942,
-4.64740641343205));
#52870=CARTESIAN_POINT('Ctrl Pts',(-63.8260877095857,4.01973993311795,-2.3412510285986));
#52871=CARTESIAN_POINT('Ctrl Pts',(-63.6272141778882,4.14271593654741,2.11605060853774));
#52872=CARTESIAN_POINT('Ctrl Pts',(-63.4283406461908,0.459356031352204,
4.62912060172093));
#52873=CARTESIAN_POINT('Ctrl Pts',(-63.2294671144932,-3.64606113863258,
2.88894508119666));
#52874=CARTESIAN_POINT('Ctrl Pts',(-63.0305935827959,-4.40146984808443,
-1.50559911172283));
#52875=CARTESIAN_POINT('Ctrl Pts',(-62.8317200510983,-1.112799023699,-4.51679574938602));
#52876=CARTESIAN_POINT('Ctrl Pts',(-62.632846519401,3.19831382854077,-3.37795117830051));
#52877=CARTESIAN_POINT('Ctrl Pts',(-62.4339729877035,4.57080936810724,0.864561871261937));
#52878=CARTESIAN_POINT('Ctrl Pts',(-62.235099456006,1.74363587513935,4.31271369832778));
#52879=CARTESIAN_POINT('Ctrl Pts',(-62.0362259243087,-2.68559384006632,
3.79833532419333));
#52880=CARTESIAN_POINT('Ctrl Pts',(-61.837352392611,-4.64729442076289,-0.205961344827695));
#52881=CARTESIAN_POINT('Ctrl Pts',(-61.6384788609138,-2.33905134550033,
-4.02102030732626));
#52882=CARTESIAN_POINT('Ctrl Pts',(-61.4396053292161,2.11831690871786,-4.14155755520273));
#52883=CARTESIAN_POINT('Ctrl Pts',(-61.2407317975188,4.62937123772409,-0.456823217612489));
#52884=CARTESIAN_POINT('Ctrl Pts',(-61.0418582658213,2.88694976814851,3.64764123030272));
#52885=CARTESIAN_POINT('Ctrl Pts',(-60.8429847341239,-1.50800707609672,
4.40064542621412));
#52886=CARTESIAN_POINT('Ctrl Pts',(-60.6441112024264,-4.51740392247471,
1.11032756879543));
#52887=CARTESIAN_POINT('Ctrl Pts',(-60.445237670729,-3.37620076942136,-3.20016153863765));
#52888=CARTESIAN_POINT('Ctrl Pts',(-60.2463641390314,0.867062582836786,
-4.57033565356654));
#52889=CARTESIAN_POINT('Ctrl Pts',(-60.0474906073341,4.31366705366866,-1.74127598585364));
#52890=CARTESIAN_POINT('Ctrl Pts',(-59.8486170756365,3.79686537845552,2.68767163297581));
#52891=CARTESIAN_POINT('Ctrl Pts',(-59.6497435439392,-0.208504002482106,
4.64718103690463));
#52892=CARTESIAN_POINT('Ctrl Pts',(-59.4508700122417,-4.02229947782363,
2.3368509621961));
#52893=CARTESIAN_POINT('Ctrl Pts',(-59.2519964805442,-4.14039793406358,
-2.12058257477011));
#52894=CARTESIAN_POINT('Ctrl Pts',(-59.0531229488468,-0.45429026712059,
-4.62962048790353));
#52895=CARTESIAN_POINT('Ctrl Pts',(-58.8542494171492,3.64922023003459,-2.88495359087861));
#52896=CARTESIAN_POINT('Ctrl Pts',(-58.655375885452,4.39981968699025,1.51041458904172));
#52897=CARTESIAN_POINT('Ctrl Pts',(-58.4565023537543,1.10785578151018,4.51801074325765));
#52898=CARTESIAN_POINT('Ctrl Pts',(-58.2576288220571,-3.20200829075135,
3.37444934986091));
#52899=CARTESIAN_POINT('Ctrl Pts',(-58.0587552903594,-4.56986057087472,
-0.869563034852338));
#52900=CARTESIAN_POINT('Ctrl Pts',(-57.8598817586621,-1.73891557530902,
-4.31461911769333));
#52901=CARTESIAN_POINT('Ctrl Pts',(-57.6610082269646,2.68974862131826,-3.79539429610858));
#52902=CARTESIAN_POINT('Ctrl Pts',(-57.4621346952672,4.64706626189126,0.211046597719749));
#52903=CARTESIAN_POINT('Ctrl Pts',(-57.2632611635697,2.33464987934486,4.02357744422698));
#52904=CARTESIAN_POINT('Ctrl Pts',(-57.0643876318722,-2.12284760601617,
4.13923707347725));
#52905=CARTESIAN_POINT('Ctrl Pts',(-56.8655141001748,-4.62986835218477,
0.451757180634654));
#52906=CARTESIAN_POINT('Ctrl Pts',(-56.6666405684773,-2.88295654998432,
-3.6507981373556));
#52907=CARTESIAN_POINT('Ctrl Pts',(-56.4677670367799,1.51282164983718,-4.39899263065995));
#52908=CARTESIAN_POINT('Ctrl Pts',(-56.2688935050824,4.51861621155319,-1.10538366258318));
#52909=CARTESIAN_POINT('Ctrl Pts',(-56.070019973385,3.37269692014345,3.20385408432906));
#52910=CARTESIAN_POINT('Ctrl Pts',(-55.8711464416876,-0.872063226560181,
4.56938412017402));
#52911=CARTESIAN_POINT('Ctrl Pts',(-55.67227290999,-4.31556989011681,1.736554644212));
#52912=CARTESIAN_POINT('Ctrl Pts',(-55.4733993782926,-3.79392207759281,
-2.69182480447203));
#52913=CARTESIAN_POINT('Ctrl Pts',(-55.2745258465952,0.213589129779611,
-4.64695009575711));
#52914=CARTESIAN_POINT('Ctrl Pts',(-55.0756523148977,4.02485420615382,-2.33244809760538));
#52915=CARTESIAN_POINT('Ctrl Pts',(-54.8767787832003,4.13807497379115,2.1251120017779));
#52916=CARTESIAN_POINT('Ctrl Pts',(-54.6779052515027,0.449223958913303,
4.63011483049344));
#52917=CARTESIAN_POINT('Ctrl Pts',(-54.4790317198054,-3.65237495179322,
2.88095864606385));
#52918=CARTESIAN_POINT('Ctrl Pts',(-54.2801581881078,-4.39816425747094,
-1.51522825776243));
#52919=CARTESIAN_POINT('Ctrl Pts',(-54.0812846564105,-1.10291121275446,
-4.51922032718007));
#52920=CARTESIAN_POINT('Ctrl Pts',(-53.8824111247129,3.20569891881823,-3.37094348079357));
#52921=CARTESIAN_POINT('Ctrl Pts',(-53.6835375930156,4.56890630160706,0.874563157211865));
#52922=CARTESIAN_POINT('Ctrl Pts',(-53.4846640613179,1.73419319326931,4.31651937065449));
#52923=CARTESIAN_POINT('Ctrl Pts',(-53.2857905296208,-2.6939001818156,3.79244872334894));
#52924=CARTESIAN_POINT('Ctrl Pts',(-53.086916997923,-4.64683253853698,-0.216131597900584));
#52925=CARTESIAN_POINT('Ctrl Pts',(-52.8880434662258,-2.33024561763677,
-4.02612976322195));
#52926=CARTESIAN_POINT('Ctrl Pts',(-52.6891699345282,2.12737576137752,-4.13691163535318));
#52927=CARTESIAN_POINT('Ctrl Pts',(-52.4902964028309,4.63035992275584,-0.446690602714689));
#52928=CARTESIAN_POINT('Ctrl Pts',(-52.2914228711333,2.87895987971509,3.65395067287553));
#52929=CARTESIAN_POINT('Ctrl Pts',(-52.0925493394359,-1.5176344120971,4.39733456767112));
#52930=CARTESIAN_POINT('Ctrl Pts',(-51.8936758077385,-4.51982308995746,
1.10043843276417));
#52931=CARTESIAN_POINT('Ctrl Pts',(-51.6948022760409,-3.36918903233618,
-3.20754279366662));
#52932=CARTESIAN_POINT('Ctrl Pts',(-51.4959287443436,0.877062826059023,
-4.56842711531687));
#52933=CARTESIAN_POINT('Ctrl Pts',(-51.2970552126461,4.31746755902214,-1.73183122318787));
#52934=CARTESIAN_POINT('Ctrl Pts',(-51.0981816809486,3.790974233818,2.69597475272769));
#52935=CARTESIAN_POINT('Ctrl Pts',(-50.8993081492512,-0.21867400132156,
4.64671359026604));
#52936=CARTESIAN_POINT('Ctrl Pts',(-50.7004346175536,-4.02740411504953,
2.32804244009837));
#52937=CARTESIAN_POINT('Ctrl Pts',(-50.5015610858563,-4.13574705851158,
-2.12963888413737));
#52938=CARTESIAN_POINT('Ctrl Pts',(-50.3026875541588,-0.444157112797176,
-4.63060362889859));
#52939=CARTESIAN_POINT('Ctrl Pts',(-50.1038140224614,3.6555253001308,-2.87696025153637));
#52940=CARTESIAN_POINT('Ctrl Pts',(-49.9049404907639,4.39650356150887,1.52004011212088));
#52941=CARTESIAN_POINT('Ctrl Pts',(-49.7060669590665,1.09796532335256,4.52042449970491));
#52942=CARTESIAN_POINT('Ctrl Pts',(-49.507193427369,-3.20938570832225,3.36743357529647));
#52943=CARTESIAN_POINT('Ctrl Pts',(-49.3083198956715,-4.56794656144691,
-0.879562232353367));
#52944=CARTESIAN_POINT('Ctrl Pts',(-49.1094463639741,-1.72946873467476,
-4.31841445493593));
#52945=CARTESIAN_POINT('Ctrl Pts',(-48.9105728322766,2.69804851658728,-3.78949860944139));
#52946=CARTESIAN_POINT('Ctrl Pts',(-48.7116993005792,4.6465932509799,0.221216339281466));
#52947=CARTESIAN_POINT('Ctrl Pts',(-48.5128257688817,2.3258385656497,4.02867726125506));
#52948=CARTESIAN_POINT('Ctrl Pts',(-48.3139522371842,-2.13190136937999,
4.13458124361499));
#52949=CARTESIAN_POINT('Ctrl Pts',(-48.1150787054868,-4.63084594884872,
0.441623489919174));
#52950=CARTESIAN_POINT('Ctrl Pts',(-47.9162051737893,-2.87495976212631,
-3.65709883308768));
#52951=CARTESIAN_POINT('Ctrl Pts',(-47.7173316420919,1.52244535711364,-4.39567123923295));
#52952=CARTESIAN_POINT('Ctrl Pts',(-47.5184581103945,4.52102455624239,-1.09549188525994));
#52953=CARTESIAN_POINT('Ctrl Pts',(-47.319584578697,3.36567711019996,3.21122766223342));
#52954=CARTESIAN_POINT('Ctrl Pts',(-47.1207110469995,-0.882061375346694,
4.56746464014102));
#52955=CARTESIAN_POINT('Ctrl Pts',(-46.9218375153021,-4.31936005811238,
1.72710572843718));
#52956=CARTESIAN_POINT('Ctrl Pts',(-46.7229639836046,-3.78802185066086,
-2.70012147277357));
#52957=CARTESIAN_POINT('Ctrl Pts',(-46.5240904519073,0.223758611019232,
-4.6464715207146));
#52958=CARTESIAN_POINT('Ctrl Pts',(-46.3252169202096,4.02994920145744,-2.3236339949505));
#52959=CARTESIAN_POINT('Ctrl Pts',(-46.1263433885124,4.13341419101237,2.13416321642806));
#52960=CARTESIAN_POINT('Ctrl Pts',(-45.9274698568147,0.439089734839147,
4.63108688253373));
#52961=CARTESIAN_POINT('Ctrl Pts',(-45.7285963251174,-3.65867127127512,
2.87295841208375));
#52962=CARTESIAN_POINT('Ctrl Pts',(-45.5297227934199,-4.39483760109253,
-1.52485014635534));
#52963=CARTESIAN_POINT('Ctrl Pts',(-45.3308492617225,-1.09301811922677,
-4.52162325939027));
#52964=CARTESIAN_POINT('Ctrl Pts',(-45.131975730025,3.21306865484875,-3.36391963757244));
#52965=CARTESIAN_POINT('Ctrl Pts',(-44.9331021983275,4.56698135154348,0.88456025429087));
#52966=CARTESIAN_POINT('Ctrl Pts',(-44.7342286666301,1.72474220518251,4.32030436826842));
#52967=CARTESIAN_POINT('Ctrl Pts',(-44.5353551349326,-2.70219362066602,
3.78654395791848));
#52968=CARTESIAN_POINT('Ctrl Pts',(-44.3364816032352,-4.64634839950656,
-0.22630081577383));
#52969=CARTESIAN_POINT('Ctrl Pts',(-44.1376080715377,-2.32142872866073,
-4.03121993527588));
#52970=CARTESIAN_POINT('Ctrl Pts',(-43.9387345398403,2.13642442460452,-4.13224590105312));
#52971=CARTESIAN_POINT('Ctrl Pts',(-43.7398610081428,4.63132642988146,-0.43655584831557));
#52972=CARTESIAN_POINT('Ctrl Pts',(-43.5409874764454,2.8709562020078,3.66024261422239));
#52973=CARTESIAN_POINT('Ctrl Pts',(-43.3421139447479,-1.52725447912609,
4.39400264733715));
#52974=CARTESIAN_POINT('Ctrl Pts',(-43.1432404130505,-4.52222060896932,
1.09054402599357));
#52975=CARTESIAN_POINT('Ctrl Pts',(-42.944366881353,-3.36216115794003,-3.21490868561712));
#52976=CARTESIAN_POINT('Ctrl Pts',(-42.7454933496555,0.887058868437845,
-4.56649669579896));
#52977=CARTESIAN_POINT('Ctrl Pts',(-42.5466198179581,4.32124738512139,-1.72237816561829));
#52978=CARTESIAN_POINT('Ctrl Pts',(-42.3477462862606,3.78506493165666,2.70426495964431));
#52979=CARTESIAN_POINT('Ctrl Pts',(-42.1488727545632,-0.228842952784232,
4.64622388739265));
#52980=CARTESIAN_POINT('Ctrl Pts',(-41.9499992228657,-4.03248946233,2.31922276744054));
#52981=CARTESIAN_POINT('Ctrl Pts',(-41.7511256911683,-4.13107637408695,
-2.13868499323244));
#52982=CARTESIAN_POINT('Ctrl Pts',(-41.5522521594709,-0.434021831106983,
-4.63156459082021));
#52983=CARTESIAN_POINT('Ctrl Pts',(-41.3533786277734,3.66181286145911,-2.86895313249785));
#52984=CARTESIAN_POINT('Ctrl Pts',(-41.1545050960759,4.39316637821677,1.52965835470616));
#52985=CARTESIAN_POINT('Ctrl Pts',(-40.9556315643785,1.08806960630097,4.52281660480072));
#52986=CARTESIAN_POINT('Ctrl Pts',(-40.756758032681,-3.21674775398771,3.36040167182914));
#52987=CARTESIAN_POINT('Ctrl Pts',(-40.5578845009836,-4.56601067305254,
-0.889557217039647));
#52988=CARTESIAN_POINT('Ctrl Pts',(-40.3590109692861,-1.72001361045221,
-4.32218910838897));
#52989=CARTESIAN_POINT('Ctrl Pts',(-40.1601374375886,2.70633548908839,-3.78358477231815));
#52990=CARTESIAN_POINT('Ctrl Pts',(-39.9612639058912,4.64609798441014,0.231385021289438));
#52991=CARTESIAN_POINT('Ctrl Pts',(-39.7623903741937,2.31701611195028,4.03375778223976));
#52992=CARTESIAN_POINT('Ctrl Pts',(-39.5635168424963,-2.14094492163513,
4.12990561046398));
#52993=CARTESIAN_POINT('Ctrl Pts',(-39.3646433107988,-4.6318013652787,0.431487683971952));
#52994=CARTESIAN_POINT('Ctrl Pts',(-39.1657697791014,-2.86694920415351,
-3.66338201251523));
#52995=CARTESIAN_POINT('Ctrl Pts',(-38.9668962474039,1.53206177237593,-4.39232879398173));
#52996=CARTESIAN_POINT('Ctrl Pts',(-38.7680227157065,4.52341124670607,-1.08559486088971));
#52997=CARTESIAN_POINT('Ctrl Pts',(-38.569149184009,3.35864117976647,3.21858585941));
#52998=CARTESIAN_POINT('Ctrl Pts',(-38.3702756523116,-0.892055299348385,
4.56552328344972));
#52999=CARTESIAN_POINT('Ctrl Pts',(-38.1714021206141,-4.32312953778925,
1.7176485403921));
#53000=CARTESIAN_POINT('Ctrl Pts',(-37.9725285889166,-3.78210348034605,
-2.70840520837842));
#53001=CARTESIAN_POINT('Ctrl Pts',(-37.7736550572192,0.233927020528463,
-4.64597069059672));
#53002=CARTESIAN_POINT('Ctrl Pts',(-37.5747815255217,4.03502489462548,-2.31480876285055));
#53003=CARTESIAN_POINT('Ctrl Pts',(-37.3759079938243,4.12873361053465,2.14320420913606));
#53004=CARTESIAN_POINT('Ctrl Pts',(-37.1770344621268,0.428953407669176,
4.63203675318597));
#53005=CARTESIAN_POINT('Ctrl Pts',(-36.9781609304295,-3.66495006692095,
2.86494441757476));
#53006=CARTESIAN_POINT('Ctrl Pts',(-36.7792873987319,-4.39148989488282,
-1.53446473141587));
#53007=CARTESIAN_POINT('Ctrl Pts',(-36.5804138670346,-1.0831197905006,-4.52400453450735));
#53008=CARTESIAN_POINT('Ctrl Pts',(-36.381540335337,3.22042300133372,-3.35687968227903));
#53009=CARTESIAN_POINT('Ctrl Pts',(-36.1826668036397,4.5650345271364,0.894553114616239));
#53010=CARTESIAN_POINT('Ctrl Pts',(-35.983793271942,1.71528295614595,4.32406867304074));
#53011=CARTESIAN_POINT('Ctrl Pts',(-35.7849197402448,-2.71047411689484,
3.78062105618378));
#53012=CARTESIAN_POINT('Ctrl Pts',(-35.5860462085471,-4.64584200599049,
-0.236468949740354));
#53013=CARTESIAN_POINT('Ctrl Pts',(-35.3871726768498,-2.3126007208021,-4.03629079910785));
#53014=CARTESIAN_POINT('Ctrl Pts',(-35.1882991451523,2.1454628550589,-4.12756037464984));
#53015=CARTESIAN_POINT('Ctrl Pts',(-34.9894256134549,4.63227075447169,-0.426419002957134));
#53016=CARTESIAN_POINT('Ctrl Pts',(-34.7905520817573,2.86293877336157,3.66651702420699));
#53017=CARTESIAN_POINT('Ctrl Pts',(-34.59167855006,-1.53686723110675,4.39064968117103));
#53018=CARTESIAN_POINT('Ctrl Pts',(-34.3928050183625,-4.52459646802695,
1.08064439587459));
#53019=CARTESIAN_POINT('Ctrl Pts',(-34.1939314866651,-3.35511717989414,
-3.22225917920893));
#53020=CARTESIAN_POINT('Ctrl Pts',(-33.9950579549676,0.897050662095486,
-4.56454440425889));
#53021=CARTESIAN_POINT('Ctrl Pts',(-33.7961844232701,4.32500651386226,-1.71291685842193));
#53022=CARTESIAN_POINT('Ctrl Pts',(-33.5973108915727,3.77913750027513,2.7125422140183));
#53023=CARTESIAN_POINT('Ctrl Pts',(-33.3984373598752,-0.239010808164181,
4.64571193062998));
#53024=CARTESIAN_POINT('Ctrl Pts',(-33.1995638281778,-4.0375554953079,2.31039198646595));
#53025=CARTESIAN_POINT('Ctrl Pts',(-33.0006902964803,-4.12638590316076,
-2.14772085872751));
#53026=CARTESIAN_POINT('Ctrl Pts',(-32.8018167647829,-0.423884470594582,
-4.63250336906573));
#53027=CARTESIAN_POINT('Ctrl Pts',(-32.6029432330854,3.66808288390419,-2.86093227211442));
#53028=CARTESIAN_POINT('Ctrl Pts',(-32.4040697013879,4.38980815309797,1.53926927072932));
#53029=CARTESIAN_POINT('Ctrl Pts',(-32.2051961696905,1.07816867775268,4.52518704708768));
#53030=CARTESIAN_POINT('Ctrl Pts',(-32.006322637993,-3.22409439248597,3.35335367313942));
#53031=CARTESIAN_POINT('Ctrl Pts',(-31.8074491062956,-4.56405291496391,
-0.899547941038473));
#53032=CARTESIAN_POINT('Ctrl Pts',(-31.6085755745981,-1.71055024792833,
-4.3259430599731));
#53033=CARTESIAN_POINT('Ctrl Pts',(-31.4097020429007,2.71460949912971,-3.7776528130642));
#53034=CARTESIAN_POINT('Ctrl Pts',(-31.2108285112032,4.64558046455413,0.241552595039009));
#53035=CARTESIAN_POINT('Ctrl Pts',(-31.0119549795058,2.30818256050327,4.03881898284705));
#53036=CARTESIAN_POINT('Ctrl Pts',(-30.8130814478083,-2.14997821946597,
4.12521019641897));
#53037=CARTESIAN_POINT('Ctrl Pts',(-30.6142079161108,-4.63273459689848,
0.421349811340259));
#53038=CARTESIAN_POINT('Ctrl Pts',(-30.4153343844134,-2.85892491443397,
-3.66964764554383));
#53039=CARTESIAN_POINT('Ctrl Pts',(-30.216460852716,1.54167084956452,-4.38896531091555));
#53040=CARTESIAN_POINT('Ctrl Pts',(-30.0175873210185,4.52577627151276,-1.07569263687598));
#53041=CARTESIAN_POINT('Ctrl Pts',(-29.818713789321,3.35158916254276,3.22592864061543));
#53042=CARTESIAN_POINT('Ctrl Pts',(-29.6198402576236,-0.902044950697624,
4.56356005939858));
#53043=CARTESIAN_POINT('Ctrl Pts',(-29.4209667259261,-4.32687831109287,
1.70818312537359));
#53044=CARTESIAN_POINT('Ctrl Pts',(-29.2220931942287,-3.77616699499543,
-2.71667597161021));
#53045=CARTESIAN_POINT('Ctrl Pts',(-29.0232196625312,0.244094309603952,
-4.64544760780229));
#53046=CARTESIAN_POINT('Ctrl Pts',(-28.8243461308338,4.04008126134707,-2.30597244357546));
#53047=CARTESIAN_POINT('Ctrl Pts',(-28.6254725991363,4.12403325477644,2.15223493659848));
#53048=CARTESIAN_POINT('Ctrl Pts',(-28.4265990674389,0.418815025952924,
4.63296443790072));
#53049=CARTESIAN_POINT('Ctrl Pts',(-28.2277255357414,-3.67121130865748,
2.85691670092113));
#53050=CARTESIAN_POINT('Ctrl Pts',(-28.0288520040439,-4.38812115487607,
-1.54407196689343));
#53051=CARTESIAN_POINT('Ctrl Pts',(-27.8299784723465,-1.07321627398572,
-4.52636414112578));
#53052=CARTESIAN_POINT('Ctrl Pts',(-27.6311049406491,3.22776192304825,-3.3498236486324));
#53053=CARTESIAN_POINT('Ctrl Pts',(-27.4322314089516,4.56306583771046,0.904541690325447));
#53054=CARTESIAN_POINT('Ctrl Pts',(-27.2333578772542,1.70581549146635,4.32781226694163));
#53055=CARTESIAN_POINT('Ctrl Pts',(-27.0344843455567,-2.7187416308412,3.77468004651361));
#53056=CARTESIAN_POINT('Ctrl Pts',(-26.8356108138592,-4.64531336041423,
-0.246635951098138));
#53057=CARTESIAN_POINT('Ctrl Pts',(-26.6367372821618,-2.30376163634415,
-4.04134233043008));
#53058=CARTESIAN_POINT('Ctrl Pts',(-26.4378637504643,2.15449100944954,-4.12285507858549));
#53059=CARTESIAN_POINT('Ctrl Pts',(-26.2389902187669,4.63319289200362,-0.416280115191373));
#53060=CARTESIAN_POINT('Ctrl Pts',(-26.0401166870694,2.85490763217707,3.67277387277706));
#53061=CARTESIAN_POINT('Ctrl Pts',(-25.841243155372,-1.54647262199725,4.38727568523224));
#53062=CARTESIAN_POINT('Ctrl Pts',(-25.6423696236745,-4.52695065575077,
1.07073958982321));
#53063=CARTESIAN_POINT('Ctrl Pts',(-25.4434960919771,-3.34805713193684,
-3.22959423923561));
#53064=CARTESIAN_POINT('Ctrl Pts',(-25.2446225602796,0.907038159174535,
-4.56257025004749));
#53065=CARTESIAN_POINT('Ctrl Pts',(-25.0457490285821,4.32874492723977,-1.70344734691535));
#53066=CARTESIAN_POINT('Ctrl Pts',(-24.8468754968847,3.77319196806387,2.72080647620431));
#53067=CARTESIAN_POINT('Ctrl Pts',(-24.6480019651872,-0.249177518760706,
4.64517772243015));
#53068=CARTESIAN_POINT('Ctrl Pts',(-24.4491284334898,-4.04260218971858,
2.30155013947114));
#53069=CARTESIAN_POINT('Ctrl Pts',(-24.2502549017923,-4.12167566819881,
-2.15674643734374));
#53070=CARTESIAN_POINT('Ctrl Pts',(-24.0513813700949,-0.41374507981445,
-4.63341995913882));
#53071=CARTESIAN_POINT('Ctrl Pts',(-23.8525078383975,3.6743353374348,-2.8528977088032));
#53072=CARTESIAN_POINT('Ctrl Pts',(-23.6536343067,4.38642890223714,1.54887281415735));
#53073=CARTESIAN_POINT('Ctrl Pts',(-23.4547607750026,1.06826258512985,4.52753581521215));
#53074=CARTESIAN_POINT('Ctrl Pts',(-23.255887243305,-3.23142558862902,3.34628961298491));
#53075=CARTESIAN_POINT('Ctrl Pts',(-23.0570137116077,-4.56207329655801,
-0.909534356497557));
#53076=CARTESIAN_POINT('Ctrl Pts',(-22.8581401799101,-1.70107869242952,
-4.32967629170811));
#53077=CARTESIAN_POINT('Ctrl Pts',(-22.6592666482128,2.72287050708144,-3.77170276009168));
#53078=CARTESIAN_POINT('Ctrl Pts',(-22.4603931165152,4.64504069389063,0.251719011830838));
#53079=CARTESIAN_POINT('Ctrl Pts',(-22.2615195848178,2.29933795361846,4.04386083883543));
#53080=CARTESIAN_POINT('Ctrl Pts',(-22.0626460531203,-2.15900121960593,
4.12049502396947));
#53081=CARTESIAN_POINT('Ctrl Pts',(-21.8637725214229,-4.63364563923833,
0.411209920581015));
#53082=CARTESIAN_POINT('Ctrl Pts',(-21.6648989897254,-2.85088693140123,
-3.67589570216326));
#53083=CARTESIAN_POINT('Ctrl Pts',(-21.466025458028,1.5512725426552,-4.38558080614428));
#53084=CARTESIAN_POINT('Ctrl Pts',(-21.2671519263305,4.52811961933476,-1.06578526064715));
#53085=CARTESIAN_POINT('Ctrl Pts',(-21.0682783946331,3.3445210923057,3.23325597068022));
#53086=CARTESIAN_POINT('Ctrl Pts',(-20.8694048629356,-0.912030281547263,
4.5615749773908));
#53087=CARTESIAN_POINT('Ctrl Pts',(-20.6705313312382,-4.33060636006784,
1.69870952871791));
#53088=CARTESIAN_POINT('Ctrl Pts',(-20.4716577995407,-3.77021242304282,
-2.72493372285468));
#53089=CARTESIAN_POINT('Ctrl Pts',(-20.2727842678433,0.254260429547719,
-4.64490227483671));
#53090=CARTESIAN_POINT('Ctrl Pts',(-20.0739107361458,4.04511827740384,-2.29712507944832));
#53091=CARTESIAN_POINT('Ctrl Pts',(-19.8750372044484,4.1193131462509,2.16125535556112));
#53092=CARTESIAN_POINT('Ctrl Pts',(-19.6761636727509,0.408674638249995,
4.6338699322346));
#53093=CARTESIAN_POINT('Ctrl Pts',(-19.4772901410535,-3.67745496649536,
2.84887530057306));
#53094=CARTESIAN_POINT('Ctrl Pts',(-19.278416609356,-4.38473139720753,-1.55367180677245));
#53095=CARTESIAN_POINT('Ctrl Pts',(-19.0795430776586,-1.0633076171167,-4.52870206794382));
#53096=CARTESIAN_POINT('Ctrl Pts',(-18.8806695459611,3.23508538484131,-3.34275157042865));
#53097=CARTESIAN_POINT('Ctrl Pts',(-18.6817960142637,4.56107529269504,0.914525933576483));
#53098=CARTESIAN_POINT('Ctrl Pts',(-18.4829224825662,1.69633985648975,4.33153513204054));
#53099=CARTESIAN_POINT('Ctrl Pts',(-18.2840489508687,-2.72699612290642,
3.76872095736344));
#53100=CARTESIAN_POINT('Ctrl Pts',(-18.0851754191713,-4.64476246530983,
-0.256801771150557));
#53101=CARTESIAN_POINT('Ctrl Pts',(-17.8863018874738,-2.29491151762317,
-4.0463745050474));
#53102=CARTESIAN_POINT('Ctrl Pts',(-17.6874283557763,2.16350884453443,-4.11813003539688));
#53103=CARTESIAN_POINT('Ctrl Pts',(-17.4885548240789,4.63409283806047,-0.406139233580442));
#53104=CARTESIAN_POINT('Ctrl Pts',(-17.2896812923815,2.846862816921,3.6790131299643));
#53105=CARTESIAN_POINT('Ctrl Pts',(-17.090807760684,-1.55607060579087,4.38388067568116));
#53106=CARTESIAN_POINT('Ctrl Pts',(-16.8919342289866,-4.52928316086499,
1.06082965528021));
#53107=CARTESIAN_POINT('Ctrl Pts',(-16.6930606972891,-3.34098104788346,
-3.23691383056463));
#53108=CARTESIAN_POINT('Ctrl Pts',(-16.4941871655917,0.917021311838145,
-4.5605742426203));
#53109=CARTESIAN_POINT('Ctrl Pts',(-16.2953136338942,4.33246260734816,-1.69396967645442));
#53110=CARTESIAN_POINT('Ctrl Pts',(-16.0964401021967,3.76722836350003,2.72905770661926));
#53111=CARTESIAN_POINT('Ctrl Pts',(-15.8975665704993,-0.259343035878605,
4.64462126535182));
#53112=CARTESIAN_POINT('Ctrl Pts',(-15.6986930388018,-4.04762952139003,
2.29269726880566));
#53113=CARTESIAN_POINT('Ctrl Pts',(-15.4998195071044,-4.11694569176161,
-2.16576168585147));
#53114=CARTESIAN_POINT('Ctrl Pts',(-15.3009459754069,-0.40360370733112,
-4.63431435664923));
#53115=CARTESIAN_POINT('Ctrl Pts',(-15.1020724437095,3.68057019210366,-2.84484948104731));
#53116=CARTESIAN_POINT('Ctrl Pts',(-14.903198912012,4.38302864181985,1.55846893899236));
#53117=CARTESIAN_POINT('Ctrl Pts',(-14.7043253803146,1.05835137587945,4.5298628979243));
#53118=CARTESIAN_POINT('Ctrl Pts',(-14.5054518486171,-3.23874130730283,
3.33920952520015));
#53119=CARTESIAN_POINT('Ctrl Pts',(-14.3065783169196,-4.56007182731658,
-0.919516415585235));
#53120=CARTESIAN_POINT('Ctrl Pts',(-14.1077047852222,-1.69159898932142,
-4.33338878571307));
#53121=CARTESIAN_POINT('Ctrl Pts',(-13.9088312535247,2.73111847337605,-3.76573464189939));
#53122=CARTESIAN_POINT('Ctrl Pts',(-13.7099577218273,4.64447867500497,0.261884222971118));
#53123=CARTESIAN_POINT('Ctrl Pts',(-13.5110841901299,2.29048233365862,4.04888332605607));
#53124=CARTESIAN_POINT('Ctrl Pts',(-13.3122106584324,-2.16801387883773,
4.1157601156996));
#53125=CARTESIAN_POINT('Ctrl Pts',(-13.1133371267349,-4.63453448793457,
0.401068060261169));
#53126=CARTESIAN_POINT('Ctrl Pts',(-12.9144635950375,-2.84283529355476,
-3.68212615244732));
#53127=CARTESIAN_POINT('Ctrl Pts',(-12.7155900633401,1.56086680565895,-4.38217529587864));
#53128=CARTESIAN_POINT('Ctrl Pts',(-12.5167165316425,4.53044127894822,-1.05587277965632));
#53129=CARTESIAN_POINT('Ctrl Pts',(-12.3178429999451,3.33743700290902,3.24056781450885));
#53130=CARTESIAN_POINT('Ctrl Pts',(-12.1189694682477,-0.922011244070831,
4.55956804693427));
#53131=CARTESIAN_POINT('Ctrl Pts',(-11.9200959365502,-4.33431366685802,
1.68922779580046));
#53132=CARTESIAN_POINT('Ctrl Pts',(-11.7212224048528,-3.76423979300867,
-2.73317842255992));
#53133=CARTESIAN_POINT('Ctrl Pts',(-11.5223488731553,0.264425331667373,
-4.64433469431195));
#53134=CARTESIAN_POINT('Ctrl Pts',(-11.3234753414579,4.05013591867016,-2.2882667128451));
#53135=CARTESIAN_POINT('Ctrl Pts',(-11.1246018097604,4.11457330756578,2.17026542281901));
#53136=CARTESIAN_POINT('Ctrl Pts',(-10.925728278063,0.398532293129632,4.63475323185059));
#53137=CARTESIAN_POINT('Ctrl Pts',(-10.7268547463655,-3.68368101052949,
2.84082025504633));
#53138=CARTESIAN_POINT('Ctrl Pts',(-10.5279812146681,-4.38132063811301,
-1.56326420507285));
#53139=CARTESIAN_POINT('Ctrl Pts',(-10.3291076829706,-1.05339386735279,
-4.53101830376359));
#53140=CARTESIAN_POINT('Ctrl Pts',(-10.1302341512731,3.24239335163591,-3.3356634815407));
#53141=CARTESIAN_POINT('Ctrl Pts',(-9.93136061957567,4.55906290162419,0.924505796548103));
#53142=CARTESIAN_POINT('Ctrl Pts',(-9.7324870878782,1.68685609660134,4.33523725050613));
#53143=CARTESIAN_POINT('Ctrl Pts',(-9.53361355618078,-2.73523755355419,
3.76274381727536));
#53144=CARTESIAN_POINT('Ctrl Pts',(-9.33474002448328,-4.64418932331583,
-0.266966361206601));
#53145=CARTESIAN_POINT('Ctrl Pts',(-9.13586649278587,-2.28605040702846,
-4.05138729885728));
#53146=CARTESIAN_POINT('Ctrl Pts',(-8.9369929610884,2.17251631712126,-4.1133852677155));
#53147=CARTESIAN_POINT('Ctrl Pts',(-8.73811942939097,4.63497058833175,-0.395996406695693));
#53148=CARTESIAN_POINT('Ctrl Pts',(-8.53924589769349,2.8388043661253,3.68523476588466));
#53149=CARTESIAN_POINT('Ctrl Pts',(-8.34037236599606,-1.56566113651624,
4.38046466877884));
#53150=CARTESIAN_POINT('Ctrl Pts',(-8.14149883429858,-4.53159397219767,
1.05091463971103));
#53151=CARTESIAN_POINT('Ctrl Pts',(-7.94262530260114,-3.33388896162619,
-3.24421791813743));
#53152=CARTESIAN_POINT('Ctrl Pts',(-7.74375177090367,0.927000072270143,
-4.55855639153756));
#53153=CARTESIAN_POINT('Ctrl Pts',(-7.54487823920623,4.33615953638097,-1.68448389243425));
#53154=CARTESIAN_POINT('Ctrl Pts',(-7.34600470750878,3.76124671514718,2.73729586574244));
#53155=CARTESIAN_POINT('Ctrl Pts',(-7.14713117581134,-0.269507310827875,
4.64404256206009));
#53156=CARTESIAN_POINT('Ctrl Pts',(-6.94825764411386,-4.05263746624359,
2.28383341687229));
#53157=CARTESIAN_POINT('Ctrl Pts',(-6.74938411241643,-4.11219599650301,
-2.17476656107136));
#53158=CARTESIAN_POINT('Ctrl Pts',(-6.55051058071893,-0.393460401720496,
-4.63518655731204));
#53159=CARTESIAN_POINT('Ctrl Pts',(-6.35163704902152,3.68678741805236,-2.83678762739698));
#53160=CARTESIAN_POINT('Ctrl Pts',(-6.15276351732402,4.37960738812384,1.56805759927625));
#53161=CARTESIAN_POINT('Ctrl Pts',(-5.9538899856266,1.04843509748853,4.53216828407051));
#53162=CARTESIAN_POINT('Ctrl Pts',(-5.75501645392912,-3.24604151349715,
3.33211344371086));
#53163=CARTESIAN_POINT('Ctrl Pts',(-5.5561429222317,-4.55804851676996,-0.929494070517982));
#53164=CARTESIAN_POINT('Ctrl Pts',(-5.35726939053425,-1.68211118411471,
-4.33708052415461));
#53165=CARTESIAN_POINT('Ctrl Pts',(-5.15839585883678,2.73935335870827,-3.75974848717027));
#53166=CARTESIAN_POINT('Ctrl Pts',(-4.95952232713934,4.64389441021169,0.272048179955862));
#53167=CARTESIAN_POINT('Ctrl Pts',(-4.76064879544187,2.28161574375186,4.05388642010502));
#53168=CARTESIAN_POINT('Ctrl Pts',(-4.56177526374442,-2.17701615533913,
4.11100549494485));
#53169=CARTESIAN_POINT('Ctrl Pts',(-4.36290173204695,-4.63540113618978,
0.39092427771653));
#53170=CARTESIAN_POINT('Ctrl Pts',(-4.16402820034951,-2.83477004425545,
-3.68833896421277));
#53171=CARTESIAN_POINT('Ctrl Pts',(-3.96515466865204,1.57045360167918,-4.3787488008511));
#53172=CARTESIAN_POINT('Ctrl Pts',(-3.76628113695459,4.53274122213237,-1.04595523303274));
#53173=CARTESIAN_POINT('Ctrl Pts',(-3.56740760525717,3.33033696057287,3.24786412131688));
#53174=CARTESIAN_POINT('Ctrl Pts',(-3.36853407355969,-0.931987851432297,
4.55753930740539));
#53175=CARTESIAN_POINT('Ctrl Pts',(-3.16966054186226,-4.33800009858357,
1.67973791583561));
#53176=CARTESIAN_POINT('Ctrl Pts',(-2.97078701016478,-3.7582493508756,-2.74140992511906));
#53177=CARTESIAN_POINT('Ctrl Pts',(-2.77191347846734,0.274589377725611,
-4.6437450693177));
#53178=CARTESIAN_POINT('Ctrl Pts',(-2.57303994676988,4.05513338610117,-2.27939700785305));
#53179=CARTESIAN_POINT('Ctrl Pts',(-2.37416641507242,4.10981522480361,2.1792643808313));
#53180=CARTESIAN_POINT('Ctrl Pts',(-2.17529288337496,0.388385276010726,
4.63561568142362));
#53181=CARTESIAN_POINT('Ctrl Pts',(-1.9764193516775,-3.68988419353248,2.8327490559136));
#53182=CARTESIAN_POINT('Ctrl Pts',(-1.77754581998008,-4.37789874545427,
-1.57284430658088));
#53183=CARTESIAN_POINT('Ctrl Pts',(-1.57867228828259,-1.04345647049151,
-4.53332191837153));
#53184=CARTESIAN_POINT('Ctrl Pts',(-1.37979875658517,3.24965066464255,-3.32854226935553));
#53185=CARTESIAN_POINT('Ctrl Pts',(-1.1809252248877,4.55709499515704,0.934448855132265));
#53186=CARTESIAN_POINT('Ctrl Pts',(-0.982051693190257,1.6772390282778,4.33897973856184));
#53187=CARTESIAN_POINT('Ctrl Pts',(-0.783178161492788,-2.7432294143621,
3.75663321416178));
#53188=CARTESIAN_POINT('Ctrl Pts',(-0.584304629795343,-4.64404053043935,
-0.276911636729995));
#53189=CARTESIAN_POINT('Ctrl Pts',(-0.385431098097881,-2.27633433757937,
-4.05679287690181));
#53190=CARTESIAN_POINT('Ctrl Pts',(-0.18655756640042,2.17991358653948,-4.10783847096312));
#53191=CARTESIAN_POINT('Ctrl Pts',(0.0123159652969969,4.63889703590742,
-0.38736179081203));
#53192=CARTESIAN_POINT('Ctrl Pts',(0.2111894969945,2.82452520683169,3.6945553743333));
#53193=CARTESIAN_POINT('Ctrl Pts',(0.343771851459442,-0.0987079820474816,
4.14442455744695));
#53194=CARTESIAN_POINT('Ctrl Pts',(0.410063028691923,-1.33182005907514,
3.70064107017218));
#53195=CARTESIAN_POINT('',(0.,3.89175630324273,-0.568086152067144));
#53196=CARTESIAN_POINT('Ctrl Pts',(-8.04911692853238E-15,3.89860680620593,
-0.567889413565848));
#53197=CARTESIAN_POINT('Ctrl Pts',(-1.07269636646957E-14,3.90357565560566,
-0.487072913846011));
#53198=CARTESIAN_POINT('Ctrl Pts',(2.32719976779923E-14,3.9058565072249,
-0.406193250504373));
#53199=CARTESIAN_POINT('Ctrl Pts',(1.50990331349021E-14,3.90537360502758,
-0.32534746124043));
#53200=CARTESIAN_POINT('Ctrl Pts',(2.76112838444297E-15,3.90464797577591,
-0.203865161326043));
#53201=CARTESIAN_POINT('Ctrl Pts',(-6.82244033398785E-15,3.89768417373717,
-0.0824584493220015));
#53202=CARTESIAN_POINT('Ctrl Pts',(-9.2148511043888E-15,3.88471463000325,
0.0384874957482827));
#53203=CARTESIAN_POINT('Ctrl Pts',(-1.06155140461537E-14,3.87712146937028,
0.109296616536635));
#53204=CARTESIAN_POINT('Ctrl Pts',(-8.57920104564936E-15,3.86746876710794,
0.179947588184905));
#53205=CARTESIAN_POINT('Ctrl Pts',(-5.38458166943201E-15,3.85579555749106,
0.250360153300933));
#53206=CARTESIAN_POINT('Ctrl Pts',(-2.93363335536299E-15,3.84683973832737,
0.304381473976933));
#53207=CARTESIAN_POINT('Ctrl Pts',(2.92444448707381E-14,3.83669450630869,
0.358262424434777));
#53208=CARTESIAN_POINT('Ctrl Pts',(3.66373598126302E-14,3.82537548919011,
0.411965518384648));
#53209=CARTESIAN_POINT('Ctrl Pts',(3.95702663936449E-14,3.82088502500127,
0.433270532564362));
#53210=CARTESIAN_POINT('Ctrl Pts',(2.77330594251881E-14,3.81620949621549,
0.454548537547267));
#53211=CARTESIAN_POINT('Ctrl Pts',(2.66453525910038E-14,3.81135385472659,
0.475780514671049));
#53212=CARTESIAN_POINT('Ctrl Pts',(2.04972267428747E-14,3.78390795293671,
0.595791590504276));
#53213=CARTESIAN_POINT('Ctrl Pts',(-4.54776054783641E-15,3.75068649423825,
0.714458464692085));
#53214=CARTESIAN_POINT('Ctrl Pts',(6.77236045021345E-15,3.71192731145421,
0.831378922517886));
#53215=CARTESIAN_POINT('Ctrl Pts',(1.66774663235071E-14,3.67801302651818,
0.933684323115462));
#53216=CARTESIAN_POINT('Ctrl Pts',(2.44821053095673E-14,3.63985784417228,
1.03465273289086));
#53217=CARTESIAN_POINT('Ctrl Pts',(2.1094237467878E-14,3.59759146080822,
1.1339965863823));
#53218=CARTESIAN_POINT('Ctrl Pts',(1.96107288013879E-14,3.57908349386506,
1.17749812614235));
#53219=CARTESIAN_POINT('Ctrl Pts',(-2.10007386744337E-15,3.55978689124514,
1.22068790168118));
#53220=CARTESIAN_POINT('Ctrl Pts',(-7.54951656745106E-15,3.53971110958904,
1.26354040163506));
#53221=CARTESIAN_POINT('Ctrl Pts',(-1.09169839508804E-14,3.52730533827528,
1.29002098026246));
#53222=CARTESIAN_POINT('Ctrl Pts',(5.45879109936265E-15,3.51460201437022,
1.31637274971798));
#53223=CARTESIAN_POINT('Ctrl Pts',(3.88578058618805E-15,3.50160321988813,
1.342589505873));
#53224=CARTESIAN_POINT('Ctrl Pts',(2.67861275308231E-15,3.49162761804916,
1.36270890396579));
#53225=CARTESIAN_POINT('Ctrl Pts',(-2.2629275639963E-14,3.48147646278302,
1.38275156313355));
#53226=CARTESIAN_POINT('Ctrl Pts',(-1.90958360235527E-14,3.47116236725966,
1.40269254368647));
#53227=CARTESIAN_POINT('Ctrl Pts',(-3.81991545211577E-16,3.4165367331714,
1.50830419955852));
#53228=CARTESIAN_POINT('Ctrl Pts',(-2.56312607080658E-15,3.35728334038055,
1.61119239851335));
#53229=CARTESIAN_POINT('Ctrl Pts',(-3.05311331771918E-15,3.2936112110481,
1.71099772625822));
#53230=CARTESIAN_POINT('Ctrl Pts',(-3.53944506258838E-15,3.23041410142351,
1.81005846609429));
#53231=CARTESIAN_POINT('Ctrl Pts',(2.27276944610714E-14,3.16286336209999,
1.90608284429344));
#53232=CARTESIAN_POINT('Ctrl Pts',(2.23154827949656E-14,3.09112535423912,
1.99868541489889));
#53233=CARTESIAN_POINT('Ctrl Pts',(2.19154714197454E-14,3.02151058702234,
2.08854721324816));
#53234=CARTESIAN_POINT('Ctrl Pts',(2.65458674629001E-14,2.94795215192818,
2.17518718759128));
#53235=CARTESIAN_POINT('Ctrl Pts',(2.56183962932255E-14,2.87057487892889,
2.25821308833352));
#53236=CARTESIAN_POINT('Ctrl Pts',(2.49982485680853E-14,2.81883705526706,
2.3137278311703));
#53237=CARTESIAN_POINT('Ctrl Pts',(1.93937339864825E-14,2.76539134747941,
2.36762595258285));
#53238=CARTESIAN_POINT('Ctrl Pts',(2.06779038336435E-14,2.71026985849297,
2.41977831105942));
#53239=CARTESIAN_POINT('Ctrl Pts',(2.12972403643666E-14,2.68368556216127,
2.4449306387202));
#53240=CARTESIAN_POINT('Ctrl Pts',(5.6667007202163E-15,2.65671142532864,
2.46967675127111));
#53241=CARTESIAN_POINT('Ctrl Pts',(7.02216063075412E-15,2.62935077228863,
2.49400127076223));
#53242=CARTESIAN_POINT('Ctrl Pts',(7.56656610583958E-15,2.61836166873706,
2.5037709448683));
#53243=CARTESIAN_POINT('Ctrl Pts',(5.67951698064326E-14,2.60731240461056,
2.51347060811221));
#53244=CARTESIAN_POINT('Ctrl Pts',(5.52891066263328E-14,2.59620959029183,
2.52309397415439));
#53245=CARTESIAN_POINT('Ctrl Pts',(4.38243996477893E-14,2.51169088318614,
2.59635057671843));
#53246=CARTESIAN_POINT('Ctrl Pts',(6.92167992872912E-15,2.42396547938964,
2.66528379542761));
#53247=CARTESIAN_POINT('Ctrl Pts',(7.13318293321663E-15,2.33318085873788,
2.72955162985394));
#53248=CARTESIAN_POINT('Ctrl Pts',(7.25502550614834E-15,2.28088168790746,
2.76657502024136));
#53249=CARTESIAN_POINT('Ctrl Pts',(1.05441232867865E-14,2.22756672536945,
2.80204936230559));
#53250=CARTESIAN_POINT('Ctrl Pts',(1.21846976952611E-14,2.17326041266705,
2.83590230914314));
#53251=CARTESIAN_POINT('Ctrl Pts',(1.50908074605165E-14,2.07718824792624,
2.89579085107679));
#53252=CARTESIAN_POINT('Ctrl Pts',(1.62408507202679E-14,1.97801391730883,
2.95060784545968));
#53253=CARTESIAN_POINT('Ctrl Pts',(2.30648833365876E-14,1.87615319865268,
3.00032665839637));
#53254=CARTESIAN_POINT('Ctrl Pts',(2.99199362602384E-14,1.77382944721587,
3.05027148034329));
#53255=CARTESIAN_POINT('Ctrl Pts',(4.48598975355489E-14,1.66879386290452,
3.09507168092574));
#53256=CARTESIAN_POINT('Ctrl Pts',(5.18474152499948E-14,1.56146419487867,
3.13464824772879));
#53257=CARTESIAN_POINT('Ctrl Pts',(5.3933480596659E-14,1.52942181441002,
3.14646350286254));
#53258=CARTESIAN_POINT('Ctrl Pts',(1.45371142394304E-14,1.49717499764285,
3.15781283903599));
#53259=CARTESIAN_POINT('Ctrl Pts',(1.41830991395864E-14,1.46473499388962,
3.16869325771511));
#53260=CARTESIAN_POINT('Ctrl Pts',(1.39834571560156E-14,1.44644089654973,
3.17482912132131));
#53261=CARTESIAN_POINT('Ctrl Pts',(8.93808405976052E-15,1.42808321458713,
3.18081643667667));
#53262=CARTESIAN_POINT('Ctrl Pts',(9.49240686054509E-15,1.40968594116012,
3.18664793170129));
#53263=CARTESIAN_POINT('Ctrl Pts',(1.26906562468948E-14,1.30354008469316,
3.22029362579435));
#53264=CARTESIAN_POINT('Ctrl Pts',(-3.59846457681172E-15,1.19592044539289,
3.24881064998302));
#53265=CARTESIAN_POINT('Ctrl Pts',(-1.0547118733939E-15,1.0872294197538,
3.27220684178733));
#53266=CARTESIAN_POINT('Ctrl Pts',(1.49132431113259E-15,0.978440824133397,
3.29562403593276));
#53267=CARTESIAN_POINT('Ctrl Pts',(3.55444460830568E-14,0.868577967529425,
3.31391114504953));
#53268=CARTESIAN_POINT('Ctrl Pts',(4.57966997657877E-14,0.758041213997769,
3.32702390602429));
#53269=CARTESIAN_POINT('Ctrl Pts',(5.59225919287158E-14,0.648866852833935,
3.33997504903125));
#53270=CARTESIAN_POINT('Ctrl Pts',(-2.24905070291909E-15,0.539034240310298,
3.34787845352108));
#53271=CARTESIAN_POINT('Ctrl Pts',(4.01068067645838E-15,0.428939545617156,
3.35064237850942));
#53272=CARTESIAN_POINT('Ctrl Pts',(7.73133663615164E-15,0.363501516872001,
3.35228519884096));
#53273=CARTESIAN_POINT('Ctrl Pts',(-4.85704133178524E-15,0.297971159229881,
3.3521113829659));
#53274=CARTESIAN_POINT('Ctrl Pts',(-1.02279296143593E-14,0.232435308205704,
3.35009360870352));
#53275=CARTESIAN_POINT('Ctrl Pts',(-1.28532778767699E-14,0.200400675653365,
3.34910729882796));
#53276=CARTESIAN_POINT('Ctrl Pts',(1.79661326338799E-14,0.168364780635814,
3.34768031034544));
#53277=CARTESIAN_POINT('Ctrl Pts',(1.75137682134618E-14,0.136338088246541,
3.34580893463049));
#53278=CARTESIAN_POINT('Ctrl Pts',(1.72908107034634E-14,0.120553045775695,
3.34488658695936));
#53279=CARTESIAN_POINT('Ctrl Pts',(4.81777123886202E-15,0.104779344373586,
3.34385680185526));
#53280=CARTESIAN_POINT('Ctrl Pts',(5.6621374255883E-15,0.0890209173056848,
3.34271970942635));
#53281=CARTESIAN_POINT('Ctrl Pts',(1.14070011246775E-14,-0.0181956162792568,
3.3349832070414));
#53282=CARTESIAN_POINT('Ctrl Pts',(2.34325705547898E-14,-0.124748133264004,
3.32228092968165));
#53283=CARTESIAN_POINT('Ctrl Pts',(2.26901830657766E-14,-0.230273591897684,
3.30457403911883));
#53284=CARTESIAN_POINT('Ctrl Pts',(2.19582654213507E-14,-0.334310831551059,
3.2871168677324));
#53285=CARTESIAN_POINT('Ctrl Pts',(-1.6042210484668E-14,-0.437350531390714,
3.26479505345607));
#53286=CARTESIAN_POINT('Ctrl Pts',(-1.62231339473351E-14,-0.539027315639043,
3.23752483134509));
#53287=CARTESIAN_POINT('Ctrl Pts',(-1.63984945268408E-14,-0.637577827248858,
3.21109309119302));
#53288=CARTESIAN_POINT('Ctrl Pts',(6.57984010550879E-17,-0.734848489443402,
3.18001228206578));
#53289=CARTESIAN_POINT('Ctrl Pts',(-4.31252256127834E-15,-0.830480771345168,
3.14416574488326));
#53290=CARTESIAN_POINT('Ctrl Pts',(-8.36192191764401E-15,-0.918928672746715,
3.11101218080159));
#53291=CARTESIAN_POINT('Ctrl Pts',(1.49022108953379E-15,-1.00597524039212,
3.07378159410529));
#53292=CARTESIAN_POINT('Ctrl Pts',(0.,-1.0913102200307,3.03235215074973));
#53293=CARTESIAN_POINT('Ctrl Pts',(-0.596163522034903,-3.93901438905508,
-0.00135576060872734));
#53294=CARTESIAN_POINT('Ctrl Pts',(-0.592210557955047,-3.93937169862689,
-0.0791783416986369));
#53295=CARTESIAN_POINT('Ctrl Pts',(-0.58825759387519,-3.93726116271843,
-0.156981519214978));
#53296=CARTESIAN_POINT('Ctrl Pts',(-0.584304629795334,-3.9326209789498,
-0.234634368276791));
#53297=CARTESIAN_POINT('Ctrl Pts',(-0.518013452562853,-3.85480513281932,
-1.53687205012064));
#53298=CARTESIAN_POINT('Ctrl Pts',(-0.45172227533037,-3.06556973519939,
-2.79683246351116));
#53299=CARTESIAN_POINT('Ctrl Pts',(-0.385431098097887,-1.92824404903633,
-3.43532026921666));
#53300=CARTESIAN_POINT('Ctrl Pts',(-0.319139920865397,-0.790918362873148,
-4.07380807492224));
#53301=CARTESIAN_POINT('Ctrl Pts',(-0.252848743632905,0.694497611833248,
-4.09082327294269));
#53302=CARTESIAN_POINT('Ctrl Pts',(-0.186557566400421,1.8470361740811,-3.479251425261));
#53303=CARTESIAN_POINT('Ctrl Pts',(-0.124371710933646,2.92819960251862,
-2.90555338405549));
#53304=CARTESIAN_POINT('Ctrl Pts',(-0.0621858554668791,3.71643826597518,
-1.77871263703401));
#53305=CARTESIAN_POINT('Ctrl Pts',(-9.86016823745217E-14,3.89860680620567,
-0.567889413567609));
#53306=CARTESIAN_POINT('',(-109.567,-1.87158653174005,-2.62360084934985));
#53307=CARTESIAN_POINT('Ctrl Pts',(-109.567,-1.87558868214585,-2.62754025481268));
#53308=CARTESIAN_POINT('Ctrl Pts',(-109.567,-1.93405508168532,-2.59497549554658));
#53309=CARTESIAN_POINT('Ctrl Pts',(-109.567,-1.99134228758153,-2.56051026827204));
#53310=CARTESIAN_POINT('Ctrl Pts',(-109.567,-2.04734666558749,-2.52416324142431));
#53311=CARTESIAN_POINT('Ctrl Pts',(-109.567,-2.13340847164491,-2.46830884420198));
#53312=CARTESIAN_POINT('Ctrl Pts',(-109.567,-2.21644226853764,-2.4080133982524));
#53313=CARTESIAN_POINT('Ctrl Pts',(-109.567,-2.29635488563297,-2.34366975158224));
#53314=CARTESIAN_POINT('Ctrl Pts',(-109.567,-2.34682481961543,-2.30303261920351));
#53315=CARTESIAN_POINT('Ctrl Pts',(-109.567,-2.39604948944602,-2.26077970899706));
#53316=CARTESIAN_POINT('Ctrl Pts',(-109.567,-2.44400132255651,-2.21700032194834));
#53317=CARTESIAN_POINT('Ctrl Pts',(-109.567,-2.47482458050397,-2.18885909663428));
#53318=CARTESIAN_POINT('Ctrl Pts',(-109.567,-2.50512185085323,-2.1600870049542));
#53319=CARTESIAN_POINT('Ctrl Pts',(-109.567,-2.53488497154578,-2.13070632870751));
#53320=CARTESIAN_POINT('Ctrl Pts',(-109.567,-2.54830243821907,-2.11746127122677));
#53321=CARTESIAN_POINT('Ctrl Pts',(-109.567,-2.56161091598415,-2.10409282722601));
#53322=CARTESIAN_POINT('Ctrl Pts',(-109.567,-2.57480027481449,-2.09061288448896));
#53323=CARTESIAN_POINT('Ctrl Pts',(-109.567,-2.64900045473092,-2.01477794897633));
#53324=CARTESIAN_POINT('Ctrl Pts',(-109.567,-2.71951129357198,-1.9353409036445));
#53325=CARTESIAN_POINT('Ctrl Pts',(-109.567,-2.78623172025196,-1.85270968846994));
#53326=CARTESIAN_POINT('Ctrl Pts',(-109.567,-2.84985923039024,-1.77390895617731));
#53327=CARTESIAN_POINT('Ctrl Pts',(-109.567,-2.91003979995533,-1.69220250627302));
#53328=CARTESIAN_POINT('Ctrl Pts',(-109.567,-2.96666467242472,-1.60790763032119));
#53329=CARTESIAN_POINT('Ctrl Pts',(-109.567,-2.99143805413007,-1.57102862209226));
#53330=CARTESIAN_POINT('Ctrl Pts',(-109.567,-3.01553055578497,-1.53365375878569));
#53331=CARTESIAN_POINT('Ctrl Pts',(-109.567,-3.03893156594076,-1.49580784353154));
#53332=CARTESIAN_POINT('Ctrl Pts',(-109.567,-3.04980560210158,-1.47822151506651));
#53333=CARTESIAN_POINT('Ctrl Pts',(-109.567,-3.06053031082592,-1.46053345873251));
#53334=CARTESIAN_POINT('Ctrl Pts',(-109.567,-3.07110455244537,-1.44274609509514));
#53335=CARTESIAN_POINT('Ctrl Pts',(-109.567,-3.08003851032833,-1.42771791971349));
#53336=CARTESIAN_POINT('Ctrl Pts',(-109.567,-3.08886464794213,-1.41261942057115));
#53337=CARTESIAN_POINT('Ctrl Pts',(-109.567,-3.09757568073968,-1.3974639260691));
#53338=CARTESIAN_POINT('Ctrl Pts',(-109.567,-3.15304228551282,-1.3009628746756));
#53339=CARTESIAN_POINT('Ctrl Pts',(-109.567,-3.20391780446871,-1.20203235076329));
#53340=CARTESIAN_POINT('Ctrl Pts',(-109.567,-3.25009311850581,-1.10110149034648));
#53341=CARTESIAN_POINT('Ctrl Pts',(-109.567,-3.29699647665682,-0.998579257561797));
#53342=CARTESIAN_POINT('Ctrl Pts',(-109.567,-3.33905083589063,-0.893992444125954));
#53343=CARTESIAN_POINT('Ctrl Pts',(-109.567,-3.37610808814847,-0.787749106949813));
#53344=CARTESIAN_POINT('Ctrl Pts',(-109.567,-3.41307771922245,-0.681756980168778));
#53345=CARTESIAN_POINT('Ctrl Pts',(-109.567,-3.44507435458282,-0.574115341585501));
#53346=CARTESIAN_POINT('Ctrl Pts',(-109.567,-3.471909492288,-0.465199525320855));
#53347=CARTESIAN_POINT('Ctrl Pts',(-109.567,-3.48930969706608,-0.394577286396749));
#53348=CARTESIAN_POINT('Ctrl Pts',(-109.567,-3.50453895879291,-0.323418758370256));
#53349=CARTESIAN_POINT('Ctrl Pts',(-109.567,-3.51753498407954,-0.251822000732028));
#53350=CARTESIAN_POINT('Ctrl Pts',(-109.567,-3.52185337791623,-0.228031419374075));
#53351=CARTESIAN_POINT('Ctrl Pts',(-109.567,-3.5259251160337,-0.204192432008078));
#53352=CARTESIAN_POINT('Ctrl Pts',(-109.567,-3.52974768103556,-0.18030858771712));
#53353=CARTESIAN_POINT('Ctrl Pts',(-109.567,-3.5322279650709,-0.164811475786041));
#53354=CARTESIAN_POINT('Ctrl Pts',(-109.567,-3.53460305911876,-0.149296894027067));
#53355=CARTESIAN_POINT('Ctrl Pts',(-109.567,-3.53687070026767,-0.133777965353361));
#53356=CARTESIAN_POINT('Ctrl Pts',(-109.567,-3.55362006210883,-0.0191512961964261));
#53357=CARTESIAN_POINT('Ctrl Pts',(-109.567,-3.56453969470775,0.0958883104104314));
#53358=CARTESIAN_POINT('Ctrl Pts',(-109.567,-3.56948236683328,0.210916428015749));
#53359=CARTESIAN_POINT('Ctrl Pts',(-109.567,-3.57215030524466,0.273005906248279));
#53360=CARTESIAN_POINT('Ctrl Pts',(-109.567,-3.57307608943884,0.335092588218926));
#53361=CARTESIAN_POINT('Ctrl Pts',(-109.567,-3.57223104459554,0.397112793171267));
#53362=CARTESIAN_POINT('Ctrl Pts',(-109.567,-3.57071960889364,0.508041287378316));
#53363=CARTESIAN_POINT('Ctrl Pts',(-109.567,-3.5635465120436,0.618756803306876));
#53364=CARTESIAN_POINT('Ctrl Pts',(-109.567,-3.55097661781193,0.728974557829716));
#53365=CARTESIAN_POINT('Ctrl Pts',(-109.567,-3.53816715848062,0.841292912950918));
#53366=CARTESIAN_POINT('Ctrl Pts',(-109.567,-3.5197531319118,0.953095028235097));
#53367=CARTESIAN_POINT('Ctrl Pts',(-109.567,-3.49596074425854,1.0640829788475));
#53368=CARTESIAN_POINT('Ctrl Pts',(-109.567,-3.488522449697,1.09878151694581));
#53369=CARTESIAN_POINT('Ctrl Pts',(-109.567,-3.48055809112876,1.1334004624857));
#53370=CARTESIAN_POINT('Ctrl Pts',(-109.567,-3.47207355089471,1.16793061249935));
#53371=CARTESIAN_POINT('Ctrl Pts',(-109.567,-3.46814577917836,1.18391575050844));
#53372=CARTESIAN_POINT('Ctrl Pts',(-109.567,-3.46410593314054,1.19988411131588));
#53373=CARTESIAN_POINT('Ctrl Pts',(-109.567,-3.4599564744153,1.21582745846855));
#53374=CARTESIAN_POINT('Ctrl Pts',(-109.567,-3.43129298422129,1.32596037098317));
#53375=CARTESIAN_POINT('Ctrl Pts',(-109.567,-3.39747435133908,1.43463252196887));
#53376=CARTESIAN_POINT('Ctrl Pts',(-109.567,-3.35880367683646,1.54155102136754));
#53377=CARTESIAN_POINT('Ctrl Pts',(-109.567,-3.31885844540897,1.65199347568964));
#53378=CARTESIAN_POINT('Ctrl Pts',(-109.567,-3.27373604012402,1.76056546471733));
#53379=CARTESIAN_POINT('Ctrl Pts',(-109.567,-3.22371511386614,1.86694840066266));
#53380=CARTESIAN_POINT('Ctrl Pts',(-109.567,-3.17318630958296,1.97441147565131));
#53381=CARTESIAN_POINT('Ctrl Pts',(-109.567,-3.11765875257899,2.07964161817074));
#53382=CARTESIAN_POINT('Ctrl Pts',(-109.567,-3.05736645015778,2.18230326993847));
#53383=CARTESIAN_POINT('Ctrl Pts',(-109.567,-3.01747154321521,2.25023361725265));
#53384=CARTESIAN_POINT('Ctrl Pts',(-109.567,-2.97548937180041,2.31703922297468));
#53385=CARTESIAN_POINT('Ctrl Pts',(-109.567,-2.93147598465934,2.38261852576162));
#53386=CARTESIAN_POINT('Ctrl Pts',(-109.567,-2.91011659414414,2.41444370507471));
#53387=CARTESIAN_POINT('Ctrl Pts',(-109.567,-2.88827869870454,2.44598001332719));
#53388=CARTESIAN_POINT('Ctrl Pts',(-109.567,-2.8659679668509,2.47721541551838));
#53389=CARTESIAN_POINT('Ctrl Pts',(-109.567,-2.85153128249921,2.49742701794319));
#53390=CARTESIAN_POINT('Ctrl Pts',(-109.567,-2.83689258662859,2.517517866556));
#53391=CARTESIAN_POINT('Ctrl Pts',(-109.567,-2.82207503428789,2.53745591080546));
#53392=CARTESIAN_POINT('Ctrl Pts',(-109.567,-2.7489276911345,2.63588073367702));
#53393=CARTESIAN_POINT('Ctrl Pts',(-109.567,-2.67135364275062,2.73068902811859));
#53394=CARTESIAN_POINT('Ctrl Pts',(-109.567,-2.58964383806861,2.82154575548173));
#53395=CARTESIAN_POINT('Ctrl Pts',(-109.567,-2.50782128256363,2.9125278554464));
#53396=CARTESIAN_POINT('Ctrl Pts',(-109.567,-2.42185116409135,2.99954830547996));
#53397=CARTESIAN_POINT('Ctrl Pts',(-109.567,-2.33197556942183,3.08225487705311));
#53398=CARTESIAN_POINT('Ctrl Pts',(-109.567,-2.2422857465215,3.16479049514126));
#53399=CARTESIAN_POINT('Ctrl Pts',(-109.567,-2.14870616705358,3.24303087993829));
#53400=CARTESIAN_POINT('Ctrl Pts',(-109.567,-2.05143358017556,3.31659784347169));
#53401=CARTESIAN_POINT('Ctrl Pts',(-109.567,-1.95416099329755,3.3901648070051));
#53402=CARTESIAN_POINT('Ctrl Pts',(-109.567,-1.85319500343946,3.45905921673876));
#53403=CARTESIAN_POINT('Ctrl Pts',(-109.567,-1.74869447533098,3.52286199445095));
#53404=CARTESIAN_POINT('Ctrl Pts',(-109.567,-1.8755886821457,-2.62754025481279));
#53405=CARTESIAN_POINT('Ctrl Pts',(-109.504814144533,-1.05624460814695,
-3.20663122225699));
#53406=CARTESIAN_POINT('Ctrl Pts',(-109.376337111834,1.24418819625944,-3.56417172636872));
#53407=CARTESIAN_POINT('Ctrl Pts',(-109.181568901902,3.6901636846244,-0.955038498682453));
#53408=CARTESIAN_POINT('Ctrl Pts',(-108.982695370205,2.7979887412231,2.58915131051891));
#53409=CARTESIAN_POINT('Ctrl Pts',(-108.783821838507,-0.665419358724505,
3.75306610556087));
#53410=CARTESIAN_POINT('Ctrl Pts',(-108.624998898681,-2.94289439362547,
1.92928088442713));
#53411=CARTESIAN_POINT('Ctrl Pts',(-108.532467136088,-3.22041771955432,
0.428199733749597));
#53412=CARTESIAN_POINT('Ctrl Pts',(-108.506226550727,-3.21833411702487,
0.00177219254916029));
#53413=CARTESIAN_POINT('Origin',(-109.567,-5.160062080289E-16,2.1385152528819E-16));
#53414=CARTESIAN_POINT('',(-109.567,-3.93300000000001,-4.81653586104655E-16));
#53415=CARTESIAN_POINT('Origin',(-109.567,0.,0.));
#53416=CARTESIAN_POINT('Origin',(-109.567,0.,0.));
#53417=CARTESIAN_POINT('',(-109.567,1.87158653173898,-2.62360084935061));
#53418=CARTESIAN_POINT('Ctrl Pts',(-109.567,1.75275645914455,3.52838181187388));
#53419=CARTESIAN_POINT('Ctrl Pts',(-109.567,1.82202500014327,3.48645490739411));
#53420=CARTESIAN_POINT('Ctrl Pts',(-109.567,1.88981509185284,3.44228222701039));
#53421=CARTESIAN_POINT('Ctrl Pts',(-109.567,1.95600382845685,3.3958567385041));
#53422=CARTESIAN_POINT('Ctrl Pts',(-109.567,2.05546182159306,3.32609583726757));
#53423=CARTESIAN_POINT('Ctrl Pts',(-109.567,2.15130605150922,3.25124954236935));
#53424=CARTESIAN_POINT('Ctrl Pts',(-109.567,2.24335219247688,3.17172823304734));
#53425=CARTESIAN_POINT('Ctrl Pts',(-109.567,2.29724160807795,3.12517161652716));
#53426=CARTESIAN_POINT('Ctrl Pts',(-109.567,2.34982843551166,3.07701188213643));
#53427=CARTESIAN_POINT('Ctrl Pts',(-109.567,2.40106891848523,3.02732681361603));
#53428=CARTESIAN_POINT('Ctrl Pts',(-109.567,2.44038120004853,2.98920786371907));
#53429=CARTESIAN_POINT('Ctrl Pts',(-109.567,2.47890090599221,2.95019101034076));
#53430=CARTESIAN_POINT('Ctrl Pts',(-109.567,2.51660611613464,2.91031044345441));
#53431=CARTESIAN_POINT('Ctrl Pts',(-109.567,2.53156447098204,2.89448908431736));
#53432=CARTESIAN_POINT('Ctrl Pts',(-109.567,2.54639525737649,2.87853096014503));
#53433=CARTESIAN_POINT('Ctrl Pts',(-109.567,2.56108565929238,2.86245096993407));
#53434=CARTESIAN_POINT('Ctrl Pts',(-109.567,2.64412131549488,2.77156084000153));
#53435=CARTESIAN_POINT('Ctrl Pts',(-109.567,2.72276365995974,2.67668790351876));
#53436=CARTESIAN_POINT('Ctrl Pts',(-109.567,2.79681743724591,2.57825667956293));
#53437=CARTESIAN_POINT('Ctrl Pts',(-109.567,2.86161449237131,2.49212935860158));
#53438=CARTESIAN_POINT('Ctrl Pts',(-109.567,2.92289790212134,2.40327677587802));
#53439=CARTESIAN_POINT('Ctrl Pts',(-109.567,2.98050509863801,2.31196927698884));
#53440=CARTESIAN_POINT('Ctrl Pts',(-109.567,3.00573063331407,2.27198676406189));
#53441=CARTESIAN_POINT('Ctrl Pts',(-109.567,3.03025086583581,2.23153340920802));
#53442=CARTESIAN_POINT('Ctrl Pts',(-109.567,3.05405020721428,2.19063151133595));
#53443=CARTESIAN_POINT('Ctrl Pts',(-109.567,3.06875694113979,2.16535630226663));
#53444=CARTESIAN_POINT('Ctrl Pts',(-109.567,3.08318837281295,2.13990980974904));
#53445=CARTESIAN_POINT('Ctrl Pts',(-109.567,3.09734058716092,2.114297277655));
#53446=CARTESIAN_POINT('Ctrl Pts',(-109.567,3.10820135238902,2.09464157635407));
#53447=CARTESIAN_POINT('Ctrl Pts',(-109.567,3.11889908116918,2.07488524212842));
#53448=CARTESIAN_POINT('Ctrl Pts',(-109.567,3.12942045161792,2.05505284340651));
#53449=CARTESIAN_POINT('Ctrl Pts',(-109.567,3.18514385739147,1.95001626030842));
#53450=CARTESIAN_POINT('Ctrl Pts',(-109.567,3.23599354366025,1.84272574147176));
#53451=CARTESIAN_POINT('Ctrl Pts',(-109.567,3.28179303842333,1.73355775273866));
#53452=CARTESIAN_POINT('Ctrl Pts',(-109.567,3.32725085049152,1.62520420121232));
#53453=CARTESIAN_POINT('Ctrl Pts',(-109.567,3.36773377451,1.51500022479072));
#53454=CARTESIAN_POINT('Ctrl Pts',(-109.567,3.40301964925438,1.40330203831042));
#53455=CARTESIAN_POINT('Ctrl Pts',(-109.567,3.43726116268567,1.29490979976387));
#53456=CARTESIAN_POINT('Ctrl Pts',(-109.567,3.46660872504405,1.18510975826472));
#53457=CARTESIAN_POINT('Ctrl Pts',(-109.567,3.49081093656453,1.07422785924485));
#53458=CARTESIAN_POINT('Ctrl Pts',(-109.567,3.50699359207182,1.00008737946617));
#53459=CARTESIAN_POINT('Ctrl Pts',(-109.567,3.52087485467189,0.925463243069554));
#53460=CARTESIAN_POINT('Ctrl Pts',(-109.567,3.53236683395441,0.85045536704003));
#53461=CARTESIAN_POINT('Ctrl Pts',(-109.567,3.53790924920365,0.81428015425042));
#53462=CARTESIAN_POINT('Ctrl Pts',(-109.567,3.54289576268122,0.778015725169597));
#53463=CARTESIAN_POINT('Ctrl Pts',(-109.567,3.54731562475149,0.741673567948634));
#53464=CARTESIAN_POINT('Ctrl Pts',(-109.567,3.54909081350037,0.727077142181763));
#53465=CARTESIAN_POINT('Ctrl Pts',(-109.567,3.55077419437748,0.712471117916151));
#53466=CARTESIAN_POINT('Ctrl Pts',(-109.567,3.55236436289117,0.697864508620402));
#53467=CARTESIAN_POINT('Ctrl Pts',(-109.567,3.56446931029815,0.586673628033493));
#53468=CARTESIAN_POINT('Ctrl Pts',(-109.567,3.57119429444985,0.475307970362645));
#53469=CARTESIAN_POINT('Ctrl Pts',(-109.567,3.57234212104006,0.364083492885442));
#53470=CARTESIAN_POINT('Ctrl Pts',(-109.567,3.57300336055886,0.300009336917556));
#53471=CARTESIAN_POINT('Ctrl Pts',(-109.567,3.57181279307812,0.235982024622193));
#53472=CARTESIAN_POINT('Ctrl Pts',(-109.567,3.56872485737067,0.172062839259968));
#53473=CARTESIAN_POINT('Ctrl Pts',(-109.567,3.5632620547378,0.0589847420555476));
#53474=CARTESIAN_POINT('Ctrl Pts',(-109.567,3.55186373352207,-0.0537562397880342));
#53475=CARTESIAN_POINT('Ctrl Pts',(-109.567,3.53474471555629,-0.165803129864622));
#53476=CARTESIAN_POINT('Ctrl Pts',(-109.567,3.5175478789259,-0.278359356363241));
#53477=CARTESIAN_POINT('Ctrl Pts',(-109.567,3.49457768041398,-0.390215969444795));
#53478=CARTESIAN_POINT('Ctrl Pts',(-109.567,3.46600700359361,-0.500984551047218));
#53479=CARTESIAN_POINT('Ctrl Pts',(-109.567,3.45747746547809,-0.534053590493489));
#53480=CARTESIAN_POINT('Ctrl Pts',(-109.567,3.44844850025554,-0.567025433035426));
#53481=CARTESIAN_POINT('Ctrl Pts',(-109.567,3.43892404746731,-0.599889123387569));
#53482=CARTESIAN_POINT('Ctrl Pts',(-109.567,3.43355286207557,-0.618422153836961));
#53483=CARTESIAN_POINT('Ctrl Pts',(-109.567,3.4280233534425,-0.636922883471933));
#53484=CARTESIAN_POINT('Ctrl Pts',(-109.567,3.42234320335153,-0.655367447148205));
#53485=CARTESIAN_POINT('Ctrl Pts',(-109.567,3.38957071812405,-0.76178614752175));
#53486=CARTESIAN_POINT('Ctrl Pts',(-109.567,3.35174285235985,-0.866496509973046));
#53487=CARTESIAN_POINT('Ctrl Pts',(-109.567,3.30909514849801,-0.969172184804078));
#53488=CARTESIAN_POINT('Ctrl Pts',(-109.567,3.26640916057173,-1.0719400297122));
#53489=CARTESIAN_POINT('Ctrl Pts',(-109.567,3.2188940912709,-1.17267028238691));
#53490=CARTESIAN_POINT('Ctrl Pts',(-109.567,3.16674149373716,-1.27100860119449));
#53491=CARTESIAN_POINT('Ctrl Pts',(-109.567,3.11523168974658,-1.36813487612768));
#53492=CARTESIAN_POINT('Ctrl Pts',(-109.567,3.05919735145539,-1.4629284384482));
#53493=CARTESIAN_POINT('Ctrl Pts',(-109.567,2.99878861195219,-1.5550113642337));
#53494=CARTESIAN_POINT('Ctrl Pts',(-109.567,2.96288289596785,-1.60974356701515));
#53495=CARTESIAN_POINT('Ctrl Pts',(-109.567,2.9254311493055,-1.66351739572016));
#53496=CARTESIAN_POINT('Ctrl Pts',(-109.567,2.88646034894762,-1.71624590697244));
#53497=CARTESIAN_POINT('Ctrl Pts',(-109.567,2.86741100001697,-1.74202017386495));
#53498=CARTESIAN_POINT('Ctrl Pts',(-109.567,2.84799864852909,-1.76754458402546));
#53499=CARTESIAN_POINT('Ctrl Pts',(-109.567,2.82822620377072,-1.7928084225986));
#53500=CARTESIAN_POINT('Ctrl Pts',(-109.567,2.81848093071187,-1.8052602467619));
#53501=CARTESIAN_POINT('Ctrl Pts',(-109.567,2.80865378977432,-1.81764157929085));
#53502=CARTESIAN_POINT('Ctrl Pts',(-109.567,2.79874712727207,-1.8299492607085));
#53503=CARTESIAN_POINT('Ctrl Pts',(-109.567,2.73134458457393,-1.91368775710731));
#53504=CARTESIAN_POINT('Ctrl Pts',(-109.567,2.6602377061028,-1.99405316358428));
#53505=CARTESIAN_POINT('Ctrl Pts',(-109.567,2.58560125585586,-2.07072490991953));
#53506=CARTESIAN_POINT('Ctrl Pts',(-109.567,2.51201739882552,-2.14631535938401));
#53507=CARTESIAN_POINT('Ctrl Pts',(-109.567,2.43500223422176,-2.21831610629024));
#53508=CARTESIAN_POINT('Ctrl Pts',(-109.567,2.35469492044372,-2.28637908316542));
#53509=CARTESIAN_POINT('Ctrl Pts',(-109.567,2.27685682873383,-2.35234931659522));
#53510=CARTESIAN_POINT('Ctrl Pts',(-109.567,2.19592538297238,-2.41462049371991));
#53511=CARTESIAN_POINT('Ctrl Pts',(-109.567,2.11200880209288,-2.47283144644441));
#53512=CARTESIAN_POINT('Ctrl Pts',(-109.567,2.0343964590955,-2.52666929805499));
#53513=CARTESIAN_POINT('Ctrl Pts',(-109.567,1.95423020934163,-2.5770339076807));
#53514=CARTESIAN_POINT('Ctrl Pts',(-109.567,1.87158653173824,-2.62360084935114));
#53515=CARTESIAN_POINT('Origin',(-109.567,0.,0.));
#53516=CARTESIAN_POINT('Origin',(-111.877773449273,0.,0.));
#53517=CARTESIAN_POINT('Ctrl Pts',(-109.567,1.87158653173818,-2.62360084935118));
#53518=CARTESIAN_POINT('Ctrl Pts',(-109.500708822768,2.74581178927839,-1.99995864473678));
#53519=CARTESIAN_POINT('Ctrl Pts',(-109.368126468303,3.80651295487345,0.179129781420444));
#53520=CARTESIAN_POINT('Ctrl Pts',(-109.169252936605,1.9032035356359,3.30567173395145));
#53521=CARTESIAN_POINT('Ctrl Pts',(-108.970379404908,-1.7502378889635,3.3848793341849));
#53522=CARTESIAN_POINT('Ctrl Pts',(-108.83155290913,-3.17746554677698,1.27272365819482));
#53523=CARTESIAN_POINT('Ctrl Pts',(-108.759017590586,-3.22751915473568,
0.102767056756573));
#53524=CARTESIAN_POINT('Ctrl Pts',(-108.752773449273,-3.22685723674299,
0.00199079345700971));
#53525=CARTESIAN_POINT('Ctrl Pts',(-109.977063028692,2.28405859260862,-3.20180657528383));
#53526=CARTESIAN_POINT('Ctrl Pts',(-109.910771851459,3.35095113404214,-2.44072216267053));
#53527=CARTESIAN_POINT('Ctrl Pts',(-109.778189496995,4.64541632193532,0.21860753404117));
#53528=CARTESIAN_POINT('Ctrl Pts',(-109.579315965297,2.32264355151719,4.03419654941691));
#53529=CARTESIAN_POINT('Ctrl Pts',(-109.3804424336,-2.13596636949734,4.13086042086637));
#53530=CARTESIAN_POINT('Ctrl Pts',(-109.181568901902,-4.63110802863978,
0.438297717986617));
#53531=CARTESIAN_POINT('Ctrl Pts',(-108.982695370205,-2.87167397122528,
-3.66022965207199));
#53532=CARTESIAN_POINT('Ctrl Pts',(-108.783821838507,1.52652252159763,-4.394010664145));
#53533=CARTESIAN_POINT('Ctrl Pts',(-108.58494830681,4.52200798253338,-1.09147594363445));
#53534=CARTESIAN_POINT('Ctrl Pts',(-108.386074775112,3.3627368399975,3.21439114027321));
#53535=CARTESIAN_POINT('Ctrl Pts',(-108.187201243415,-0.886262802760796,
4.56661377013007));
#53536=CARTESIAN_POINT('Ctrl Pts',(-107.988327711717,-4.32094171494865,
1.72315748479787));
#53537=CARTESIAN_POINT('Ctrl Pts',(-107.78945418002,-3.78554144244751,-2.70361103446967));
#53538=CARTESIAN_POINT('Ctrl Pts',(-107.590580648323,0.228027871382542,
-4.64625826502713));
#53539=CARTESIAN_POINT('Ctrl Pts',(-107.391707116625,4.03208164170884,-2.31993394368827));
#53540=CARTESIAN_POINT('Ctrl Pts',(-107.192833584928,4.13145214500505,2.13796108409874));
#53541=CARTESIAN_POINT('Ctrl Pts',(-106.99396005323,0.434835074219217,4.63148744537977));
#53542=CARTESIAN_POINT('Ctrl Pts',(-106.795086521533,-3.66130890000019,
2.86959661519726));
#53543=CARTESIAN_POINT('Ctrl Pts',(-106.596212989835,-4.39343498051869,
-1.52888705693157));
#53544=CARTESIAN_POINT('Ctrl Pts',(-106.397339458138,-1.08886385223194,
-4.52262532524078));
#53545=CARTESIAN_POINT('Ctrl Pts',(-106.19846592644,3.21615755154426,-3.3609666016501));
#53546=CARTESIAN_POINT('Ctrl Pts',(-105.999592394743,4.56616682915475,0.888755371192072));
#53547=CARTESIAN_POINT('Ctrl Pts',(-105.800718863045,1.72077262957113,4.3218869598412));
#53548=CARTESIAN_POINT('Ctrl Pts',(-105.601845331348,-2.70567098522491,
3.78406000159801));
#53549=CARTESIAN_POINT('Ctrl Pts',(-105.402971799651,-4.64613854864029,
-0.230569090679434));
#53550=CARTESIAN_POINT('Ctrl Pts',(-105.204098267953,-2.31772447095656,
-4.03335081055775));
#53551=CARTESIAN_POINT('Ctrl Pts',(-105.005224736256,2.14021960806887,-4.13028153390441));
#53552=CARTESIAN_POINT('Ctrl Pts',(-104.806351204558,4.63172551753725,-0.432301098127802));
#53553=CARTESIAN_POINT('Ctrl Pts',(-104.607477672861,2.86759251087864,3.66287847149825));
#53554=CARTESIAN_POINT('Ctrl Pts',(-104.408604141163,-1.53129038250247,
4.39259778207621));
#53555=CARTESIAN_POINT('Ctrl Pts',(-104.209730609466,-4.52322052840125,
1.08638923051286));
#53556=CARTESIAN_POINT('Ctrl Pts',(-104.010857077768,-3.35920636533815,
-3.21799597629154));
#53557=CARTESIAN_POINT('Ctrl Pts',(-103.811983546071,0.891253503530981,
-4.56567987287217));
#53558=CARTESIAN_POINT('Ctrl Pts',(-103.613110014374,4.32282782338692,-1.71840772755835));
#53559=CARTESIAN_POINT('Ctrl Pts',(-103.414236482676,3.78257906316194,2.707740966135));
#53560=CARTESIAN_POINT('Ctrl Pts',(-103.215362950979,-0.233111106957137,
4.64601170044533));
#53561=CARTESIAN_POINT('Ctrl Pts',(-103.016489419281,-4.03461831336596,
2.31551734484117));
#53562=CARTESIAN_POINT('Ctrl Pts',(-102.817615887584,-4.12910992928167,
-2.1424791015823));
#53563=CARTESIAN_POINT('Ctrl Pts',(-102.618742355886,-0.42976686398599,
-4.63196135038316));
#53564=CARTESIAN_POINT('Ctrl Pts',(-102.419868824189,3.66444687836893,-2.86558799977029));
#53565=CARTESIAN_POINT('Ctrl Pts',(-102.220995292491,4.39175930477002,1.53369348886343));
#53566=CARTESIAN_POINT('Ctrl Pts',(-102.022121760794,1.08391426446963,4.52381425083935));
#53567=CARTESIAN_POINT('Ctrl Pts',(-101.823248229096,-3.21983342759692,
3.35744519052003));
#53568=CARTESIAN_POINT('Ctrl Pts',(-101.624374697399,-4.56519155519177,
-0.893751404598992));
#53569=CARTESIAN_POINT('Ctrl Pts',(-101.425501165701,-1.71604230829386,
-4.32376737405733));
#53570=CARTESIAN_POINT('Ctrl Pts',(-101.226627634004,2.70981013496705,-3.78109700235881));
#53571=CARTESIAN_POINT('Ctrl Pts',(-101.027754102307,4.64588346224142,0.235653058729701));
#53572=CARTESIAN_POINT('Ctrl Pts',(-100.828880570609,2.31330952514332,4.03588460559741));
#53573=CARTESIAN_POINT('Ctrl Pts',(-100.630007038912,-2.14473795351143,
4.12793709007108));
#53574=CARTESIAN_POINT('Ctrl Pts',(-100.431133507214,-4.63219579674829,
0.427232500407485));
#53575=CARTESIAN_POINT('Ctrl Pts',(-100.232259975517,-2.86358263077228,
-3.6660141878553));
#53576=CARTESIAN_POINT('Ctrl Pts',(-100.033386443819,1.53609613607296,-4.39091951299027));
#53577=CARTESIAN_POINT('Ctrl Pts',(-99.8345129121218,4.52440661907031,-1.08143897383521));
#53578=CARTESIAN_POINT('Ctrl Pts',(-99.6356393804243,3.35568301062586,3.22166991496862));
#53579=CARTESIAN_POINT('Ctrl Pts',(-99.4367658487269,-0.896249038113484,
4.56470187093282));
#53580=CARTESIAN_POINT('Ctrl Pts',(-99.2378923170294,-4.3247056303906,1.71367637530684));
#53581=CARTESIAN_POINT('Ctrl Pts',(-99.039018785332,-3.77961380966542,-2.71187849259577));
#53582=CARTESIAN_POINT('Ctrl Pts',(-98.8401452536345,0.238194939957711,
-4.64575383327566));
#53583=CARTESIAN_POINT('Ctrl Pts',(-98.6412717219371,4.03714968966855,-2.31110101294298));
#53584=CARTESIAN_POINT('Ctrl Pts',(-98.4423981902396,4.12676301514323,2.146996163402));
#53585=CARTESIAN_POINT('Ctrl Pts',(-98.2435246585422,0.424698008935038,
4.63242885644492));
#53586=CARTESIAN_POINT('Ctrl Pts',(-98.0446511268446,-3.66758039990343,
2.86157640454717));
#53587=CARTESIAN_POINT('Ctrl Pts',(-97.8457775951473,-4.39007840676843,
-1.53849832344483));
#53588=CARTESIAN_POINT('Ctrl Pts',(-97.6469040634498,-1.07896335946704,
-4.52499763289935));
#53589=CARTESIAN_POINT('Ctrl Pts',(-97.4480305317523,3.22350543791854,-3.35391982619242));
#53590=CARTESIAN_POINT('Ctrl Pts',(-97.249157000055,4.56421082020927,0.898746403331652));
#53591=CARTESIAN_POINT('Ctrl Pts',(-97.0502834683573,1.71130992932287,4.32564259210328));
#53592=CARTESIAN_POINT('Ctrl Pts',(-96.8514099366601,-2.71394603841112,
3.77812948552713));
#53593=CARTESIAN_POINT('Ctrl Pts',(-96.6525364049624,-4.64562281358202,
-0.240736749880956));
#53594=CARTESIAN_POINT('Ctrl Pts',(-96.4536628732651,-2.3088918089039,-4.03841356520025));
#53595=CARTESIAN_POINT('Ctrl Pts',(-96.2547893415676,2.14925373057933,-4.1255877048498));
#53596=CARTESIAN_POINT('Ctrl Pts',(-96.0559158098702,4.63266052940256,-0.422163390327286));
#53597=CARTESIAN_POINT('Ctrl Pts',(-95.8570422781727,2.85956932169593,3.66914551404444));
#53598=CARTESIAN_POINT('Ctrl Pts',(-95.6581687464752,-1.54090005026015,
4.38923598635631));
#53599=CARTESIAN_POINT('Ctrl Pts',(-95.4592952147778,-4.5255872921494,1.07648742210618));
#53600=CARTESIAN_POINT('Ctrl Pts',(-95.2604216830804,-3.35215563774757,
-3.2253399958972));
#53601=CARTESIAN_POINT('Ctrl Pts',(-95.0615481513828,0.901243499505942,
-4.56371840316811));
#53602=CARTESIAN_POINT('Ctrl Pts',(-94.8626746196855,4.32657825891484,-1.70894297105036));
#53603=CARTESIAN_POINT('Ctrl Pts',(-94.6638010879879,3.77664403038834,2.71601277179418));
#53604=CARTESIAN_POINT('Ctrl Pts',(-94.4649275562906,-0.24327848773853,
4.64549040319971));
#53605=CARTESIAN_POINT('Ctrl Pts',(-94.266054024593,-4.0396762318142,2.30668191368736));
#53606=CARTESIAN_POINT('Ctrl Pts',(-94.0671804928956,-4.12441115954261,
-2.15151065436761));
#53607=CARTESIAN_POINT('Ctrl Pts',(-93.8683069611983,-0.419628645342997,
-4.63289081555184));
#53608=CARTESIAN_POINT('Ctrl Pts',(-93.6694334295006,3.67070952980976,-2.85756138281943));
#53609=CARTESIAN_POINT('Ctrl Pts',(-93.4705598978034,4.38839225200612,1.54330131579987));
#53610=CARTESIAN_POINT('Ctrl Pts',(-93.2716863661057,1.07401116249385,4.52617559664399));
#53611=CARTESIAN_POINT('Ctrl Pts',(-93.0728128344084,-3.22717358835541,
3.35039044581944));
#53612=CARTESIAN_POINT('Ctrl Pts',(-92.8739393027109,-4.56322461995675,
-0.903740325888789));
#53613=CARTESIAN_POINT('Ctrl Pts',(-92.6750657710135,-1.70657550119789,
-4.3275126305452));
#53614=CARTESIAN_POINT('Ctrl Pts',(-92.4761922393159,2.71807869212624,-3.7751574446937));
#53615=CARTESIAN_POINT('Ctrl Pts',(-92.2773187076185,4.64535660216838,0.245820152769577));
#53616=CARTESIAN_POINT('Ctrl Pts',(-92.0784451759211,2.30447132795495,4.04093768913237));
#53617=CARTESIAN_POINT('Ctrl Pts',(-91.8795716442236,-2.15376693409124,
4.12323337957387));
#53618=CARTESIAN_POINT('Ctrl Pts',(-91.6806981125262,-4.63311971482384,
0.417093774740931));
#53619=CARTESIAN_POINT('Ctrl Pts',(-91.4818245808287,-2.8555525885187,-3.67227244673119));
#53620=CARTESIAN_POINT('Ctrl Pts',(-91.2829510491312,1.54570211934521,-4.38754720397043));
#53621=CARTESIAN_POINT('Ctrl Pts',(-91.0840775174339,4.52676254620699,-1.07153458137132));
#53622=CARTESIAN_POINT('Ctrl Pts',(-90.8852039857363,3.34862425093643,3.22900621474431));
#53623=CARTESIAN_POINT('Ctrl Pts',(-90.686330454039,-0.9062368817328,4.562729470723));
#53624=CARTESIAN_POINT('Ctrl Pts',(-90.4874569223414,-4.32844570671463,
1.70420752047416));
#53625=CARTESIAN_POINT('Ctrl Pts',(-90.288583390644,-3.77366972888823,-2.72014379878889));
#53626=CARTESIAN_POINT('Ctrl Pts',(-90.0897098589466,0.248361744213206,
-4.64522141052807));
#53627=CARTESIAN_POINT('Ctrl Pts',(-89.8908363272491,4.04219793677718,-2.30226005236837));
#53628=CARTESIAN_POINT('Ctrl Pts',(-89.6919627955516,4.12205436529617,2.15602256907477));
#53629=CARTESIAN_POINT('Ctrl Pts',(-89.4930892638543,0.414558779279898,
4.63334722715004));
#53630=CARTESIAN_POINT('Ctrl Pts',(-89.2942157321566,-3.67383426434092,
2.8535429393951));
#53631=CARTESIAN_POINT('Ctrl Pts',(-89.0953422004594,-4.38670084250218,
-1.54810246017749));
#53632=CARTESIAN_POINT('Ctrl Pts',(-88.8964686687618,-1.06905767947995,
-4.52734814066269));
#53633=CARTESIAN_POINT('Ctrl Pts',(-88.6975951370643,3.23083787451525,-3.34685705362729));
#53634=CARTESIAN_POINT('Ctrl Pts',(-88.498721605367,4.56223295561509,0.908733166290631));
#53635=CARTESIAN_POINT('Ctrl Pts',(-88.2998480736694,1.70183902958803,4.32937748714383));
#53636=CARTESIAN_POINT('Ctrl Pts',(-88.1009745419721,-2.7222080911639,3.77218088341728));
#53637=CARTESIAN_POINT('Ctrl Pts',(-87.9021010102746,-4.64508482831926,
-0.250903261308599));
#53638=CARTESIAN_POINT('Ctrl Pts',(-87.703227478577,-2.30004808758962,-4.04345697437135));
#53639=CARTESIAN_POINT('Ctrl Pts',(-87.5043539468797,2.15827755864299,-4.12087411706242));
#53640=CARTESIAN_POINT('Ctrl Pts',(-87.3054804151822,4.63357335246232,-0.412023659718792));
#53641=CARTESIAN_POINT('Ctrl Pts',(-87.1066068834848,2.85153243605024,3.67539498217135));
#53642=CARTESIAN_POINT('Ctrl Pts',(-86.9077333517873,-1.55050233757813,
4.38585316785479));
#53643=CARTESIAN_POINT('Ctrl Pts',(-86.7088598200898,-4.52793237983578,
1.06658045756125));
#53644=CARTESIAN_POINT('Ctrl Pts',(-86.5099862883923,-3.34508885442102,
-3.2326685671199));
#53645=CARTESIAN_POINT('Ctrl Pts',(-86.311112756695,0.911229178814921,-4.56173507478168));
#53646=CARTESIAN_POINT('Ctrl Pts',(-86.1122392249975,4.33030797155388,-1.69947002924852));
#53647=CARTESIAN_POINT('Ctrl Pts',(-85.9133656933001,3.77069090872654,2.72427156863332));
#53648=CARTESIAN_POINT('Ctrl Pts',(-85.7144921616024,-0.253444703294882,
4.64494685558281));
#53649=CARTESIAN_POINT('Ctrl Pts',(-85.5156186299052,-4.04471480153795,
2.29783543428091));
#53650=CARTESIAN_POINT('Ctrl Pts',(-85.3167450982075,-4.119692635226,-2.16053190212079));
#53651=CARTESIAN_POINT('Ctrl Pts',(-85.1178715665103,-0.409488416816509,
-4.63379809069301));
#53652=CARTESIAN_POINT('Ctrl Pts',(-84.9189980348126,3.67695459975529,-2.84952107908597));
#53653=CARTESIAN_POINT('Ctrl Pts',(-84.7201245031154,4.38500418028194,1.55290175082866));
#53654=CARTESIAN_POINT('Ctrl Pts',(-84.5212509714178,1.0641029163568,4.5285152635514));
#53655=CARTESIAN_POINT('Ctrl Pts',(-84.3223774397204,-3.23449829201034,
3.34331965384694));
#53656=CARTESIAN_POINT('Ctrl Pts',(-84.1235039080229,-4.56123582837174,
-0.913724918558631));
#53657=CARTESIAN_POINT('Ctrl Pts',(-83.9246303763255,-1.69710052016476,
-4.33123715966623));
#53658=CARTESIAN_POINT('Ctrl Pts',(-83.7257568446281,2.72633423057952,-3.76919980526202));
#53659=CARTESIAN_POINT('Ctrl Pts',(-83.5268833129305,4.64480749236006,0.255986069411427));
#53660=CARTESIAN_POINT('Ctrl Pts',(-83.3280097812332,2.29562209310443,4.04597141790051));
#53661=CARTESIAN_POINT('Ctrl Pts',(-83.1291362495355,-2.16278559883345,
4.11850992014049));
#53662=CARTESIAN_POINT('Ctrl Pts',(-82.9302627178384,-4.63402144177481,
0.406953051331925));
#53663=CARTESIAN_POINT('Ctrl Pts',(-82.7313891861407,-2.84750886910435,
-3.67851311662592));
#53664=CARTESIAN_POINT('Ctrl Pts',(-82.5325156544434,1.55530069921097,-4.38415388003783));
#53665=CARTESIAN_POINT('Ctrl Pts',(-82.3336421227458,4.52909679163504,-1.06162505660813));
#53666=CARTESIAN_POINT('Ctrl Pts',(-82.1347685910484,3.34154945243463,3.23632704863876));
#53667=CARTESIAN_POINT('Ctrl Pts',(-81.935895059351,-0.916220384774566,
4.56073521653479));
#53668=CARTESIAN_POINT('Ctrl Pts',(-81.7370215276534,-4.33216505120267,
1.69473050304614));
#53669=CARTESIAN_POINT('Ctrl Pts',(-81.5381479959561,-3.76770757347015,
-2.7283960763849));
#53670=CARTESIAN_POINT('Ctrl Pts',(-81.3392744642586,0.25852735889732,-4.64466673869274));
#53671=CARTESIAN_POINT('Ctrl Pts',(-81.1404009325611,4.04722682308283,-2.29340806472287));
#53672=CARTESIAN_POINT('Ctrl Pts',(-80.9415274008637,4.11732597216001,2.16503864810625));
#53673=CARTESIAN_POINT('Ctrl Pts',(-80.7426538691662,0.404417564024095,
4.63424340564085));
#53674=CARTESIAN_POINT('Ctrl Pts',(-80.5437803374688,-3.6800705323166,2.84549580670783));
#53675=CARTESIAN_POINT('Ctrl Pts',(-80.3449068057713,-4.38330226737701,
-1.5576991820068));
#53676=CARTESIAN_POINT('Ctrl Pts',(-80.1460332740738,-1.05914687905708,
-4.52967696391263));
#53677=CARTESIAN_POINT('Ctrl Pts',(-79.9471597423764,3.23815483645772,-3.33977825071404));
#53678=CARTESIAN_POINT('Ctrl Pts',(-79.7482862106789,4.56023323942065,0.918715576715648));
#53679=CARTESIAN_POINT('Ctrl Pts',(-79.5494126789815,1.69235997860213,4.33309164588549));
#53680=CARTESIAN_POINT('Ctrl Pts',(-79.350539147284,-2.73045710543234,3.7662142137976));
#53681=CARTESIAN_POINT('Ctrl Pts',(-79.1516656155867,-4.64452459462294,
-0.261068570991888));
#53682=CARTESIAN_POINT('Ctrl Pts',(-78.9527920838891,-2.29119334979902,
-4.04848101670905));
#53683=CARTESIAN_POINT('Ctrl Pts',(-78.7539185521917,2.16729104926462,-4.11614079163897));
#53684=CARTESIAN_POINT('Ctrl Pts',(-78.5550450204942,4.63446398222474,-0.401881955652068));
#53685=CARTESIAN_POINT('Ctrl Pts',(-78.3561714887967,2.84348189249898,3.68162684636119));
#53686=CARTESIAN_POINT('Ctrl Pts',(-78.1572979570994,-1.56009719849821,
4.38244934255435));
#53687=CARTESIAN_POINT('Ctrl Pts',(-77.9584244254017,-4.53025578021044,
1.05666838444556));
#53688=CARTESIAN_POINT('Ctrl Pts',(-77.7595508937045,-3.33800604921544,
-3.23998165491997));
#53689=CARTESIAN_POINT('Ctrl Pts',(-77.5606773620069,0.921210493634929,
-4.55972989717965));
#53690=CARTESIAN_POINT('Ctrl Pts',(-77.3618038303096,4.33401694343732,-1.68998894754233));
#53691=CARTESIAN_POINT('Ctrl Pts',(-77.162930298612,3.76471972669138,2.73251731710484));
#53692=CARTESIAN_POINT('Ctrl Pts',(-76.9640567669146,-0.263609704934334,
4.64438106019319));
#53693=CARTESIAN_POINT('Ctrl Pts',(-76.7651832352171,-4.04973399840377,
2.28897794899589));
#53694=CARTESIAN_POINT('Ctrl Pts',(-76.5663097035197,-4.11495437893218,
-2.16954280163448));
#53695=CARTESIAN_POINT('Ctrl Pts',(-76.3674361718222,-0.399346226974714,
-4.63468317146038));
#53696=CARTESIAN_POINT('Ctrl Pts',(-76.1685626401248,3.68318205829376,-2.84146712708065));
#53697=CARTESIAN_POINT('Ctrl Pts',(-75.9696891084273,4.38159510582523,1.56249474796727));
#53698=CARTESIAN_POINT('Ctrl Pts',(-75.7708155767298,1.05418957351549,4.53083324035525));
#53699=CARTESIAN_POINT('Ctrl Pts',(-75.5719420450326,-3.24180750347881,
3.33623284846929));
#53700=CARTESIAN_POINT('Ctrl Pts',(-75.3730685133348,-4.55922518996239,
-0.923705134785675));
#53701=CARTESIAN_POINT('Ctrl Pts',(-75.1741949816376,-1.68761741057648,
-4.33494094358115));
#53702=CARTESIAN_POINT('Ctrl Pts',(-74.97532144994,2.7345767107856,-3.76322411259891));
#53703=CARTESIAN_POINT('Ctrl Pts',(-74.7764479182426,4.64423613544655,0.266150759963972));
#53704=CARTESIAN_POINT('Ctrl Pts',(-74.5775743865452,2.2867618629766,4.05098576779194));
#53705=CARTESIAN_POINT('Ctrl Pts',(-74.3787008548477,-2.17179390454168,
4.11376673439473));
#53706=CARTESIAN_POINT('Ctrl Pts',(-74.1798273231502,-4.63490097328221,
0.396810378751233));
#53707=CARTESIAN_POINT('Ctrl Pts',(-73.9809537914528,-2.839451511056,-3.68473616764873));
#53708=CARTESIAN_POINT('Ctrl Pts',(-73.7820802597553,1.56489182969629,-4.38073955744536));
#53709=CARTESIAN_POINT('Ctrl Pts',(-73.5832067280579,4.53140934417422,-1.0517104470089));
#53710=CARTESIAN_POINT('Ctrl Pts',(-73.3843331963604,3.33445864900637,3.24363238158761));
#53711=CARTESIAN_POINT('Ctrl Pts',(-73.185459664663,-0.926199499420982,
4.55871911791998));
#53712=CARTESIAN_POINT('Ctrl Pts',(-72.9865861329655,-4.33586364604029,
1.68524536841465));
#53713=CARTESIAN_POINT('Ctrl Pts',(-72.7877126012681,-3.76172737196798,
-2.73663528585817));
#53714=CARTESIAN_POINT('Ctrl Pts',(-72.5888390695705,0.268691735320179,
-4.64408982042635));
#53715=CARTESIAN_POINT('Ctrl Pts',(-72.3899655378732,4.05223632449878,-2.28454509240455));
#53716=CARTESIAN_POINT('Ctrl Pts',(-72.1910920061757,4.11257785838219,2.1740443573123));
#53717=CARTESIAN_POINT('Ctrl Pts',(-71.9922184744783,0.394274411740812,
4.63511738762496));
#53718=CARTESIAN_POINT('Ctrl Pts',(-71.7933449427808,-3.68628917396088,
2.8374350450285));
#53719=CARTESIAN_POINT('Ctrl Pts',(-71.5944714110833,-4.37988269767089,
-1.56728844296773));
#53720=CARTESIAN_POINT('Ctrl Pts',(-71.3955978793859,-1.04923100566787,
-4.53198409149484));
#53721=CARTESIAN_POINT('Ctrl Pts',(-71.1967243476885,3.2454562887,-3.33268345135785));
#53722=CARTESIAN_POINT('Ctrl Pts',(-70.9978508159909,4.55821168120396,0.928693586794169));
#53723=CARTESIAN_POINT('Ctrl Pts',(-70.7989772842936,1.68287282176677,4.33678505053868));
#53724=CARTESIAN_POINT('Ctrl Pts',(-70.6001037525961,-2.73869304170636,
3.76022950524648));
#53725=CARTESIAN_POINT('Ctrl Pts',(-70.4012302208986,-4.64394211517639,
-0.271232630242302));
#53726=CARTESIAN_POINT('Ctrl Pts',(-70.2023566892012,-2.28232763794338,
-4.0534856681499));
#53727=CARTESIAN_POINT('Ctrl Pts',(-70.0034831575037,2.17629415927268,-4.11138775125048));
#53728=CARTESIAN_POINT('Ctrl Pts',(-69.8046096258063,4.63533241442395,-0.391738326702473));
#53729=CARTESIAN_POINT('Ctrl Pts',(-69.6057360941088,2.83541772960161,3.68784107676536));
#53730=CARTESIAN_POINT('Ctrl Pts',(-69.4068625624114,-1.56968458706416,
4.37902452675825));
#53731=CARTESIAN_POINT('Ctrl Pts',(-69.2079890307139,-4.53255748214502,
1.04675125023471));
#53732=CARTESIAN_POINT('Ctrl Pts',(-69.0091154990165,-3.33090725605517,
-3.24727922427005));
#53733=CARTESIAN_POINT('Ctrl Pts',(-68.8102419673191,0.931187396158665,
-4.55770287996621));
#53734=CARTESIAN_POINT('Ctrl Pts',(-68.6113684356214,4.33770515680041,-1.6804997713431));
#53735=CARTESIAN_POINT('Ctrl Pts',(-68.4124949039242,3.75873051288291,2.74074997771414));
#53736=CARTESIAN_POINT('Ctrl Pts',(-68.2136213722265,-0.273773443969652,
4.64379301974085));
#53737=CARTESIAN_POINT('Ctrl Pts',(-68.0147478405293,-4.05473379837136,
2.2801095002569));
#53738=CARTESIAN_POINT('Ctrl Pts',(-67.8158743088316,-4.11019641335586,
-2.17854330974936));
#53739=CARTESIAN_POINT('Ctrl Pts',(-67.6170007771344,-0.389202124395414,
-4.63554605361474));
#53740=CARTESIAN_POINT('Ctrl Pts',(-67.4181272454367,3.68939187559753,-2.83339956537932));
#53741=CARTESIAN_POINT('Ctrl Pts',(-67.2192537137394,4.37816504496438,1.57208026126815));
#53742=CARTESIAN_POINT('Ctrl Pts',(-67.0203801820419,1.04427118145181,4.53312951595323));
#53743=CARTESIAN_POINT('Ctrl Pts',(-66.8215066503444,-3.24910118775209,
3.32913006362999));
#53744=CARTESIAN_POINT('Ctrl Pts',(-66.622633118647,-4.55719271435901,-0.933680926767934));
#53745=CARTESIAN_POINT('Ctrl Pts',(-66.4237595869495,-1.67812621785408,
-4.33862396455001));
#53746=CARTESIAN_POINT('Ctrl Pts',(-66.2248860552522,2.74280609326566,-3.757230395326));
#53747=CARTESIAN_POINT('Ctrl Pts',(-66.0260125235546,4.64364253416446,0.276314175741591));
#53748=CARTESIAN_POINT('Ctrl Pts',(-65.8271389918572,2.27789068000911,4.05598071478954));
#53749=CARTESIAN_POINT('Ctrl Pts',(-65.6282654601598,-2.18079180806907,
4.10900384505489));
#53750=CARTESIAN_POINT('Ctrl Pts',(-65.4293919284622,-4.63575830513335,
0.38666580557894));
#53751=CARTESIAN_POINT('Ctrl Pts',(-65.2305183967649,-2.83138055296581,
-3.6909415699932));
#53752=CARTESIAN_POINT('Ctrl Pts',(-65.0316448650673,1.57447546486273,-4.37730425254658));
#53753=CARTESIAN_POINT('Ctrl Pts',(-64.83277133337,4.53370019274813,-1.0417908000614));
#53754=CARTESIAN_POINT('Ctrl Pts',(-64.6338978016724,3.32735187461431,3.25092217860068));
#53755=CARTESIAN_POINT('Ctrl Pts',(-64.435024269975,-0.936174177875471,
4.55668118453508));
#53756=CARTESIAN_POINT('Ctrl Pts',(-64.2361507382776,-4.33954147351247,
1.67575216201024));
#53757=CARTESIAN_POINT('Ctrl Pts',(-64.03727720658,-3.75572915302483,-2.74486138774556));
#53758=CARTESIAN_POINT('Ctrl Pts',(-63.8384036748827,0.27885482479771,-4.64349065849217));
#53759=CARTESIAN_POINT('Ctrl Pts',(-63.6395301431852,4.05722641703115,-2.27567117786416));
#53760=CARTESIAN_POINT('Ctrl Pts',(-63.4406566114878,4.10781004670463,2.18303965355862));
#53761=CARTESIAN_POINT('Ctrl Pts',(-63.2417830797902,0.384129371012292,
4.63596916891631));
#53762=CARTESIAN_POINT('Ctrl Pts',(-63.0429095480929,-3.69249015948847,
2.82936069296544));
#53763=CARTESIAN_POINT('Ctrl Pts',(-62.8440360163953,-4.37644214976249,
-1.57687019713081));
#53764=CARTESIAN_POINT('Ctrl Pts',(-62.645162484698,-1.03931010680609,-4.53426951235894));
#53765=CARTESIAN_POINT('Ctrl Pts',(-62.4462889530004,3.25274219627064,-3.32557268954045));
#53766=CARTESIAN_POINT('Ctrl Pts',(-62.247415421303,4.5561682906476,0.938667148734915));
#53767=CARTESIAN_POINT('Ctrl Pts',(-62.0485418896056,1.67337760452224,4.34045768341317));
#53768=CARTESIAN_POINT('Ctrl Pts',(-61.8496683579081,-2.74691586053853,
3.75422678642872));
#53769=CARTESIAN_POINT('Ctrl Pts',(-61.6507948262107,-4.64333739276948,
-0.2813953903773));
#53770=CARTESIAN_POINT('Ctrl Pts',(-61.4519212945132,-2.2734509944866,-4.0584709047232));
#53771=CARTESIAN_POINT('Ctrl Pts',(-61.2530477628157,2.18528684554512,-4.10661501866251));
#53772=CARTESIAN_POINT('Ctrl Pts',(-61.0541742311184,4.63617864490049,-0.381592821454718));
#53773=CARTESIAN_POINT('Ctrl Pts',(-60.8553006994208,2.82733998598282,3.69403764361975));
#53774=CARTESIAN_POINT('Ctrl Pts',(-60.6564271677235,-1.57926445735542,
4.37557873687019));
#53775=CARTESIAN_POINT('Ctrl Pts',(-60.4575536360258,-4.53483747461512,
1.03682910242867));
#53776=CARTESIAN_POINT('Ctrl Pts',(-60.2586801043286,-3.32379250894121,
-3.25456124021708));
#53777=CARTESIAN_POINT('Ctrl Pts',(-60.059806572631,0.941159838599904,-4.55565403285013));
#53778=CARTESIAN_POINT('Ctrl Pts',(-59.8609330409336,4.34137259397775,-1.67100254610099));
#53779=CARTESIAN_POINT('Ctrl Pts',(-59.6620595092361,3.75272329598755,2.74896951102943));
#53780=CARTESIAN_POINT('Ctrl Pts',(-59.4631859775387,-0.283935871719825,
4.64318273704232));
#53781=CARTESIAN_POINT('Ctrl Pts',(-59.2643124458413,-4.05971417749329,
2.27123013054094));
#53782=CARTESIAN_POINT('Ctrl Pts',(-59.0654389141437,-4.10541876128613,
-2.18753338335589));
#53783=CARTESIAN_POINT('Ctrl Pts',(-58.8665653824463,-0.379056157665712,
-4.63638673302307));
#53784=CARTESIAN_POINT('Ctrl Pts',(-58.6676918507489,3.69558402192361,-2.82531843262312));
#53785=CARTESIAN_POINT('Ctrl Pts',(-58.4688183190514,4.37471401412829,1.58165824481985));
#53786=CARTESIAN_POINT('Ctrl Pts',(-58.269944787354,1.03434778767158,4.53540407934683));
#53787=CARTESIAN_POINT('Ctrl Pts',(-58.0710712556565,-3.25637930989572,
3.32201133334915));
#53788=CARTESIAN_POINT('Ctrl Pts',(-57.872197723959,-4.5551384112965,-0.94365224672451));
#53789=CARTESIAN_POINT('Ctrl Pts',(-57.6733241922616,-1.66862698745729,
-4.34228620493241));
#53790=CARTESIAN_POINT('Ctrl Pts',(-57.4744506605641,2.75102233860371,-3.75121868215123));
#53791=CARTESIAN_POINT('Ctrl Pts',(-57.2755771288667,4.64302669135687,0.286476268064849));
#53792=CARTESIAN_POINT('Ctrl Pts',(-57.0767035971692,2.26900858669214,4.06095623496905));
#53793=CARTESIAN_POINT('Ctrl Pts',(-56.8778300654718,-2.18977926631837,
4.1042212749338));
#53794=CARTESIAN_POINT('Ctrl Pts',(-56.6789565337743,-4.63659343322196,
0.376519380404392));
#53795=CARTESIAN_POINT('Ctrl Pts',(-56.4800830020769,-2.82329603349106,
-3.69712929393748));
#53796=CARTESIAN_POINT('Ctrl Pts',(-56.2812094703794,1.58405155880773,-4.37384798179542));
#53797=CARTESIAN_POINT('Ctrl Pts',(-56.0823359386819,4.53596932638436,-1.03186616327761));
#53798=CARTESIAN_POINT('Ctrl Pts',(-55.8834624069846,3.32022916329763,3.25819640476215));
#53799=CARTESIAN_POINT('Ctrl Pts',(-55.684588875287,-0.946144372362453,
4.55462142614115));
#53800=CARTESIAN_POINT('Ctrl Pts',(-55.4857153435897,-4.34319851600362,
1.66625092930237));
#53801=CARTESIAN_POINT('Ctrl Pts',(-55.286841811892,-3.74971294537027,-2.75307434264664));
#53802=CARTESIAN_POINT('Ctrl Pts',(-55.0879682801948,0.289016578651858,
-4.64286925575996));
#53803=CARTESIAN_POINT('Ctrl Pts',(-54.8890947484972,4.0621970767789,-2.26678636360509));
#53804=CARTESIAN_POINT('Ctrl Pts',(-54.6902212167999,4.10302255996373,2.19202449376046));
#53805=CARTESIAN_POINT('Ctrl Pts',(-54.4913476851023,0.373982490430176,
4.63679874543512));
#53806=CARTESIAN_POINT('Ctrl Pts',(-54.292474153405,-3.69867345919861,2.82127278919229));
#53807=CARTESIAN_POINT('Ctrl Pts',(-54.0936006217074,-4.37298064013094,
-1.58644439860245));
#53808=CARTESIAN_POINT('Ctrl Pts',(-53.89472709001,-1.02938422998975,-4.5365332155585));
#53809=CARTESIAN_POINT('Ctrl Pts',(-53.6958535583125,3.26001252427244,-3.31844599932015));
#53810=CARTESIAN_POINT('Ctrl Pts',(-53.496980026615,4.55410307753876,0.948636214767613));
#53811=CARTESIAN_POINT('Ctrl Pts',(-53.2981064949176,1.66387437234772,4.34410952691816));
#53812=CARTESIAN_POINT('Ctrl Pts',(-53.0992329632202,-2.75512552254401,
3.74820608609554));
#53813=CARTESIAN_POINT('Ctrl Pts',(-52.9003594315228,-4.64271043029872,
-0.291556802720443));
#53814=CARTESIAN_POINT('Ctrl Pts',(-52.7014858998252,-2.26456346194496,
-4.06343670255129));
#53815=CARTESIAN_POINT('Ctrl Pts',(-52.5026123681279,2.19426906500987,-4.10182261673488));
#53816=CARTESIAN_POINT('Ctrl Pts',(-52.3037388364303,4.63700266960115,-0.371445488502572));
#53817=CARTESIAN_POINT('Ctrl Pts',(-52.1048653047329,2.81924870033247,3.70021651724473));
#53818=CARTESIAN_POINT('Ctrl Pts',(-51.9059917730354,-1.58883676348771,
4.37211198939449));
#53819=CARTESIAN_POINT('Ctrl Pts',(-51.707118241338,-4.53709574670044,1.02690198855093));
#53820=CARTESIAN_POINT('Ctrl Pts',(-51.5082447096406,-3.31666184195056,
-3.2618276678828));
#53821=CARTESIAN_POINT('Ctrl Pts',(-51.309371177943,0.951127773194121,-4.55358336564463));
#53822=CARTESIAN_POINT('Ctrl Pts',(-51.1104976462456,4.34501923740356,-1.66149731730449));
#53823=CARTESIAN_POINT('Ctrl Pts',(-50.9116241145482,3.74669810477784,2.75717587768194));
#53824=CARTESIAN_POINT('Ctrl Pts',(-50.7127505828507,-0.294096939510222,
4.64255021502059));
#53825=CARTESIAN_POINT('Ctrl Pts',(-50.5138770511534,-4.06467511191512,
2.2623398823773));
#53826=CARTESIAN_POINT('Ctrl Pts',(-50.3150035194557,-4.10062144560646,
-2.19651297939471));
#53827=CARTESIAN_POINT('Ctrl Pts',(-50.1161299877585,-0.368908375381047,
-4.63720520565898));
#53828=CARTESIAN_POINT('Ctrl Pts',(-49.9172564560607,3.70175846761393,-2.81722376751752));
#53829=CARTESIAN_POINT('Ctrl Pts',(-49.7183829243636,4.37124202984609,1.59122865274734));
#53830=CARTESIAN_POINT('Ctrl Pts',(-49.5195093926659,1.02441943970435,4.53765691964172));
#53831=CARTESIAN_POINT('Ctrl Pts',(-49.3206358609686,-3.26364183505,3.31487669172296));
#53832=CARTESIAN_POINT('Ctrl Pts',(-49.1217623292711,-4.55306229061429,
-0.953619046896171));
#53833=CARTESIAN_POINT('Ctrl Pts',(-48.9228887975736,-1.65911976488428,
-4.34592764718735));
#53834=CARTESIAN_POINT('Ctrl Pts',(-48.7240152658762,2.75922540744653,-3.74518900186874));
#53835=CARTESIAN_POINT('Ctrl Pts',(-48.5251417341786,4.6423886099736,0.296636988260731));
#53836=CARTESIAN_POINT('Ctrl Pts',(-48.3262682024814,2.26011562556773,4.06591230449965));
#53837=CARTESIAN_POINT('Ctrl Pts',(-48.1273946707837,-2.19875623624322,
4.09941904693807));
#53838=CARTESIAN_POINT('Ctrl Pts',(-47.9285211390865,-4.63740635354801,
0.366371151825084));
#53839=CARTESIAN_POINT('Ctrl Pts',(-47.7296476073888,-2.81519799135364,
-3.70329930984454));
#53840=CARTESIAN_POINT('Ctrl Pts',(-47.5307740756915,1.59362006566512,-4.37037076174621));
#53841=CARTESIAN_POINT('Ctrl Pts',(-47.331900543994,4.53821673421451,-1.02193658419319));
#53842=CARTESIAN_POINT('Ctrl Pts',(-47.1330270122966,3.31309054917171,3.26545502523097));
#53843=CARTESIAN_POINT('Ctrl Pts',(-46.934153480599,-0.956110035128021,
4.55253985260366));
#53844=CARTESIAN_POINT('Ctrl Pts',(-46.7352799489017,-4.34683475599761,
1.65674171579889));
#53845=CARTESIAN_POINT('Ctrl Pts',(-46.5364064172041,-3.74367877782001,
-2.76127411122423));
#53846=CARTESIAN_POINT('Ctrl Pts',(-46.3375328855068,0.299176948211582,
-4.64222561520612));
#53847=CARTESIAN_POINT('Ctrl Pts',(-46.1386593538092,4.06714827993455,-2.2578906921821));
#53848=CARTESIAN_POINT('Ctrl Pts',(-45.9397858221119,4.09821542108963,2.20099883488389));
#53849=CARTESIAN_POINT('Ctrl Pts',(-45.7409122904143,0.363833818594308,
4.63760611320794));
#53850=CARTESIAN_POINT('Ctrl Pts',(-45.542038758717,-3.7048390434754,2.81317137244729));
#53851=CARTESIAN_POINT('Ctrl Pts',(-45.3431652270194,-4.36949818535569,
-1.5960110015255));
#53852=CARTESIAN_POINT('Ctrl Pts',(-45.1442916953221,-1.01945342276039,
-4.53877519025113));
#53853=CARTESIAN_POINT('Ctrl Pts',(-44.9454181636245,3.2672672378829,-3.3113034148314));
#53854=CARTESIAN_POINT('Ctrl Pts',(-44.7465446319271,4.55201605176918,0.958600737143906));
#53855=CARTESIAN_POINT('Ctrl Pts',(-44.5476711002296,1.65436317076021,4.34774056356279));
#53856=CARTESIAN_POINT('Ctrl Pts',(-44.3487975685322,-2.76332198840176,
3.74216743308372));
#53857=CARTESIAN_POINT('Ctrl Pts',(-44.1499240368347,-4.64206123076694,
-0.301716818602429));
#53858=CARTESIAN_POINT('Ctrl Pts',(-43.9510505051373,-2.25566508288644,
-4.0683830378498));
#53859=CARTESIAN_POINT('Ctrl Pts',(-43.7521769734398,2.20324077464528,-4.09701056842145));
#53860=CARTESIAN_POINT('Ctrl Pts',(-43.5533034417424,4.6378044845791,-0.361296376448224));
#53861=CARTESIAN_POINT('Ctrl Pts',(-43.3544299100449,2.81114391140508,3.70637766804561));
#53862=CARTESIAN_POINT('Ctrl Pts',(-43.1555563783475,-1.59840145961267,
4.36862430093561));
#53863=CARTESIAN_POINT('Ctrl Pts',(-42.9566828466501,-4.53933228758441,
1.0169699561495));
#53864=CARTESIAN_POINT('Ctrl Pts',(-42.7578093149525,-3.3095152892371,-3.26907847246329));
#53865=CARTESIAN_POINT('Ctrl Pts',(-42.5589357832552,0.961091152198231,
-4.55149088826764));
#53866=CARTESIAN_POINT('Ctrl Pts',(-42.3600622515576,4.34864506961174,-1.65198413048027));
#53867=CARTESIAN_POINT('Ctrl Pts',(-42.1611887198603,3.74065496811231,2.76536903836609));
#53868=CARTESIAN_POINT('Ctrl Pts',(-41.9623151881627,-0.304256598672874,
4.64189545670523));
#53869=CARTESIAN_POINT('Ctrl Pts',(-41.7634416564653,-4.06961657787565,
2.25343879834717));
#53870=CARTESIAN_POINT('Ctrl Pts',(-41.5645681247679,-4.09580448929436,
-2.20548205485632));
#53871=CARTESIAN_POINT('Ctrl Pts',(-41.3656945930703,-0.358758826146377,
-4.63800146760209));
#53872=CARTESIAN_POINT('Ctrl Pts',(-41.166821061373,3.70791518309455,-2.80911560883385));
#53873=CARTESIAN_POINT('Ctrl Pts',(-40.9679475296754,4.36774910874765,1.60079143921098));
#53874=CARTESIAN_POINT('Ctrl Pts',(-40.7690739979781,1.01448618510396,4.53988802604759));
#53875=CARTESIAN_POINT('Ctrl Pts',(-40.5702004662805,-3.27088872842992,
3.30772617292411));
#53876=CARTESIAN_POINT('Ctrl Pts',(-40.3713269345831,-4.55096436225627,
-0.963581279545481));
#53877=CARTESIAN_POINT('Ctrl Pts',(-40.1724534028856,-1.64960459567123,
-4.34954827387366));
#53878=CARTESIAN_POINT('Ctrl Pts',(-39.9735798711882,2.7674152605043,-3.73914138335856));
#53879=CARTESIAN_POINT('Ctrl Pts',(-39.7747063394908,4.6417282930707,0.306796287662675));
#53880=CARTESIAN_POINT('Ctrl Pts',(-39.5758328077933,2.25121183923051,4.0708488996431));
#53881=CARTESIAN_POINT('Ctrl Pts',(-39.3769592760958,-2.20772267484625,
4.09459718406912));
#53882=CARTESIAN_POINT('Ctrl Pts',(-39.1780857443984,-4.63819706221785,
0.356221168448329));
#53883=CARTESIAN_POINT('Ctrl Pts',(-38.979212212701,-2.80708646534088,-3.70945158816194));
#53884=CARTESIAN_POINT('Ctrl Pts',(-38.7803386810035,1.60318093960496,-4.36687260905381));
#53885=CARTESIAN_POINT('Ctrl Pts',(-38.5814651493061,4.5404424054743,-1.01200211036728));
#53886=CARTESIAN_POINT('Ctrl Pts',(-38.3825916176086,3.30593606642799,3.27269800524089));
#53887=CARTESIAN_POINT('Ctrl Pts',(-38.1837180859111,-0.966071118440219,
4.55043647389266));
#53888=CARTESIAN_POINT('Ctrl Pts',(-37.9848445542137,-4.35045017607815,
1.64722456704551));
#53889=CARTESIAN_POINT('Ctrl Pts',(-37.7859710225162,-3.73762667927559,
-2.76946065420398));
#53890=CARTESIAN_POINT('Ctrl Pts',(-37.5870974908188,0.309335884811614,
-4.64155973991339));
#53891=CARTESIAN_POINT('Ctrl Pts',(-37.3882239591213,4.07208000278311,-2.2489842062031));
#53892=CARTESIAN_POINT('Ctrl Pts',(-37.1893504274239,4.0933886531073,2.20996263394419));
#53893=CARTESIAN_POINT('Ctrl Pts',(-36.9904768957264,0.353683404113827,
4.6383912683679));
#53894=CARTESIAN_POINT('Ctrl Pts',(-36.791603364029,-3.71098688278783,2.80505648153359));
#53895=CARTESIAN_POINT('Ctrl Pts',(-36.5927298323315,-4.36599480211647,
-1.60556996007931));
#53896=CARTESIAN_POINT('Ctrl Pts',(-36.393856300634,-1.00951773268308,-4.54099542569859));
#53897=CARTESIAN_POINT('Ctrl Pts',(-36.1949827689366,3.27450630235449,-3.30414497028465));
#53898=CARTESIAN_POINT('Ctrl Pts',(-35.9961092372392,4.54990722333487,0.968560668136903));
#53899=CARTESIAN_POINT('Ctrl Pts',(-35.7972357055417,1.64484404531562,4.35135077595531));
#53900=CARTESIAN_POINT('Ctrl Pts',(-35.5983621738442,-2.77150521885286,
3.73611085631683));
#53901=CARTESIAN_POINT('Ctrl Pts',(-35.3994886421467,-4.64138979728367,
-0.311875389359506));
#53902=CARTESIAN_POINT('Ctrl Pts',(-35.2006151104494,-2.24675589993187,
-4.07330988692714));
#53903=CARTESIAN_POINT('Ctrl Pts',(-35.0017415787518,2.21220193147961,-4.09217889677064));
#53904=CARTESIAN_POINT('Ctrl Pts',(-34.8028680470544,4.63858408599405,-0.351145533902577));
#53905=CARTESIAN_POINT('Ctrl Pts',(-34.6039945153569,2.80302565801969,3.71252106651267));
#53906=CARTESIAN_POINT('Ctrl Pts',(-34.4051209836595,-1.60795849991889,
4.36511568819838));
#53907=CARTESIAN_POINT('Ctrl Pts',(-34.206247451962,-4.54154708655483,1.00703305279517));
#53908=CARTESIAN_POINT('Ctrl Pts',(-34.0073739202647,-3.30235288503029,
-3.27631361922951));
#53909=CARTESIAN_POINT('Ctrl Pts',(-33.8085003885671,0.971049927890603,
-4.54937661074138));
#53910=CARTESIAN_POINT('Ctrl Pts',(-33.6096268568697,4.35225007323551,-1.64246303119386));
#53911=CARTESIAN_POINT('Ctrl Pts',(-33.4107533251722,3.73459391493592,2.77354895383887));
#53912=CARTESIAN_POINT('Ctrl Pts',(-33.2118797934748,-0.314414800546058,
4.64121846523245));
#53913=CARTESIAN_POINT('Ctrl Pts',(-33.0130062617773,-4.07453855170703,
2.24452692108387));
#53914=CARTESIAN_POINT('Ctrl Pts',(-32.8141327300799,-4.09096791542132,
-2.21444056678213));
#53915=CARTESIAN_POINT('Ctrl Pts',(-32.6152591983824,-0.348607558574277,
-4.63877551503864));
#53916=CARTESIAN_POINT('Ctrl Pts',(-32.416385666685,3.71405413887715,-2.80099399540709));
#53917=CARTESIAN_POINT('Ctrl Pts',(-32.2175121349874,4.36423526756273,1.61034655840855));
#53918=CARTESIAN_POINT('Ctrl Pts',(-32.0186386032901,1.00454807144728,4.542097387878));
#53919=CARTESIAN_POINT('Ctrl Pts',(-31.8197650715926,-3.27811995532495,
3.30055981120134));
#53920=CARTESIAN_POINT('Ctrl Pts',(-31.6208915398952,-4.5488446362709,-0.973538896956091));
#53921=CARTESIAN_POINT('Ctrl Pts',(-31.4220180081977,-1.64008152539322,
-4.35314806764954));
#53922=CARTESIAN_POINT('Ctrl Pts',(-31.2231444765002,2.77559185855018,-3.73307585558706));
#53923=CARTESIAN_POINT('Ctrl Pts',(-31.0242709448028,4.64104574381103,0.316954117611085));
#53924=CARTESIAN_POINT('Ctrl Pts',(-30.8253974131053,2.24229727032636,4.07576599675497));
#53925=CARTESIAN_POINT('Ctrl Pts',(-30.6265238814079,-2.21667853918166,
4.08975570942184));
#53926=CARTESIAN_POINT('Ctrl Pts',(-30.4276503497104,-4.63896555544426,
0.346069478888772));
#53927=CARTESIAN_POINT('Ctrl Pts',(-30.228776818013,-2.79896149430411,-3.71558609942221));
#53928=CARTESIAN_POINT('Ctrl Pts',(-30.0299032863155,1.61273413483346,-4.3633535404732));
#53929=CARTESIAN_POINT('Ctrl Pts',(-29.8310297546181,4.54264632950338,-1.00206278938327));
#53930=CARTESIAN_POINT('Ctrl Pts',(-29.6321562229206,3.29876574933446,3.27992531010005));
#53931=CARTESIAN_POINT('Ctrl Pts',(-29.4332826912232,-0.976027574588195,
4.54831130008276));
#53932=CARTESIAN_POINT('Ctrl Pts',(-29.2344091595257,-4.35404475892857,
1.63769952862658));
#53933=CARTESIAN_POINT('Ctrl Pts',(-29.0355356278282,-3.73155667872468,
-2.77763393237523));
#53934=CARTESIAN_POINT('Ctrl Pts',(-28.8366620961308,0.319493339794431,
-4.6408716330711));
#53935=CARTESIAN_POINT('Ctrl Pts',(-28.6377885644333,4.07699222170351,-2.2400669483268));
#53936=CARTESIAN_POINT('Ctrl Pts',(-28.4389150327359,4.08854227913508,2.21891584800811));
#53937=CARTESIAN_POINT('Ctrl Pts',(-28.2400415010384,0.343531295605794,
4.63915420715415));
#53938=CARTESIAN_POINT('Ctrl Pts',(-28.041167969341,-3.71711694768952,2.79692815531905));
#53939=CARTESIAN_POINT('Ctrl Pts',(-27.8422944376435,-4.36247050719351,
-1.61512122847912));
#53940=CARTESIAN_POINT('Ctrl Pts',(-27.6434209059461,-0.999577207347043,
-4.54319391126653));
#53941=CARTESIAN_POINT('Ctrl Pts',(-27.4445473742487,3.28172968301435,-3.29697069996681));
#53942=CARTESIAN_POINT('Ctrl Pts',(-27.2456738425511,4.5477766023366,0.978515960041948));
#53943=CARTESIAN_POINT('Ctrl Pts',(-27.0468003108538,1.63531704160702,4.35494014680417));
#53944=CARTESIAN_POINT('Ctrl Pts',(-26.8479267791562,-2.77967517470273,
3.73003638480356));
#53945=CARTESIAN_POINT('Ctrl Pts',(-26.6490532474588,-4.6406961330648,-0.322032466335979));
#53946=CARTESIAN_POINT('Ctrl Pts',(-26.4501797157613,-2.23783595575289,
-4.0782172261855));
#53947=CARTESIAN_POINT('Ctrl Pts',(-26.2513061840639,2.22115249259184,-4.08732762492435));
#53948=CARTESIAN_POINT('Ctrl Pts',(-26.0524326523664,4.63934147011183,-0.340993009485119));
#53949=CARTESIAN_POINT('Ctrl Pts',(-25.853559120669,2.79489397906051,3.71864668322071));
#53950=CARTESIAN_POINT('Ctrl Pts',(-25.6546855889715,-1.61750783863076,
4.3615861679881));
#53951=CARTESIAN_POINT('Ctrl Pts',(-25.4558120572741,-4.5437401330036,0.997091326082762));
#53952=CARTESIAN_POINT('Ctrl Pts',(-25.2569385255766,-3.29517466363574,
-3.28353307352769));
#53953=CARTESIAN_POINT('Ctrl Pts',(-25.0580649938792,0.981004052572414,
-4.54724054319249));
#53954=CARTESIAN_POINT('Ctrl Pts',(-24.8591914621817,4.35583423100831,-1.63293406504773));
#53955=CARTESIAN_POINT('Ctrl Pts',(-24.6603179304843,3.72851497427881,2.78171558492152));
#53956=CARTESIAN_POINT('Ctrl Pts',(-24.4614443987868,-0.324571496475413,
4.64051924384463));
#53957=CARTESIAN_POINT('Ctrl Pts',(-24.2625708670894,-4.07944100983435,
2.23560429327258));
#53958=CARTESIAN_POINT('Ctrl Pts',(-24.0636973353919,-4.08611174715321,
-2.22338847226336));
#53959=CARTESIAN_POINT('Ctrl Pts',(-23.8648238036945,-0.338454621286521,
-4.63952734426114));
#53960=CARTESIAN_POINT('Ctrl Pts',(-23.665950271997,3.72017530555782,-2.79285896613754));
#53961=CARTESIAN_POINT('Ctrl Pts',(-23.4670767402996,4.3607005231217,1.61989396457395));
#53962=CARTESIAN_POINT('Ctrl Pts',(-23.2682032086021,0.994605146334582,
4.54428499455105));
#53963=CARTESIAN_POINT('Ctrl Pts',(-23.0693296769047,-3.28533548110023,
3.29337764087889));
#53964=CARTESIAN_POINT('Ctrl Pts',(-22.8704561452072,-4.5467031228109,-0.983491851434788));
#53965=CARTESIAN_POINT('Ctrl Pts',(-22.6715826135097,-1.63055059966216,
-4.35672701127326));
#53966=CARTESIAN_POINT('Ctrl Pts',(-22.4727090818123,2.7837551624209,-3.72699244760593));
#53967=CARTESIAN_POINT('Ctrl Pts',(-22.2738355501148,4.64034096546365,0.327110429452991));
#53968=CARTESIAN_POINT('Ctrl Pts',(-22.0749620184174,2.2333719615536,4.08066357228372));
#53969=CARTESIAN_POINT('Ctrl Pts',(-21.8760884867199,-2.2256237863533,4.08489464618556));
#53970=CARTESIAN_POINT('Ctrl Pts',(-21.6772149550225,-4.6397118295465,0.335916131769966));
#53971=CARTESIAN_POINT('Ctrl Pts',(-21.478341423325,-2.79082311715933,-3.72170281424325));
#53972=CARTESIAN_POINT('Ctrl Pts',(-21.2794678916276,1.6222796055944,-4.35981357285946));
#53973=CARTESIAN_POINT('Ctrl Pts',(-21.0805943599301,4.54482849574578,-0.992118668846749));
#53974=CARTESIAN_POINT('Ctrl Pts',(-20.8817208282327,3.29157963223422,3.2871369051924));
#53975=CARTESIAN_POINT('Ctrl Pts',(-20.6828472965352,-0.985979355884234,
4.54616434135269));
#53976=CARTESIAN_POINT('Ctrl Pts',(-20.4839737648377,-4.35761848733187,
1.62816664616376));
#53977=CARTESIAN_POINT('Ctrl Pts',(-20.2851002331403,-3.72546880524065,
-2.78579390659035));
#53978=CARTESIAN_POINT('Ctrl Pts',(-20.0862267014428,0.329649264508629,
-4.6401612979751));
#53979=CARTESIAN_POINT('Ctrl Pts',(-19.8873531697454,4.08188491316758,-2.2311389612644));
#53980=CARTESIAN_POINT('Ctrl Pts',(-19.6884796380479,4.08367632238581,2.22785843419248));
#53981=CARTESIAN_POINT('Ctrl Pts',(-19.4896061063505,0.33337754169537,4.63989492591268));
#53982=CARTESIAN_POINT('Ctrl Pts',(-19.290732574653,-3.72322920881974,2.78878643273532));
#53983=CARTESIAN_POINT('Ctrl Pts',(-19.0918590429556,-4.35892531746685,
-1.62466476097796));
#53984=CARTESIAN_POINT('Ctrl Pts',(-18.8929855112581,-0.989631894363675,
-4.54537063642502));
#53985=CARTESIAN_POINT('Ctrl Pts',(-18.6941119795606,3.28893734526478,-3.28978063824008));
#53986=CARTESIAN_POINT('Ctrl Pts',(-18.4952384478633,4.54562419897928,0.988466565176122));
#53987=CARTESIAN_POINT('Ctrl Pts',(-18.2963649161657,1.62578220526613,4.35850865891729));
#53988=CARTESIAN_POINT('Ctrl Pts',(-18.0974913844683,-2.78783181681954,
3.72394404763897));
#53989=CARTESIAN_POINT('Ctrl Pts',(-17.8986178527708,-4.63998024143282,
-0.332188000882232));
#53990=CARTESIAN_POINT('Ctrl Pts',(-17.6997443210734,-2.22890529307343,
-4.08310503212032));
#53991=CARTESIAN_POINT('Ctrl Pts',(-17.500870789376,2.23009241511192,-4.08245677611868));
#53992=CARTESIAN_POINT('Ctrl Pts',(-17.3019972576785,4.64007663330486,-0.330838851822665));
#53993=CARTESIAN_POINT('Ctrl Pts',(-17.103123725981,2.78674891347519,3.72475448883036));
#53994=CARTESIAN_POINT('Ctrl Pts',(-16.9042501942836,-1.6270494300105,4.35803575720979));
#53995=CARTESIAN_POINT('Ctrl Pts',(-16.7053766625861,-4.54591141642659,
0.987144823629757));
#53996=CARTESIAN_POINT('Ctrl Pts',(-16.5065031308886,-3.28798065943487,
-3.2907368007787));
#53997=CARTESIAN_POINT('Ctrl Pts',(-16.3076295991912,0.990953478566145,
-4.54508269585216));
#53998=CARTESIAN_POINT('Ctrl Pts',(-16.1087560674937,4.35939752576299,-1.623397277683));
#53999=CARTESIAN_POINT('Ctrl Pts',(-15.9098825357963,3.72241817525742,2.78986889249841));
#54000=CARTESIAN_POINT('Ctrl Pts',(-15.7110090040988,-0.334726637813821,
4.63979779589099));
#54001=CARTESIAN_POINT('Ctrl Pts',(-15.5121354724014,-4.0843239287767,2.22667095764937));
#54002=CARTESIAN_POINT('Ctrl Pts',(-15.313261940704,-4.08123600774924,-2.2323257284429));
#54003=CARTESIAN_POINT('Ctrl Pts',(-15.1143884090065,-0.32830006291181,
-4.64025695166864));
#54004=CARTESIAN_POINT('Ctrl Pts',(-14.9155148773091,3.72627865381841,-2.78471055998893));
#54005=CARTESIAN_POINT('Ctrl Pts',(-14.7166413456116,4.35714489235463,1.62943361197828));
#54006=CARTESIAN_POINT('Ctrl Pts',(-14.5177678139142,0.984657457389458,
4.54645083558862));
#54007=CARTESIAN_POINT('Ctrl Pts',(-14.3188942822167,-3.29253527119538,
3.28617969635737));
#54008=CARTESIAN_POINT('Ctrl Pts',(-14.1200207505192,-4.54453983213353,
-0.99344009530966));
#54009=CARTESIAN_POINT('Ctrl Pts',(-13.9211472188218,-1.62101186412838,
-4.36028508760289));
#54010=CARTESIAN_POINT('Ctrl Pts',(-13.7222736871243,2.79190513301711,-3.72089118855278));
#54011=CARTESIAN_POINT('Ctrl Pts',(-13.5234001554269,4.63961396140426,0.337265174543437));
#54012=CARTESIAN_POINT('Ctrl Pts',(-13.3245266237294,2.22443595566105,4.08554160277182));
#54013=CARTESIAN_POINT('Ctrl Pts',(-13.125653092032,-2.23455837351676,4.08001401764292));
#54014=CARTESIAN_POINT('Ctrl Pts',(-12.9267795603345,-4.64043588095,0.32576117572301));
#54015=CARTESIAN_POINT('Ctrl Pts',(-12.7279060286371,-2.78267137288683,
-3.72780170332774));
#54016=CARTESIAN_POINT('Ctrl Pts',(-12.5290324969396,1.63181730616761,-4.35625272316804));
#54017=CARTESIAN_POINT('Ctrl Pts',(-12.3301589652422,4.54698889374953,-0.982169796387303));
#54018=CARTESIAN_POINT('Ctrl Pts',(-12.1312854335447,3.28437774954679,3.29433275597639));
#54019=CARTESIAN_POINT('Ctrl Pts',(-11.9324119018472,-0.995926414662293,
4.54399560798588));
#54020=CARTESIAN_POINT('Ctrl Pts',(-11.7335383701498,-4.36117134417128,
1.61862596531638));
#54021=CARTESIAN_POINT('Ctrl Pts',(-11.5346648384523,-3.71936308798217,
-2.79394053776611));
#54022=CARTESIAN_POINT('Ctrl Pts',(-11.3357913067549,0.339803610311178,
-4.63942873802762));
#54023=CARTESIAN_POINT('Ctrl Pts',(-11.1369177750574,4.0867580537411,-2.22220028777761));
#54024=CARTESIAN_POINT('Ctrl Pts',(-10.93804424336,4.07879080616561,2.23679034966525));
#54025=CARTESIAN_POINT('Ctrl Pts',(-10.7391707116625,0.323222191015989,
4.64061342109551));
#54026=CARTESIAN_POINT('Ctrl Pts',(-10.5402971799651,-3.72932363690246,
2.78063135277903));
#54027=CARTESIAN_POINT('Ctrl Pts',(-10.3414236482676,-4.35535924991699,
-1.63420051186504));
#54028=CARTESIAN_POINT('Ctrl Pts',(-10.1425501165701,-0.979681841367978,
-4.54752559074833));
#54029=CARTESIAN_POINT('Ctrl Pts',(-9.94367658487271,3.29612925458378,-3.28257481954243));
#54030=CARTESIAN_POINT('Ctrl Pts',(-9.74480305317525,4.54345002357212,0.998412435879852));
#54031=CARTESIAN_POINT('Ctrl Pts',(-9.54592952147778,1.61623958196106,4.36205629520292));
#54032=CARTESIAN_POINT('Ctrl Pts',(-9.34705598978034,-2.79597510613618,
3.71783387400295));
#54033=CARTESIAN_POINT('Ctrl Pts',(-9.14818245808287,-4.63924212581646,
-0.342341944357115));
#54034=CARTESIAN_POINT('Ctrl Pts',(-8.94930892638543,-2.21996395466823,
-4.08797328132057));
#54035=CARTESIAN_POINT('Ctrl Pts',(-8.75043539468797,2.23902165622032,-4.07756637368338));
#54036=CARTESIAN_POINT('Ctrl Pts',(-8.55156186299052,4.64078957205195,-0.320683109550672));
#54037=CARTESIAN_POINT('Ctrl Pts',(-8.35268833129305,2.77859050027624,3.73084445408698));
#54038=CARTESIAN_POINT('Ctrl Pts',(-8.15381479959562,-1.63658322835689,
4.35446447286893));
#54039=CARTESIAN_POINT('Ctrl Pts',(-7.95494126789817,-4.54806092642439,
0.977193593076505));
#54040=CARTESIAN_POINT('Ctrl Pts',(-7.75606773620069,-3.28077090688404,
-3.29792476647959));
#54041=CARTESIAN_POINT('Ctrl Pts',(-7.55719420450327,1.00089815821756,-4.5429030790555));
#54042=CARTESIAN_POINT('Ctrl Pts',(-7.35832067280577,4.36293994043349,-1.61385271477731));
#54043=CARTESIAN_POINT('Ctrl Pts',(-7.15944714110836,3.71630354707174,2.79800883751849));
#54044=CARTESIAN_POINT('Ctrl Pts',(-6.96057360941086,-0.344880175919108,
4.63905412482613));
#54045=CARTESIAN_POINT('Ctrl Pts',(-6.76170007771343,-4.08918728515111,
2.21772695700357));
#54046=CARTESIAN_POINT('Ctrl Pts',(-6.56282654601595,-4.07634072055376,
-2.24125229251686));
#54047=CARTESIAN_POINT('Ctrl Pts',(-6.36395301431851,-0.318143932104064,
-4.64096433376144));
#54048=CARTESIAN_POINT('Ctrl Pts',(-6.16507948262108,3.73236415445752,-2.77654881599912));
#54049=CARTESIAN_POINT('Ctrl Pts',(-5.96620595092361,4.35356839223221,1.63896545494819));
#54050=CARTESIAN_POINT('Ctrl Pts',(-5.76733241922618,0.974705052370221,
4.54859490058293));
#54051=CARTESIAN_POINT('Ctrl Pts',(-5.5684588875287,-3.29971929133901,3.27896601217681));
#54052=CARTESIAN_POINT('Ctrl Pts',(-5.36958535583126,-4.54235477419835,
-1.0033835810547));
#54053=CARTESIAN_POINT('Ctrl Pts',(-5.17071182413379,-1.6114653652374,-4.36382227936571));
#54054=CARTESIAN_POINT('Ctrl Pts',(-4.97183829243634,2.80004173273539,-3.71477210808612));
#54055=CARTESIAN_POINT('Ctrl Pts',(-4.77296476073888,4.63886473241052,0.347418305066963));
#54056=CARTESIAN_POINT('Ctrl Pts',(-4.57409122904143,2.21548930055591,4.09040006330192));
#54057=CARTESIAN_POINT('Ctrl Pts',(-4.37521769734399,-2.24348226752039,
4.07511385010318));
#54058=CARTESIAN_POINT('Ctrl Pts',(-4.17634416564654,-4.64113768798076,
0.315604653849238));
#54059=CARTESIAN_POINT('Ctrl Pts',(-3.97747063394909,-2.77450633490745,
-3.73388272700877));
#54060=CARTESIAN_POINT('Ctrl Pts',(-3.77859710225162,1.64134725578213,-4.35267102819626));
#54061=CARTESIAN_POINT('Ctrl Pts',(-3.57972357055418,4.54912739060225,-0.972216182378774));
#54062=CARTESIAN_POINT('Ctrl Pts',(-3.3808500388567,3.27716036719384,3.30151275759948));
#54063=CARTESIAN_POINT('Ctrl Pts',(-3.18197650715927,-1.0058691402618,4.54180524327511));
#54064=CARTESIAN_POINT('Ctrl Pts',(-2.98310297546179,-4.36470248731841,
1.60907728082845));
#54065=CARTESIAN_POINT('Ctrl Pts',(-2.78422944376435,-3.71324111417162,
-2.80207331303322));
#54066=CARTESIAN_POINT('Ctrl Pts',(-2.58535591206692,0.349959270344922,
-4.6386748514615));
#54067=CARTESIAN_POINT('Ctrl Pts',(-2.38648238036945,4.09160606540612,-2.21324928125868));
#54068=CARTESIAN_POINT('Ctrl Pts',(-2.18760884867201,4.07389624223523,2.24570836167469));
#54069=CARTESIAN_POINT('Ctrl Pts',(-1.98873531697453,0.3130454880471,4.64131571257674));
#54070=CARTESIAN_POINT('Ctrl Pts',(-1.7898617852771,-3.73536280844222,2.77245158125543));
#54071=CARTESIAN_POINT('Ctrl Pts',(-1.59098825357963,-4.35184292986101,
-1.64370696036797));
#54072=CARTESIAN_POINT('Ctrl Pts',(-1.39211472188218,-0.969593771807376,
-4.54969931394381));
#54073=CARTESIAN_POINT('Ctrl Pts',(-1.19324119018471,3.30305362104828,-3.27527670617991));
#54074=CARTESIAN_POINT('Ctrl Pts',(-0.99436765848726,4.54172955224769,1.00820889559649));
#54075=CARTESIAN_POINT('Ctrl Pts',(-0.795494126789819,1.60579062235263,
4.36585649554455));
#54076=CARTESIAN_POINT('Ctrl Pts',(-0.596620595092368,-2.80240157693687,
3.71118654204902));
#54077=CARTESIAN_POINT('Ctrl Pts',(-0.397747063394913,-4.64175293605412,
-0.351489043021168));
#54078=CARTESIAN_POINT('Ctrl Pts',(-0.198873531697459,-2.20438994272706,
-4.09491721997484));
#54079=CARTESIAN_POINT('Ctrl Pts',(-0.0662911772324887,0.753200145251245,
-4.0766024725601));
#54080=CARTESIAN_POINT('Ctrl Pts',(0.,1.90056365518826,-3.44330463255539));
#54081=CARTESIAN_POINT('Ctrl Pts',(-109.840375352461,2.1465679056518,-3.00907133330628));
#54082=CARTESIAN_POINT('Ctrl Pts',(-109.774084175229,3.14923801912089,-2.29380099002595));
#54083=CARTESIAN_POINT('Ctrl Pts',(-109.641501820764,4.36578186624803,0.205448283167597));
#54084=CARTESIAN_POINT('Ctrl Pts',(-109.442628289066,2.1828302128901,3.79135494426175));
#54085=CARTESIAN_POINT('Ctrl Pts',(-109.243754757369,-2.00739020931939,
3.88220005863922));
#54086=CARTESIAN_POINT('Ctrl Pts',(-109.044881225672,-4.35233487181785,
0.411914045285927));
#54087=CARTESIAN_POINT('Ctrl Pts',(-108.846007693974,-2.69881131862259,
-3.43989927573611));
#54088=CARTESIAN_POINT('Ctrl Pts',(-108.647134162277,1.43463230878561,-4.12950976794978));
#54089=CARTESIAN_POINT('Ctrl Pts',(-108.448260630579,4.24980218800881,-1.02577369861691));
#54090=CARTESIAN_POINT('Ctrl Pts',(-108.249387098881,3.1603142753221,3.02089836059846));
#54091=CARTESIAN_POINT('Ctrl Pts',(-108.050513567184,-0.832913522680676,
4.29172289545985));
#54092=CARTESIAN_POINT('Ctrl Pts',(-107.851640035487,-4.0608392610929,1.61943067713845));
#54093=CARTESIAN_POINT('Ctrl Pts',(-107.652766503789,-3.55766782523455,
-2.54086506131637));
#54094=CARTESIAN_POINT('Ctrl Pts',(-107.453892972092,0.214301555961404,
-4.3665731279193));
#54095=CARTESIAN_POINT('Ctrl Pts',(-107.255019440394,3.78936734507133,-2.18028371201605));
#54096=CARTESIAN_POINT('Ctrl Pts',(-107.056145908697,3.88275616348223,2.00926485052088));
#54097=CARTESIAN_POINT('Ctrl Pts',(-106.857272376999,0.408659838058558,
4.3526914492715));
#54098=CARTESIAN_POINT('Ctrl Pts',(-106.658398845302,-3.44091355749422,
2.69685901065956));
#54099=CARTESIAN_POINT('Ctrl Pts',(-106.459525313605,-4.12896873804798,
-1.43685450907243));
#54100=CARTESIAN_POINT('Ctrl Pts',(-106.260651781907,-1.023318844092,-4.25038236929084));
#54101=CARTESIAN_POINT('Ctrl Pts',(-106.06177825021,3.02255844136648,-3.15865059785157));
#54102=CARTESIAN_POINT('Ctrl Pts',(-105.862904718512,4.29130285844483,0.835256049012763));
#54103=CARTESIAN_POINT('Ctrl Pts',(-105.664031186815,1.61718938013062,4.06172760623251));
#54104=CARTESIAN_POINT('Ctrl Pts',(-105.465157655117,-2.54280101173057,
3.55627556087148));
#54105=CARTESIAN_POINT('Ctrl Pts',(-105.26628412342,-4.36646061795366,-0.216689804582339));
#54106=CARTESIAN_POINT('Ctrl Pts',(-105.067410591722,-2.17820724021727,
-3.7905601153123));
#54107=CARTESIAN_POINT('Ctrl Pts',(-104.868537060025,2.01138742088055,-3.88165601822906));
#54108=CARTESIAN_POINT('Ctrl Pts',(-104.669663528328,4.35291519048993,-0.406278396632699));
#54109=CARTESIAN_POINT('Ctrl Pts',(-104.47078999663,2.69497554496221,3.44238864741278));
#54110=CARTESIAN_POINT('Ctrl Pts',(-104.271916464933,-1.43911316458767,
4.12818193541817));
#54111=CARTESIAN_POINT('Ctrl Pts',(-104.073042933235,-4.25094174373322,
1.02099318415578));
#54112=CARTESIAN_POINT('Ctrl Pts',(-103.874169401538,-3.15699632033617,
-3.02428620070342));
#54113=CARTESIAN_POINT('Ctrl Pts',(-103.67529586984,0.837603804328724,-4.29084521487517));
#54114=CARTESIAN_POINT('Ctrl Pts',(-103.476422338143,4.06261183376389,-1.61496683523748));
#54115=CARTESIAN_POINT('Ctrl Pts',(-103.277548806445,3.55488376867866,2.54474638852664));
#54116=CARTESIAN_POINT('Ctrl Pts',(-103.078675274748,-0.219078802209198,
4.36634140548465));
#54117=CARTESIAN_POINT('Ctrl Pts',(-102.879801743051,-3.79175131980121,
2.17613297377842));
#54118=CARTESIAN_POINT('Ctrl Pts',(-102.680928211353,-3.88055493925962,
-2.01351090242111));
#54119=CARTESIAN_POINT('Ctrl Pts',(-102.482054679656,-0.40389671268999,
-4.3531368271939));
#54120=CARTESIAN_POINT('Ctrl Pts',(-102.283181147958,3.44386264280962,-2.69309169696215));
#54121=CARTESIAN_POINT('Ctrl Pts',(-102.084307616261,4.12739393090686,1.44137161408848));
#54122=CARTESIAN_POINT('Ctrl Pts',(-101.885434084563,1.01866720062227,4.25149972658647));
#54123=CARTESIAN_POINT('Ctrl Pts',(-101.686560552866,-3.02601304519553,
3.15534116080873));
#54124=CARTESIAN_POINT('Ctrl Pts',(-101.487687021168,-4.29038629185808,
-0.839951342295326));
#54125=CARTESIAN_POINT('Ctrl Pts',(-101.288813489471,-1.61274380422899,
-4.06349482744949));
#54126=CARTESIAN_POINT('Ctrl Pts',(-101.089939957773,2.54669100212833,-3.55349092168056));
#54127=CARTESIAN_POINT('Ctrl Pts',(-100.891066426076,4.36622088667936,0.221467739213865));
#54128=CARTESIAN_POINT('Ctrl Pts',(-100.692192894378,2.17405805550784,3.79294138658497));
#54129=CARTESIAN_POINT('Ctrl Pts',(-100.493319362681,-2.01563378099804,
3.87945270001931));
#54130=CARTESIAN_POINT('Ctrl Pts',(-100.294445830983,-4.35335716087738,
0.401514907102131));
#54131=CARTESIAN_POINT('Ctrl Pts',(-100.095572299286,-2.69120704271377,
-3.44533560688004));
#54132=CARTESIAN_POINT('Ctrl Pts',(-99.8966987675885,1.44362963207685,-4.12660469104774));
#54133=CARTESIAN_POINT('Ctrl Pts',(-99.6978252358912,4.25205643675013,-1.01634091203658));
#54134=CARTESIAN_POINT('Ctrl Pts',(-99.4989517041936,3.15368505670657,3.02773898377871));
#54135=CARTESIAN_POINT('Ctrl Pts',(-99.3000781724963,-0.842298628814002,
4.28992608452472));
#54136=CARTESIAN_POINT('Ctrl Pts',(-99.1012046407987,-4.0643766047116,1.61052029042189));
#54137=CARTESIAN_POINT('Ctrl Pts',(-98.9023311091013,-3.55209701092721,
-2.54863485335771));
#54138=CARTESIAN_POINT('Ctrl Pts',(-98.7034575774039,0.223856609920464,
-4.36609906083021));
#54139=CARTESIAN_POINT('Ctrl Pts',(-98.5045840457063,3.79413031793455,-2.1719824864205));
#54140=CARTESIAN_POINT('Ctrl Pts',(-98.3057105140091,3.87834929944671,2.01775605618441));
#54141=CARTESIAN_POINT('Ctrl Pts',(-98.1068369823113,0.399132981319003,
4.35357619136394));
#54142=CARTESIAN_POINT('Ctrl Pts',(-97.9079634506143,-3.44680753957338,
2.68932158283975));
#54143=CARTESIAN_POINT('Ctrl Pts',(-97.7090899189163,-4.1258142158704,-1.44588721790784));
#54144=CARTESIAN_POINT('Ctrl Pts',(-97.5102163872193,-1.01401431920456,
-4.25261187404115));
#54145=CARTESIAN_POINT('Ctrl Pts',(-97.3113428555217,3.02946401599422,-3.15202800853414));
#54146=CARTESIAN_POINT('Ctrl Pts',(-97.1124693238242,4.28946459298215,0.844645663186656));
#54147=CARTESIAN_POINT('Ctrl Pts',(-96.9135957921268,1.60829629449811,4.06525716528381));
#54148=CARTESIAN_POINT('Ctrl Pts',(-96.7147222604292,-2.55057794164146,
3.55070203683716));
#54149=CARTESIAN_POINT('Ctrl Pts',(-96.5158487287319,-4.36597592796914,
-0.22624541361453));
#54150=CARTESIAN_POINT('Ctrl Pts',(-96.3169751970343,-2.16990626714019,
-3.79531811349369));
#54151=CARTESIAN_POINT('Ctrl Pts',(-96.1181016653371,2.01987772734617,-3.8772447378723));
#54152=CARTESIAN_POINT('Ctrl Pts',(-95.9192281336393,4.35379391858736,-0.396750936053586));
#54153=CARTESIAN_POINT('Ctrl Pts',(-95.7203546019423,2.68743531790485,3.44827844044897));
#54154=CARTESIAN_POINT('Ctrl Pts',(-95.5214810702444,-1.44814437090583,
4.1250225056115));
#54155=CARTESIAN_POINT('Ctrl Pts',(-95.3226075385472,-4.25316603829313,
1.01168742282264));
#54156=CARTESIAN_POINT('Ctrl Pts',(-95.1237340068497,-3.15037001678757,
-3.03118814132569));
#54157=CARTESIAN_POINT('Ctrl Pts',(-94.9248604751521,0.84699244471074,-4.28900181736853));
#54158=CARTESIAN_POINT('Ctrl Pts',(-94.7259869434549,4.06613650890247,-1.60607181712339));
#54159=CARTESIAN_POINT('Ctrl Pts',(-94.5271134117573,3.54930599982806,2.55252026639791));
#54160=CARTESIAN_POINT('Ctrl Pts',(-94.3282398800599,-0.22863414958098,
4.36585148813298));
#54161=CARTESIAN_POINT('Ctrl Pts',(-94.1293663483624,-3.79650477290681,
2.16782939828839));
#54162=CARTESIAN_POINT('Ctrl Pts',(-93.930492816665,-3.87613901562676,-2.02199879384818));
#54163=CARTESIAN_POINT('Ctrl Pts',(-93.7316192849675,-0.394368772018966,
-4.35401034248242));
#54164=CARTESIAN_POINT('Ctrl Pts',(-93.5327457532702,3.44974830906646,-2.68554824847382));
#54165=CARTESIAN_POINT('Ctrl Pts',(-93.3338722215725,4.12422956050804,1.45040109039508));
#54166=CARTESIAN_POINT('Ctrl Pts',(-93.1349986898752,1.00936022358743,4.2537189293402));
#54167=CARTESIAN_POINT('Ctrl Pts',(-92.9361251581777,-3.03291135925695,
3.14871108196318));
#54168=CARTESIAN_POINT('Ctrl Pts',(-92.7372516264802,-4.28853775782238,
-0.849338972683687));
#54169=CARTESIAN_POINT('Ctrl Pts',(-92.5383780947829,-1.60384685896368,
-4.06701463530438));
#54170=CARTESIAN_POINT('Ctrl Pts',(-92.3395045630853,2.55446182704561,-3.54790890031782));
#54171=CARTESIAN_POINT('Ctrl Pts',(-92.140631031388,4.365725741359,0.231022817104761));
#54172=CARTESIAN_POINT('Ctrl Pts',(-91.9417574996904,2.16575188048686,3.79769029581866));
#54173=CARTESIAN_POINT('Ctrl Pts',(-91.742883967993,-2.02411925505553,3.8750321330411));
#54174=CARTESIAN_POINT('Ctrl Pts',(-91.5440104362954,-4.35422546298436,
0.391986489928216));
#54175=CARTESIAN_POINT('Ctrl Pts',(-91.3451369045981,-2.68366037511149,
-3.45121714498581));
#54176=CARTESIAN_POINT('Ctrl Pts',(-91.1462633729005,1.45265737570005,-4.12343538079742));
#54177=CARTESIAN_POINT('Ctrl Pts',(-90.9473898412032,4.25427054701684,-1.00703272219558));
#54178=CARTESIAN_POINT('Ctrl Pts',(-90.7485163095057,3.14705120455755,3.03463366927219));
#54179=CARTESIAN_POINT('Ctrl Pts',(-90.5496427778082,-0.851685246403096,
4.28807241448263));
#54180=CARTESIAN_POINT('Ctrl Pts',(-90.3507692461108,-4.06789154422664,
1.60162142068499));
#54181=CARTESIAN_POINT('Ctrl Pts',(-90.1518957144133,-3.54651073872464,
-2.55640262300335));
#54182=CARTESIAN_POINT('Ctrl Pts',(-89.9530221827159,0.233411415470766,
-4.36559868768483));
#54183=CARTESIAN_POINT('Ctrl Pts',(-89.7541486510185,3.79887468187438,-2.16367371435747));
#54184=CARTESIAN_POINT('Ctrl Pts',(-89.5552751193209,3.87392409044664,2.0262391103334));
#54185=CARTESIAN_POINT('Ctrl Pts',(-89.3564015876237,0.389604090494498,
4.35443928002878));
#54186=CARTESIAN_POINT('Ctrl Pts',(-89.1575280559259,-3.4526849477674,2.681771698383));
#54187=CARTESIAN_POINT('Ctrl Pts',(-88.9586545242288,-4.12263996671732,
-1.45491322614534));
#54188=CARTESIAN_POINT('Ctrl Pts',(-88.759780992531,-1.00470491934382,-4.25482089115792));
#54189=CARTESIAN_POINT('Ctrl Pts',(-88.5609074608338,3.03635507085581,-3.14539038506761));
#54190=CARTESIAN_POINT('Ctrl Pts',(-88.3620339291362,4.28760578748858,0.854031265166599));
#54191=CARTESIAN_POINT('Ctrl Pts',(-88.1631603974388,1.59939550295351,4.06876723540677));
#54192=CARTESIAN_POINT('Ctrl Pts',(-87.9642868657414,-2.55834265369014,
3.54511151546708));
#54193=CARTESIAN_POINT('Ctrl Pts',(-87.7654133340439,-4.36547032714852,
-0.23579994396399));
#54194=CARTESIAN_POINT('Ctrl Pts',(-87.5665398023464,-2.16159490052237,
-3.80005793071938));
#54195=CARTESIAN_POINT('Ctrl Pts',(-87.3676662706491,2.02835835904724,-3.87281488817511));
#54196=CARTESIAN_POINT('Ctrl Pts',(-87.1687927389515,4.35465179355167,-0.387221574430996));
#54197=CARTESIAN_POINT('Ctrl Pts',(-86.9699192072541,2.67988221885378,3.45415171697175));
#54198=CARTESIAN_POINT('Ctrl Pts',(-86.7710456755566,-1.45716864105561,
4.12184331850591));
#54199=CARTESIAN_POINT('Ctrl Pts',(-86.5721721438592,-4.25536996159869,
1.00237681572903));
#54200=CARTESIAN_POINT('Ctrl Pts',(-86.3732986121618,-3.14372862399053,
-3.03807556349247));
#54201=CARTESIAN_POINT('Ctrl Pts',(-86.1744250804642,0.856377028271844,
-4.28713787697993));
#54202=CARTESIAN_POINT('Ctrl Pts',(-85.9755515487668,4.06964170858263,-1.59716910643562));
#54203=CARTESIAN_POINT('Ctrl Pts',(-85.7766780170694,3.54371123096399,2.56028191852522));
#54204=CARTESIAN_POINT('Ctrl Pts',(-85.577804485372,-0.238188401869361,
4.36534065978847));
#54205=CARTESIAN_POINT('Ctrl Pts',(-85.3789309536744,-3.80124004199946,
2.1595154396039));
#54206=CARTESIAN_POINT('Ctrl Pts',(-85.180057421977,-3.87170452655856,-2.03047700056258));
#54207=CARTESIAN_POINT('Ctrl Pts',(-84.9811838902796,-0.384838942450937,
-4.35486300348942));
#54208=CARTESIAN_POINT('Ctrl Pts',(-84.782310358582,3.45561745215982,-2.67799193708943));
#54209=CARTESIAN_POINT('Ctrl Pts',(-84.5834368268847,4.12104543640164,1.45942361975566));
#54210=CARTESIAN_POINT('Ctrl Pts',(-84.3845632951872,1.00004841204814,4.25591775817481));
#54211=CARTESIAN_POINT('Ctrl Pts',(-84.1856897634897,-3.0397951466672,3.14206592182376));
#54212=CARTESIAN_POINT('Ctrl Pts',(-83.9868162317922,-4.28666868309671,
-0.858722535016742));
#54213=CARTESIAN_POINT('Ctrl Pts',(-83.7879427000949,-1.59494223179772,
-4.07051496349243));
#54214=CARTESIAN_POINT('Ctrl Pts',(-83.5890691683973,2.56222041692812,-3.54230988563454));
#54215=CARTESIAN_POINT('Ctrl Pts',(-83.3901956367,4.36520968564351,0.240576788472024));
#54216=CARTESIAN_POINT('Ctrl Pts',(-83.1913221050024,2.15743533222441,3.8024210153608));
#54217=CARTESIAN_POINT('Ctrl Pts',(-82.9924485733051,-2.03259503424531,
3.87059300592932));
#54218=CARTESIAN_POINT('Ctrl Pts',(-82.7935750416076,-4.3550729097788,0.382456195267517));
#54219=CARTESIAN_POINT('Ctrl Pts',(-82.5947015099101,-2.67610085365577,
-3.45708215289286));
#54220=CARTESIAN_POINT('Ctrl Pts',(-82.3958279782126,1.46167816157059,-4.12024632064336));
#54221=CARTESIAN_POINT('Ctrl Pts',(-82.1969544465152,4.25646428072227,-0.997719708998039));
#54222=CARTESIAN_POINT('Ctrl Pts',(-81.9980809148177,3.14040227906498,3.04151381986522));
#54223=CARTESIAN_POINT('Ctrl Pts',(-81.7992073831203,-0.861067784699082,
4.28619820597941));
#54224=CARTESIAN_POINT('Ctrl Pts',(-81.6003338514229,-4.07138699987473,
1.59271487970651));
#54225=CARTESIAN_POINT('Ctrl Pts',(-81.4014603197254,-3.54090747989828,
-2.56415814831845));
#54226=CARTESIAN_POINT('Ctrl Pts',(-81.2025867880279,0.242965103056872,
-4.36507740475289));
#54227=CARTESIAN_POINT('Ctrl Pts',(-81.0037132563305,3.80360085044983,-2.15535457900667));
#54228=CARTESIAN_POINT('Ctrl Pts',(-80.804839724633,3.86948032662017,2.03471245946132));
#54229=CARTESIAN_POINT('Ctrl Pts',(-80.6059661929357,0.380073333594103,
4.35528151235694));
#54230=CARTESIAN_POINT('Ctrl Pts',(-80.407092661238,-3.45854581873234,2.674208969119));
#54231=CARTESIAN_POINT('Ctrl Pts',(-80.2082191295408,-4.11944597147032,
-1.46393226582538));
#54232=CARTESIAN_POINT('Ctrl Pts',(-80.0093455978432,-0.995390707275934,
-4.25700952907747));
#54233=CARTESIAN_POINT('Ctrl Pts',(-79.8104720661457,3.04323158257202,-3.13873769621227));
#54234=CARTESIAN_POINT('Ctrl Pts',(-79.6115985344483,4.28572644576884,0.863412776616762));
#54235=CARTESIAN_POINT('Ctrl Pts',(-79.4127250027508,1.59048705082877,4.07225781746852));
#54236=CARTESIAN_POINT('Ctrl Pts',(-79.2138514710534,-2.56609511211621,
3.53950401417501));
#54237=CARTESIAN_POINT('Ctrl Pts',(-79.014977939356,-4.36494381715614,-0.245353344909039));
#54238=CARTESIAN_POINT('Ctrl Pts',(-78.8161044076585,-2.1532731805736,-3.80477954691332));
#54239=CARTESIAN_POINT('Ctrl Pts',(-78.617230875961,2.03682927557666,-3.86836648896422));
#54240=CARTESIAN_POINT('Ctrl Pts',(-78.4183573442637,4.35548881116147,-0.377690358144029));
#54241=CARTESIAN_POINT('Ctrl Pts',(-78.2194838125661,2.67231628404541,3.46000844924017));
#54242=CARTESIAN_POINT('Ctrl Pts',(-78.0206102808687,-1.46618593184531,
4.11864438912206));
#54243=CARTESIAN_POINT('Ctrl Pts',(-77.8217367491712,-4.25755350307716,
0.99306140757905));
#54244=CARTESIAN_POINT('Ctrl Pts',(-77.6228632174738,-3.13707217376396,
-3.04494843427329));
#54245=CARTESIAN_POINT('Ctrl Pts',(-77.4239896857763,0.865757510067786,
-4.2852534026063));
#54246=CARTESIAN_POINT('Ctrl Pts',(-77.2251161540789,4.07312741601313,-1.58825874583137));
#54247=CARTESIAN_POINT('Ctrl Pts',(-77.0262426223814,3.5380994888848,2.56803130774155));
#54248=CARTESIAN_POINT('Ctrl Pts',(-76.8273690906839,-0.247741513313501,
4.36480892289326));
#54249=CARTESIAN_POINT('Ctrl Pts',(-76.6284955589866,-3.80595710439848,
2.15119113754828));
#54250=CARTESIAN_POINT('Ctrl Pts',(-76.429622027289,-3.86725149329488,-2.03894548195781));
#54251=CARTESIAN_POINT('Ctrl Pts',(-76.2307484955916,-0.375307269630516,
-4.35569480613026));
#54252=CARTESIAN_POINT('Ctrl Pts',(-76.0318749638941,3.46147004397849,-2.67042279900155));
#54253=CARTESIAN_POINT('Ctrl Pts',(-75.8330014321968,4.11784157383855,1.46843915895566));
#54254=CARTESIAN_POINT('Ctrl Pts',(-75.6341279004991,0.990731810604663,
4.25809620255854));
#54255=CARTESIAN_POINT('Ctrl Pts',(-75.4352543688019,-3.04666437445524,
3.13540571221858));
#54256=CARTESIAN_POINT('Ctrl Pts',(-75.2363808371042,-4.28477907663331,
-0.868101984350383));
#54257=CARTESIAN_POINT('Ctrl Pts',(-75.037507305407,-1.58602996538132,-4.07399579524822));
#54258=CARTESIAN_POINT('Ctrl Pts',(-74.8386337737093,2.56996673461481,-3.53669390444816));
#54259=CARTESIAN_POINT('Ctrl Pts',(-74.6397602420121,4.36467272200467,0.250129607555377));
#54260=CARTESIAN_POINT('Ctrl Pts',(-74.4408867103144,2.14910845055393,3.80713352255281));
#54261=CARTESIAN_POINT('Ctrl Pts',(-74.2420131786171,-2.04106107797122,
3.86613533994589));
#54262=CARTESIAN_POINT('Ctrl Pts',(-74.0431396469196,-4.35589949720169,
0.372924068767042));
#54263=CARTESIAN_POINT('Ctrl Pts',(-73.8442661152221,-2.66852851455428,
-3.46293060250971));
#54264=CARTESIAN_POINT('Ctrl Pts',(-73.6453925835248,1.47069194648194,-4.11703752586014));
#54265=CARTESIAN_POINT('Ctrl Pts',(-73.4465190518272,4.25863762735916,-0.988401917050126));
#54266=CARTESIAN_POINT('Ctrl Pts',(-73.2476455201298,3.13373831207497,3.04837940260415));
#54267=CARTESIAN_POINT('Ctrl Pts',(-73.0487719884323,-0.870446198762599,
4.28430346799187));
#54268=CARTESIAN_POINT('Ctrl Pts',(-72.849898456735,-4.07486295491378,1.58380071014596));
#54269=CARTESIAN_POINT('Ctrl Pts',(-72.6510249250373,-3.53528726128592,
-2.57190139215663));
#54270=CARTESIAN_POINT('Ctrl Pts',(-72.4521513933401,0.252517626919826,
-4.36453521453115));
#54271=CARTESIAN_POINT('Ctrl Pts',(-72.2532778616424,3.80830880102412,-2.147025120214));
#54272=CARTESIAN_POINT('Ctrl Pts',(-72.0544043299452,3.86501802925143,2.04317606298353));
#54273=CARTESIAN_POINT('Ctrl Pts',(-71.8555307982476,0.370540756267099,
4.35610288431443));
#54274=CARTESIAN_POINT('Ctrl Pts',(-71.6566572665502,-3.46439012439663,
2.66663343127074));
#54275=CARTESIAN_POINT('Ctrl Pts',(-71.4577837348527,-4.11623224542755,
-1.47294429374982));
#54276=CARTESIAN_POINT('Ctrl Pts',(-71.2589102031553,-0.986071727612851,
-4.25917777731692));
#54277=CARTESIAN_POINT('Ctrl Pts',(-71.0600366714578,3.05009351820653,-3.13206997383232));
#54278=CARTESIAN_POINT('Ctrl Pts',(-70.8611631397603,4.28382657682442,0.872790152602706));
#54279=CARTESIAN_POINT('Ctrl Pts',(-70.6622896080629,1.58157098079249,4.07572889475033));
#54280=CARTESIAN_POINT('Ctrl Pts',(-70.4634160763654,-2.57383527978793,
3.53387955981901));
#54281=CARTESIAN_POINT('Ctrl Pts',(-70.264542544668,-4.36439640051381,-0.254905570691984));
#54282=CARTESIAN_POINT('Ctrl Pts',(-70.0656690129705,-2.14494114715219,
-3.80948293946055));
#54283=CARTESIAN_POINT('Ctrl Pts',(-69.8667954812732,2.04529043636163,-3.86389956154597));
#54284=CARTESIAN_POINT('Ctrl Pts',(-69.6679219495755,4.35630496740768,-0.368157332844027));
#54285=CARTESIAN_POINT('Ctrl Pts',(-69.4690484178782,2.66473754971807,3.4658486092024));
#54286=CARTESIAN_POINT('Ctrl Pts',(-69.2701748861807,-1.47519620008504,
4.11542573278177));
#54287=CARTESIAN_POINT('Ctrl Pts',(-69.0713013544833,-4.25971665227008,
0.983741242990482));
#54288=CARTESIAN_POINT('Ctrl Pts',(-68.8724278227858,-3.13040069799007,
-3.05180672074932));
#54289=CARTESIAN_POINT('Ctrl Pts',(-68.6735542910884,0.875133845169071,
-4.28334840327369));
#54290=CARTESIAN_POINT('Ctrl Pts',(-68.4746807593909,4.07659361449859,-1.5793407779884));
#54291=CARTESIAN_POINT('Ctrl Pts',(-68.2758072276934,3.53247080046894,2.57576839692974));
#54292=CARTESIAN_POINT('Ctrl Pts',(-68.076933695996,-0.257293438156953,
4.3642562799942));
#54293=CARTESIAN_POINT('Ctrl Pts',(-67.8780601642985,-3.81065593751065,
2.14285653199235));
#54294=CARTESIAN_POINT('Ctrl Pts',(-67.6791866326011,-3.86277993716433,
-2.0474041974726));
#54295=CARTESIAN_POINT('Ctrl Pts',(-67.4803131009036,-0.365773799211309,
-4.35650574642089));
#54296=CARTESIAN_POINT('Ctrl Pts',(-67.2814395692062,3.46730605649033,-2.6628408704639));
#54297=CARTESIAN_POINT('Ctrl Pts',(-67.0825660375088,4.11461798816427,1.47744766481337));
#54298=CARTESIAN_POINT('Ctrl Pts',(-66.8836925058112,0.981410463880688,
4.2602542520574));
#54299=CARTESIAN_POINT('Ctrl Pts',(-66.6848189741139,-3.0535190097197,3.12873048504791));
#54300=CARTESIAN_POINT('Ctrl Pts',(-66.4859454424164,-4.28286894748279,
-0.877477275760104));
#54301=CARTESIAN_POINT('Ctrl Pts',(-66.2870719107189,-1.57711010240136,
-4.07745711389967));
#54302=CARTESIAN_POINT('Ctrl Pts',(-66.0881983790215,2.57770074300329,-3.53106098365743));
#54303=CARTESIAN_POINT('Ctrl Pts',(-65.889324847324,4.36411485301436,0.259681228599884));
#54304=CARTESIAN_POINT('Ctrl Pts',(-65.6904513156265,2.1407712753585,3.81182779482331));
#54305=CARTESIAN_POINT('Ctrl Pts',(-65.4915777839291,-2.04951734568369,
3.86165915644162));
#54306=CARTESIAN_POINT('Ctrl Pts',(-65.2927042522317,-4.35670522129393,
0.363390156082553));
#54307=CARTESIAN_POINT('Ctrl Pts',(-65.0938307205342,-2.66094339407605,
-3.46876246582416));
#54308=CARTESIAN_POINT('Ctrl Pts',(-64.8949571888368,1.47969868726097,-4.11380901181689));
#54309=CARTESIAN_POINT('Ctrl Pts',(-64.6960836571392,4.26079057651791,-0.97907939098104));
#54310=CARTESIAN_POINT('Ctrl Pts',(-64.4972101254419,3.12705933550577,3.05523038460505));
#54311=CARTESIAN_POINT('Ctrl Pts',(-64.2983365937443,-0.87982044367422,
4.28238820959525));
#54312=CARTESIAN_POINT('Ctrl Pts',(-64.0994630620469,-4.07831939269513,
1.57487895469916));
#54313=CARTESIAN_POINT('Ctrl Pts',(-63.9005895303495,-3.52965010980649,
-2.57963231743028));
#54314=CARTESIAN_POINT('Ctrl Pts',(-63.7017159986519,0.26206894130613,-4.36397211961652));
#54315=CARTESIAN_POINT('Ctrl Pts',(-63.5028424669547,3.81299851104771,-2.13868537787484));
#54316=CARTESIAN_POINT('Ctrl Pts',(-63.303968935257,3.86053721971338,2.05162988036224));
#54317=CARTESIAN_POINT('Ctrl Pts',(-63.1050954035597,0.361006404171295,
4.35690339196714));
#54318=CARTESIAN_POINT('Ctrl Pts',(-62.9062218718622,-3.47021783676795,
2.65904512112248));
#54319=CARTESIAN_POINT('Ctrl Pts',(-62.7073483401648,-4.11299880398172,
-1.48194926675396));
#54320=CARTESIAN_POINT('Ctrl Pts',(-62.5084748084672,-0.976748024989449,
-4.26132562549107));
#54321=CARTESIAN_POINT('Ctrl Pts',(-62.3096012767699,3.05694084489302,-3.12538724986396));
#54322=CARTESIAN_POINT('Ctrl Pts',(-62.1107277450723,4.28190618975503,0.882163348210001));
#54323=CARTESIAN_POINT('Ctrl Pts',(-61.911854213375,1.57264733554965,4.07918045062685));
#54324=CARTESIAN_POINT('Ctrl Pts',(-61.7129806816774,-2.58156311963242,
3.52823817933844));
#54325=CARTESIAN_POINT('Ctrl Pts',(-61.5141071499801,-4.36382807984344,
-0.264456575560786));
#54326=CARTESIAN_POINT('Ctrl Pts',(-61.3152336182825,-2.13659884016589,
-3.8141680858333));
#54327=CARTESIAN_POINT('Ctrl Pts',(-61.1163600865851,2.05374180087587,-3.85941412731554));
#54328=CARTESIAN_POINT('Ctrl Pts',(-60.9174865548877,4.35710025838121,-0.358622544191085));
#54329=CARTESIAN_POINT('Ctrl Pts',(-60.7186130231903,2.65714605217142,3.47167216888599));
#54330=CARTESIAN_POINT('Ctrl Pts',(-60.5197394914927,-1.48419940261849,
4.11218736490133));
#54331=CARTESIAN_POINT('Ctrl Pts',(-60.3208659597953,-4.26185939881663,
0.974416366603987));
#54332=CARTESIAN_POINT('Ctrl Pts',(-60.1219924280979,-3.1237142286232,-3.05865039007152));
#54333=CARTESIAN_POINT('Ctrl Pts',(-59.9231188964004,0.884505988666006,
-4.28142288810644));
#54334=CARTESIAN_POINT('Ctrl Pts',(-59.724245364703,4.08004028743699,-1.57041524562096));
#54335=CARTESIAN_POINT('Ctrl Pts',(-59.5253718330054,3.52682519267604,2.58349314903161));
#54336=CARTESIAN_POINT('Ctrl Pts',(-59.3264983013081,-0.266844130649094,
4.3636827337383));
#54337=CARTESIAN_POINT('Ctrl Pts',(-59.1276247696105,-3.81533651883011,
2.13451166285616));
#54338=CARTESIAN_POINT('Ctrl Pts',(-58.9287512379131,-3.85828987958418,
-2.05585310659239));
#54339=CARTESIAN_POINT('Ctrl Pts',(-58.7298777062157,-0.356238576855684,
-4.35729582047709));
#54340=CARTESIAN_POINT('Ctrl Pts',(-58.5310041745182,3.47312546174274,-2.65524618779161));
#54341=CARTESIAN_POINT('Ctrl Pts',(-58.3321306428208,4.11137469481877,1.48644909418102));
#54342=CARTESIAN_POINT('Ctrl Pts',(-58.1332571111233,0.972084416522393,
4.26239189633496));
#54343=CARTESIAN_POINT('Ctrl Pts',(-57.9343835794259,-3.06035901962902,
3.12204027228397));
#54344=CARTESIAN_POINT('Ctrl Pts',(-57.7355100477284,-4.28093830479405,
-0.886848364341211));
#54345=CARTESIAN_POINT('Ctrl Pts',(-57.5366365160309,-1.5681826855811,-4.08089890286826));
#54346=CARTESIAN_POINT('Ctrl Pts',(-57.3377629843335,2.58542240505028,-3.52541115024215));
#54347=CARTESIAN_POINT('Ctrl Pts',(-57.138889452636,4.3635360813445,0.269231605856388));
#54348=CARTESIAN_POINT('Ctrl Pts',(-56.9400159209386,2.1324238465706,3.81650380968817));
#54349=CARTESIAN_POINT('Ctrl Pts',(-56.7411423892411,-2.05796379687972,
3.85716447685603));
#54350=CARTESIAN_POINT('Ctrl Pts',(-56.5422688575437,-4.35749007819642,
0.353854502878531));
#54351=CARTESIAN_POINT('Ctrl Pts',(-56.3433953258462,-2.65334552855137,
-3.47457771490351));
#54352=CARTESIAN_POINT('Ctrl Pts',(-56.1445217941488,1.48869834076828,-4.11056079397708));
#54353=CARTESIAN_POINT('Ctrl Pts',(-55.9456482624513,4.26292311788657,-0.969752175442759));
#54354=CARTESIAN_POINT('Ctrl Pts',(-55.7467747307538,3.12036538134755,3.0620667330539));
#54355=CARTESIAN_POINT('Ctrl Pts',(-55.5479011990564,-0.889190474534251,
4.28045243996301));
#54356=CARTESIAN_POINT('Ctrl Pts',(-55.349027667359,-4.08175629666357,1.56594965609849));
#54357=CARTESIAN_POINT('Ctrl Pts',(-55.1501541356615,-3.52399605246015,
-2.58735088711071));
#54358=CARTESIAN_POINT('Ctrl Pts',(-54.9512806039641,0.271619000467934,
-4.36338812270604));
#54359=CARTESIAN_POINT('Ctrl Pts',(-54.7524070722666,3.8176699580583,-2.13033539193406));
#54360=CARTESIAN_POINT('Ctrl Pts',(-54.5535335405692,3.85603791946774,2.06007387110622));
#54361=CARTESIAN_POINT('Ctrl Pts',(-54.3546600088717,0.351470322973323,
4.35768303148091));
#54362=CARTESIAN_POINT('Ctrl Pts',(-54.1557864771742,-3.47602892793337,
2.65144407501989));
#54363=CARTESIAN_POINT('Ctrl Pts',(-53.9569129454769,-4.10974566262001,
-1.49094714170681));
#54364=CARTESIAN_POINT('Ctrl Pts',(-53.7580394137793,-0.967419644063333,
-4.26345306331242));
#54365=CARTESIAN_POINT('Ctrl Pts',(-53.5591658820819,3.06377352983496,-3.11868955631533));
#54366=CARTESIAN_POINT('Ctrl Pts',(-53.3602923503844,4.2799652937587,0.891532318543936));
#54367=CARTESIAN_POINT('Ctrl Pts',(-53.161418818687,1.56371615784177,4.08261246856616));
#54368=CARTESIAN_POINT('Ctrl Pts',(-52.9625452869895,-2.58927859463567,
3.52257989975376));
#54369=CARTESIAN_POINT('Ctrl Pts',(-52.7636717552921,-4.36323885786721,
-0.274006313769111));
#54370=CARTESIAN_POINT('Ctrl Pts',(-52.5647982235946,-2.12824629957168,
-3.81883496359127));
#54371=CARTESIAN_POINT('Ctrl Pts',(-52.3659246918972,2.06218332864007,-3.85491020775668));
#54372=CARTESIAN_POINT('Ctrl Pts',(-52.1670511601997,4.35787468027285,-0.349086037853842));
#54373=CARTESIAN_POINT('Ctrl Pts',(-51.9681776285022,2.64954182776637,3.47747910039789));
#54374=CARTESIAN_POINT('Ctrl Pts',(-51.7693040968048,-1.49319549632342,
4.10892930099158));
#54375=CARTESIAN_POINT('Ctrl Pts',(-51.5704305651073,-4.26398173245389,
0.965086823082352));
#54376=CARTESIAN_POINT('Ctrl Pts',(-51.3715570334099,-3.117012797689,-3.06547940946115));
#54377=CARTESIAN_POINT('Ctrl Pts',(-51.1726835017125,0.893873895669284,
-4.27947686632704));
#54378=CARTESIAN_POINT('Ctrl Pts',(-50.9738099700149,4.08346741831995,-1.56148219147932));
#54379=CARTESIAN_POINT('Ctrl Pts',(-50.7749364383176,3.52116269254666,2.59120552704822));
#54380=CARTESIAN_POINT('Ctrl Pts',(-50.5760629066201,-0.276393545045298,
4.36308828687261));
#54381=CARTESIAN_POINT('Ctrl Pts',(-50.3771893749227,-3.81999882593834,
2.12615657010893));
#54382=CARTESIAN_POINT('Ctrl Pts',(-50.1783158432251,-3.85378134206042,
-2.06429216884982));
#54383=CARTESIAN_POINT('Ctrl Pts',(-49.9794423115277,-0.346701648233845,
-4.35806502451485));
#54384=CARTESIAN_POINT('Ctrl Pts',(-49.7805687798303,3.47892823186297,-2.64763878736025));
#54385=CARTESIAN_POINT('Ctrl Pts',(-49.5816952481328,4.10811170933616,1.49544340394506));
#54386=CARTESIAN_POINT('Ctrl Pts',(-49.3828217164354,0.962753713198245,
4.26450912515266));
#54387=CARTESIAN_POINT('Ctrl Pts',(-49.1839481847379,-3.06718437142193,
3.11533510597052));
#54388=CARTESIAN_POINT('Ctrl Pts',(-48.9850746530405,-4.27898715781424,
-0.896215205209373));
#54389=CARTESIAN_POINT('Ctrl Pts',(-48.786201121343,-1.55924775767987,-4.08432114566889));
#54390=CARTESIAN_POINT('Ctrl Pts',(-48.5873275896455,2.59313168377142,-3.51974443126322));
#54391=CARTESIAN_POINT('Ctrl Pts',(-48.3884540579481,4.36293640976736,0.278780693581792));
#54392=CARTESIAN_POINT('Ctrl Pts',(-48.1895805262506,2.12406620417138,3.82116154475111));
#54393=CARTESIAN_POINT('Ctrl Pts',(-47.9907069945532,-2.06640039110415,
3.8526513227169));
#54394=CARTESIAN_POINT('Ctrl Pts',(-47.7918334628557,-4.35825406414994,
0.344317154827103));
#54395=CARTESIAN_POINT('Ctrl Pts',(-47.5929599311583,-2.64573495437125,
-3.48037632189472));
#54396=CARTESIAN_POINT('Ctrl Pts',(-47.3940863994607,1.49769086389862,-4.10729288789854));
#54397=CARTESIAN_POINT('Ctrl Pts',(-47.1952128677634,4.26503524125097,-0.960420315109474));
#54398=CARTESIAN_POINT('Ctrl Pts',(-46.9963393360659,3.11365648166209,3.06888841520693));
#54399=CARTESIAN_POINT('Ctrl Pts',(-46.7974658043685,-0.898556246463373,
4.2784961683668));
#54400=CARTESIAN_POINT('Ctrl Pts',(-46.5985922726709,-4.08517365035739,
1.5570128571124));
#54401=CARTESIAN_POINT('Ctrl Pts',(-46.3997187409736,-3.51832511632802,
-2.59505706422866));
#54402=CARTESIAN_POINT('Ctrl Pts',(-46.2008452092761,0.281167758664008,
-4.36278322659693));
#54403=CARTESIAN_POINT('Ctrl Pts',(-46.0019716775787,3.8223231196815,-2.12197520238479));
#54404=CARTESIAN_POINT('Ctrl Pts',(-45.8030981458812,3.8515201500644,2.06850799477198));
#54405=CARTESIAN_POINT('Ctrl Pts',(-45.6042246141837,0.341932558347505,
4.35844179912147));
#54406=CARTESIAN_POINT('Ctrl Pts',(-45.4053510824862,-3.48182337005976,
2.64383032936931));
#54407=CARTESIAN_POINT('Ctrl Pts',(-45.2064775507889,-4.10647283692384,
-1.49993787551162));
#54408=CARTESIAN_POINT('Ctrl Pts',(-45.0076040190913,-0.95808662951426,
-4.26556008059126));
#54409=CARTESIAN_POINT('Ctrl Pts',(-44.808730487394,3.07059154030602,-3.11197692526612));
#54410=CARTESIAN_POINT('Ctrl Pts',(-44.6098569556964,4.27800389813174,0.900897018730402));
#54411=CARTESIAN_POINT('Ctrl Pts',(-44.410983423999,1.55477749044593,4.08602493213029));
#54412=CARTESIAN_POINT('Ctrl Pts',(-44.2121098923016,-2.59698166784357,
3.51690474816593));
#54413=CARTESIAN_POINT('Ctrl Pts',(-44.0132363606041,-4.36262873740718,
-0.283554739577348));
#54414=CARTESIAN_POINT('Ctrl Pts',(-43.8143628289067,-2.11988356537511,
-3.82348355038179));
#54415=CARTESIAN_POINT('Ctrl Pts',(-43.6154892972092,2.07061497922229,-3.85038782444153));
#54416=CARTESIAN_POINT('Ctrl Pts',(-43.4166157655118,4.35862822937335,-0.339547859508846));
#54417=CARTESIAN_POINT('Ctrl Pts',(-43.2177422338143,2.64192491292454,3.48326937592491));
#54418=CARTESIAN_POINT('Ctrl Pts',(-43.0188687021169,-1.50218443811134,
4.10565155665745));
#54419=CARTESIAN_POINT('Ctrl Pts',(-42.8199951704193,-4.26608364301641,
0.955752657111389));
#54420=CARTESIAN_POINT('Ctrl Pts',(-42.621121638722,-3.11029643728546,-3.07229374620934));
#54421=CARTESIAN_POINT('Ctrl Pts',(-42.4222481070244,0.903237521309745,
-4.27751034725644));
#54422=CARTESIAN_POINT('Ctrl Pts',(-42.2233745753271,4.08687499073273,-1.55254165834964));
#54423=CARTESIAN_POINT('Ctrl Pts',(-42.0245010436295,3.51548332720214,2.59890549404002));
#54424=CARTESIAN_POINT('Ctrl Pts',(-41.8256275119321,-0.285941635607189,
4.36247294224429));
#54425=CARTESIAN_POINT('Ctrl Pts',(-41.6267539802346,-3.82464283650449,
2.11779129376864));
#54426=CARTESIAN_POINT('Ctrl Pts',(-41.4278804485372,-3.84925434618739,
-2.07272134382439));
#54427=CARTESIAN_POINT('Ctrl Pts',(-41.2290069168397,-0.337163059024936,
-4.35881335484976));
#54428=CARTESIAN_POINT('Ctrl Pts',(-41.0301333851424,3.48471433905729,-2.64001870560726));
#54429=CARTESIAN_POINT('Ctrl Pts',(-40.8312598534448,4.10482904734529,1.50443055102521));
#54430=CARTESIAN_POINT('Ctrl Pts',(-40.6323863217474,0.95341839859954,4.26660592836971));
#54431=CARTESIAN_POINT('Ctrl Pts',(-40.4335127900499,-3.07399503240732,
3.10861501822319));
#54432=CARTESIAN_POINT('Ctrl Pts',(-40.2346392583525,-4.27701551588864,
-0.905577753500761));
#54433=CARTESIAN_POINT('Ctrl Pts',(-40.035765726655,-1.55030536149281,-4.08772382591024));
#54434=CARTESIAN_POINT('Ctrl Pts',(-39.8368921949575,2.600828542242,-3.51406085386219));
#54435=CARTESIAN_POINT('Ctrl Pts',(-39.6380186632601,4.36231584115501,0.288328446039067));
#54436=CARTESIAN_POINT('Ctrl Pts',(-39.4391451315626,2.11569838819149,3.82580097770278));
#54437=CARTESIAN_POINT('Ctrl Pts',(-39.2402715998652,-2.07482708794791,
3.84811971564105));
#54438=CARTESIAN_POINT('Ctrl Pts',(-39.0413980681677,-4.3589971754952,0.334778157609627));
#54439=CARTESIAN_POINT('Ctrl Pts',(-38.8425245364703,-2.63811170798816,
-3.48615825902432));
#54440=CARTESIAN_POINT('Ctrl Pts',(-38.6436510047728,1.50667621358083,-4.10400530923358));
#54441=CARTESIAN_POINT('Ctrl Pts',(-38.4447774730754,4.2671269364948,-0.951083854677481));
#54442=CARTESIAN_POINT('Ctrl Pts',(-38.2459039413779,3.10693266858264,3.07569539839068));
#54443=CARTESIAN_POINT('Ctrl Pts',(-38.0470304096805,-0.907917714602892,
4.27651940417648));
#54444=CARTESIAN_POINT('Ctrl Pts',(-37.848156877983,-4.08857143740867,1.54806860054497));
#54445=CARTESIAN_POINT('Ctrl Pts',(-37.6492833462856,-3.51263732857192,
-2.60275081187394));
#54446=CARTESIAN_POINT('Ctrl Pts',(-37.4504098145881,0.290715170158508,
-4.36215743418637));
#54447=CARTESIAN_POINT('Ctrl Pts',(-37.2515362828907,3.82695797362988,-2.11360484927016));
#54448=CARTESIAN_POINT('Ctrl Pts',(-37.0526627511932,3.84698393314227,2.07693221096233));
#54449=CARTESIAN_POINT('Ctrl Pts',(-36.8537892194957,0.332393155976931,
4.3591796912547));
#54450=CARTESIAN_POINT('Ctrl Pts',(-36.6549156877984,-3.48760113539375,
2.63620392063813));
#54451=CARTESIAN_POINT('Ctrl Pts',(-36.4560421561008,-4.10318034256891,
-1.50892142510596));
#54452=CARTESIAN_POINT('Ctrl Pts',(-36.2571686244034,-0.948749026044068,
-4.26764666723571));
#54453=CARTESIAN_POINT('Ctrl Pts',(-36.0582950927059,3.07739484365031,-3.10524938886745));
#54454=CARTESIAN_POINT('Ctrl Pts',(-35.8594215610085,4.27602201226846,0.910257403915468));
#54455=CARTESIAN_POINT('Ctrl Pts',(-35.660548029311,1.54583137617576,4.08941782497438));
#54456=CARTESIAN_POINT('Ctrl Pts',(-35.4616744976137,-2.60467230236045,
3.51121275175743));
#54457=CARTESIAN_POINT('Ctrl Pts',(-35.2628009659161,-4.36199772138568,
-0.293101807251095));
#54458=CARTESIAN_POINT('Ctrl Pts',(-35.0639274342188,-2.11151067763145,
-3.82811382393941));
#54459=CARTESIAN_POINT('Ctrl Pts',(-34.8650539025212,2.07903671223751,-3.84584699903108));
#54460=CARTESIAN_POINT('Ctrl Pts',(-34.6661803708238,4.35936090207359,-0.330008054840811));
#54461=CARTESIAN_POINT('Ctrl Pts',(-34.4673068391263,2.63429534412827,3.48904296773367));
#54462=CARTESIAN_POINT('Ctrl Pts',(-34.2684333074289,-1.51116618492849,
4.10235414759823));
#54463=CARTESIAN_POINT('Ctrl Pts',(-34.0695597757314,-4.26816512043681,
0.946413913398328));
#54464=CARTESIAN_POINT('Ctrl Pts',(-33.8706862440339,-3.10356517958156,
-3.0790933676776));
#54465=CARTESIAN_POINT('Ctrl Pts',(-33.6718127123365,0.912596820738402,
-4.27552334031354));
#54466=CARTESIAN_POINT('Ctrl Pts',(-33.472939180639,4.09026298835399,-1.5435936890546));
#54467=CARTESIAN_POINT('Ctrl Pts',(-33.2740656489416,3.5097871238451,2.60659301312629));
#54468=CARTESIAN_POINT('Ctrl Pts',(-33.0751921172442,-0.295488356602298,
4.3618367028008));
#54469=CARTESIAN_POINT('Ctrl Pts',(-32.8763185855467,-3.82926852828537,
2.10941587390226));
#54470=CARTESIAN_POINT('Ctrl Pts',(-32.6774450538493,-3.8447089136478,-2.08114059114343));
#54471=CARTESIAN_POINT('Ctrl Pts',(-32.4785715221517,-0.327622854915255,
-4.35954080789764));
#54472=CARTESIAN_POINT('Ctrl Pts',(-32.2796979904543,3.49048375561245,-2.63238597902992));
#54473=CARTESIAN_POINT('Ctrl Pts',(-32.0808244587569,4.10152672456885,1.51341049237635));
#54474=CARTESIAN_POINT('Ctrl Pts',(-31.8819509270594,0.944078517439236,
4.26868229594298));
#54475=CARTESIAN_POINT('Ctrl Pts',(-31.683077395362,-3.08079096996409,3.1018800412291));
#54476=CARTESIAN_POINT('Ctrl Pts',(-31.4842038636645,-4.27502338846088,
-0.914935964371331));
#54477=CARTESIAN_POINT('Ctrl Pts',(-31.2853303319671,-1.54135553985154,
-4.09110692729445));
#54478=CARTESIAN_POINT('Ctrl Pts',(-31.0864568002696,2.60851294359646,-3.50836044526178));
#54479=CARTESIAN_POINT('Ctrl Pts',(-30.8875832685722,4.36167437847994,0.297874817497696));
#54480=CARTESIAN_POINT('Ctrl Pts',(-30.6887097368746,2.10732043870968,3.8304220863221));
#54481=CARTESIAN_POINT('Ctrl Pts',(-30.4898362051773,-2.0832438470503,3.84356967733313));
#54482=CARTESIAN_POINT('Ctrl Pts',(-30.2909626734798,-4.35971940867296,
0.325237556914354));
#54483=CARTESIAN_POINT('Ctrl Pts',(-30.0920891417824,-2.63047582591478,
-3.49192349859863));
#54484=CARTESIAN_POINT('Ctrl Pts',(-29.8932156100849,1.51565434677771,-4.1006980737286));
#54485=CARTESIAN_POINT('Ctrl Pts',(-29.6943420783874,4.26919819359942,-0.941742838865859));
#54486=CARTESIAN_POINT('Ctrl Pts',(-29.49546854669,3.10019397431441,3.08248765000159));
#54487=CARTESIAN_POINT('Ctrl Pts',(-29.2965950149925,-0.917274834113944,
4.27452215686021));
#54488=CARTESIAN_POINT('Ctrl Pts',(-29.0977214832951,-4.09194964154314,
1.53911692923657));
#54489=CARTESIAN_POINT('Ctrl Pts',(-28.8988479515976,-3.50693271643453,
-2.61043209319622));
#54490=CARTESIAN_POINT('Ctrl Pts',(-28.6999744199002,0.300261189222895,
-4.36151074847169));
#54491=CARTESIAN_POINT('Ctrl Pts',(-28.5011008882027,3.83157449770426,-2.10522437268097));
#54492=CARTESIAN_POINT('Ctrl Pts',(-28.3022273565052,3.84242929042812,2.0853464793284));
#54493=CARTESIAN_POINT('Ctrl Pts',(-28.1033538248078,0.322852161552108,
4.35989670434615));
#54494=CARTESIAN_POINT('Ctrl Pts',(-27.9044802931104,-3.4933621962615,2.6285648853545));
#54495=CARTESIAN_POINT('Ctrl Pts',(-27.7056067614129,-4.09986819532533,
-1.5178977474611));
#54496=CARTESIAN_POINT('Ctrl Pts',(-27.5067332297155,-0.939406878377322,
-4.26971281325161));
#54497=CARTESIAN_POINT('Ctrl Pts',(-27.307859698018,3.08418340728215,-3.09850697934234));
#54498=CARTESIAN_POINT('Ctrl Pts',(-27.1089861663205,4.27401964566158,0.919613429266095));
#54499=CARTESIAN_POINT('Ctrl Pts',(-26.9101126346231,1.53687785787983,4.09279113084779));
#54500=CARTESIAN_POINT('Ctrl Pts',(-26.7112391029256,-2.61235046135107,
3.50550393779077));
#54501=CARTESIAN_POINT('Ctrl Pts',(-26.5123655712282,-4.36134581282504,
-0.302647471063524));
#54502=CARTESIAN_POINT('Ctrl Pts',(-26.3134920395307,-2.10312767644367,
-3.83272576208681));
#54503=CARTESIAN_POINT('Ctrl Pts',(-26.1146185078333,2.08744848734839,-3.84128775327418));
#54504=CARTESIAN_POINT('Ctrl Pts',(-25.9157449761358,4.36007269486416,-0.320466669542563));
#54505=CARTESIAN_POINT('Ctrl Pts',(-25.7168714444384,2.62665315792108,3.49479984817026));
#54506=CARTESIAN_POINT('Ctrl Pts',(-25.5179979127409,-1.52014069375477,
4.09903708960756));
#54507=CARTESIAN_POINT('Ctrl Pts',(-25.3191243810434,-4.27022615474555,
0.937070636672996));
#54508=CARTESIAN_POINT('Ctrl Pts',(-25.120250849346,-3.09681905681786,-3.08587824129815));
#54509=CARTESIAN_POINT('Ctrl Pts',(-24.9213773176485,0.921951749127709,
-4.27351585501541));
#54510=CARTESIAN_POINT('Ctrl Pts',(-24.7225037859511,4.0936313949565,-1.53463832645159));
#54511=CARTESIAN_POINT('Ctrl Pts',(-24.5236302542536,3.5040741097582,2.61426804748663));
#54512=CARTESIAN_POINT('Ctrl Pts',(-24.3247567225562,-0.305033662305041,
4.36117957158933));
#54513=CARTESIAN_POINT('Ctrl Pts',(-24.1258831908588,-3.83387587912521,
2.1010303506255));
#54514=CARTESIAN_POINT('Ctrl Pts',(-23.9270096591612,-3.84014506621302,
-2.08954987048108));
#54515=CARTESIAN_POINT('Ctrl Pts',(-23.7281361274639,-0.318081081599751,
-4.3602473801742));
#54516=CARTESIAN_POINT('Ctrl Pts',(-23.5292625957663,3.49623645389453,-2.6247406441869));
#54517=CARTESIAN_POINT('Ctrl Pts',(-23.3303890640689,4.09820475682409,1.5223831849873));
#54518=CARTESIAN_POINT('Ctrl Pts',(-23.1315155323714,0.934734114452248,
4.27073821792754));
#54519=CARTESIAN_POINT('Ctrl Pts',(-22.932642000674,-3.08757215154224,3.09513020724629));
#54520=CARTESIAN_POINT('Ctrl Pts',(-22.7337684689765,-4.27301078507249,
-0.924289792998811));
#54521=CARTESIAN_POINT('Ctrl Pts',(-22.5348949372791,-1.53239833562235,
-4.09447043361766));
#54522=CARTESIAN_POINT('Ctrl Pts',(-22.3360214055817,2.61618485102899,-3.50264323276489));
#54523=CARTESIAN_POINT('Ctrl Pts',(-22.1371478738842,4.36101202481442,0.307419762233428));
#54524=CARTESIAN_POINT('Ctrl Pts',(-21.9382743421868,2.09893239585401,3.8350248484752));
#54525=CARTESIAN_POINT('Ctrl Pts',(-21.7394008104893,-2.09165062809739,
3.8390012295866));
#54526=CARTESIAN_POINT('Ctrl Pts',(-21.5405272787919,-4.36042076022404,
0.315695398437909));
#54527=CARTESIAN_POINT('Ctrl Pts',(-21.3416537470944,-2.62282734472448,
-3.49767201300425));
#54528=CARTESIAN_POINT('Ctrl Pts',(-21.1427802153969,1.52462522048738,-4.09737119722407));
#54529=CARTESIAN_POINT('Ctrl Pts',(-20.9439066836995,4.2712490026443,-0.932397312414519));
#54530=CARTESIAN_POINT('Ctrl Pts',(-20.745033152002,3.09344043113318,3.08926513750733));
#54531=CARTESIAN_POINT('Ctrl Pts',(-20.5461596203046,-0.926627560179405,
4.27250443598403));
#54532=CARTESIAN_POINT('Ctrl Pts',(-20.3472860886071,-4.09530824658019,
1.5301578860626));
#54533=CARTESIAN_POINT('Ctrl Pts',(-20.1484125569097,-3.50121130723917,
-2.61810087140436));
#54534=CARTESIAN_POINT('Ctrl Pts',(-19.9495390252122,0.309805770134372,
-4.36084317255037));
#54535=CARTESIAN_POINT('Ctrl Pts',(-19.7506654935148,3.83617266979276,-2.09683381275741));
#54536=CARTESIAN_POINT('Ctrl Pts',(-19.5517919618172,3.83785624373743,2.09375075956842));
#54537=CARTESIAN_POINT('Ctrl Pts',(-19.3529184301199,0.313309620771175,
4.36059283496176));
#54538=CARTESIAN_POINT('Ctrl Pts',(-19.1540448984224,-3.49910652506968,
2.62091326010657));
#54539=CARTESIAN_POINT('Ctrl Pts',(-18.9551713667249,-4.09653641105705,
-1.52686679958387));
#54540=CARTESIAN_POINT('Ctrl Pts',(-18.7562978350275,-0.930060231259401,
-4.27175850874285));
#54541=CARTESIAN_POINT('Ctrl Pts',(-18.55742430333,3.09095719868646,-3.09174972898448));
#54542=CARTESIAN_POINT('Ctrl Pts',(-18.3585507716326,4.27199680790173,0.928965049969675));
#54543=CARTESIAN_POINT('Ctrl Pts',(-18.1596772399351,1.52791697844301,4.09614483359332));
#54544=CARTESIAN_POINT('Ctrl Pts',(-17.9608037082377,-2.62001610803916,
3.49977833360957));
#54545=CARTESIAN_POINT('Ctrl Pts',(-17.7619301765402,-4.36067301484774,
-0.31219168529352));
#54546=CARTESIAN_POINT('Ctrl Pts',(-17.5630566448428,-2.09473460196391,
-3.8373193427343));
#54547=CARTESIAN_POINT('Ctrl Pts',(-17.3641831131453,2.09585026426548,-3.83671010900824));
#54548=CARTESIAN_POINT('Ctrl Pts',(-17.1653095814479,4.36076360433587,-0.310923749313768));
#54549=CARTESIAN_POINT('Ctrl Pts',(-16.9664360497504,2.61899839090615,3.5005399896614));
#54550=CARTESIAN_POINT('Ctrl Pts',(-16.7675625180529,-1.52910792160562,
4.09570039857291));
#54551=CARTESIAN_POINT('Ctrl Pts',(-16.5686889863555,-4.27226673607081,
0.927722871686493));
#54552=CARTESIAN_POINT('Ctrl Pts',(-16.369815454658,-3.09005810130619,-3.0926483345734));
#54553=CARTESIAN_POINT('Ctrl Pts',(-16.1709419229606,0.931302261670127,
-4.27148790097734));
#54554=CARTESIAN_POINT('Ctrl Pts',(-15.9720683912631,4.09698019440654,-1.52567561343433));
#54555=CARTESIAN_POINT('Ctrl Pts',(-15.7731948595657,3.49834431230515,2.62193056036003));
#54556=CARTESIAN_POINT('Ctrl Pts',(-15.5743213278682,-0.314577506996647,
4.36050155175749));
#54557=CARTESIAN_POINT('Ctrl Pts',(-15.3754477961708,-3.83846486695655,
2.09263476410191));
#54558=CARTESIAN_POINT('Ctrl Pts',(-15.1765742644733,-3.83556282574215,
-2.09794914156006));
#54559=CARTESIAN_POINT('Ctrl Pts',(-14.9777007327758,-0.308537784779887,
-4.36093306829522));
#54560=CARTESIAN_POINT('Ctrl Pts',(-14.7788272010784,3.50197240635021,-2.61708273769649));
#54561=CARTESIAN_POINT('Ctrl Pts',(-14.579953669381,4.09486316002196,1.53134858588184));
#54562=CARTESIAN_POINT('Ctrl Pts',(-14.3810801376835,0.925385234395442,
4.27277368447599));
#54563=CARTESIAN_POINT('Ctrl Pts',(-14.182206605986,-3.09433854466179,3.08836554860464));
#54564=CARTESIAN_POINT('Ctrl Pts',(-13.9833330742886,-4.2709777153633,-0.933639194580945));
#54565=CARTESIAN_POINT('Ctrl Pts',(-13.7844595425911,-1.5234337917076,-4.0978143287698));
#54566=CARTESIAN_POINT('Ctrl Pts',(-13.5855860108937,2.62384422779387,-3.49690924375519));
#54567=CARTESIAN_POINT('Ctrl Pts',(-13.3867124791962,4.36032878333094,0.316963234529536));
#54568=CARTESIAN_POINT('Ctrl Pts',(-13.1878389474988,2.09053429980003,3.83960924211661));
#54569=CARTESIAN_POINT('Ctrl Pts',(-12.9889654158013,-2.1000473908238,3.83441439428258));
#54570=CARTESIAN_POINT('Ctrl Pts',(-12.7900918841039,-4.36110122678905,
0.30615172788398));
#54571=CARTESIAN_POINT('Ctrl Pts',(-12.5912183524064,-2.61516630105115,
-3.5034037747074));
#54572=CARTESIAN_POINT('Ctrl Pts',(-12.3923448207089,1.53358879174183,-4.09402469565482));
#54573=CARTESIAN_POINT('Ctrl Pts',(-12.1934712890115,4.27327935380661,-0.923047320085955));
#54574=CARTESIAN_POINT('Ctrl Pts',(-11.994597757314,3.08667207138658,3.09602782844563));
#54575=CARTESIAN_POINT('Ctrl Pts',(-11.7957242256166,-0.935975848002548,
4.27046625121234));
#54576=CARTESIAN_POINT('Ctrl Pts',(-11.5968506939192,-4.09864723643339,
1.52119151393392));
#54577=CARTESIAN_POINT('Ctrl Pts',(-11.3979771622217,-3.49547312838928,
-2.6257571097678));
#54578=CARTESIAN_POINT('Ctrl Pts',(-11.1991036305242,0.319348867178025,
-4.36015470961981));
#54579=CARTESIAN_POINT('Ctrl Pts',(-11.0002300988268,3.84075246787181,-2.08843320968709));
#54580=CARTESIAN_POINT('Ctrl Pts',(-10.8013565671293,3.8332648149734,2.10214501142864));
#54581=CARTESIAN_POINT('Ctrl Pts',(-10.6024830354319,0.303765579340042,
4.36126807976715));
#54582=CARTESIAN_POINT('Ctrl Pts',(-10.4036095037344,-3.50483409430456,
2.61324908154353));
#54583=CARTESIAN_POINT('Ctrl Pts',(-10.204735972037,-4.09318500572241,-1.53582853851505));
#54584=CARTESIAN_POINT('Ctrl Pts',(-10.0058624403395,-0.920709129457893,
-4.27378374391132));
#54585=CARTESIAN_POINT('Ctrl Pts',(-9.80698890864207,3.09771618541933,-3.08497767015885));
#54586=CARTESIAN_POINT('Ctrl Pts',(-9.60811537694459,4.26995350867754,0.938312221235545));
#54587=CARTESIAN_POINT('Ctrl Pts',(-9.40924184524716,1.51894878078439,4.09947891714805));
#54588=CARTESIAN_POINT('Ctrl Pts',(-9.21036831354968,-2.62766920570929,
3.49403596663726));
#54589=CARTESIAN_POINT('Ctrl Pts',(-9.01149478185225,-4.35997933067613,
-0.321734404227933));
#54590=CARTESIAN_POINT('Ctrl Pts',(-8.81262125015477,-2.08633149439201,
-3.8418945438801));
#54591=CARTESIAN_POINT('Ctrl Pts',(-8.61374771845735,2.10424200274676,-3.83211408815864));
#54592=CARTESIAN_POINT('Ctrl Pts',(-8.41487418675987,4.36143362717948,-0.30137933986224));
#54593=CARTESIAN_POINT('Ctrl Pts',(-8.21600065506241,2.61133107974759,3.50626336471347));
#54594=CARTESIAN_POINT('Ctrl Pts',(-8.01712712336498,-1.53806782553083,
4.09234409047605));
#54595=CARTESIAN_POINT('Ctrl Pts',(-7.81825359166752,-4.27428685463917,
0.91837066321142));
#54596=CARTESIAN_POINT('Ctrl Pts',(-7.61938005997006,-3.08328234542873,
-3.09940361507732));
#54597=CARTESIAN_POINT('Ctrl Pts',(-7.42050652827261,0.940648313580007,
-4.26943948791234));
#54598=CARTESIAN_POINT('Ctrl Pts',(-7.22163299657514,4.10030937066533,-1.51670559293085));
#54599=CARTESIAN_POINT('Ctrl Pts',(-7.0227594648777,3.49259775892826,2.62958051504615));
#54600=CARTESIAN_POINT('Ctrl Pts',(-6.82388593318022,-0.324119844963001,
4.35980264655192));
#54601=CARTESIAN_POINT('Ctrl Pts',(-6.62501240148279,-3.84303546980398,
2.08422915454508));
#54602=CARTESIAN_POINT('Ctrl Pts',(-6.42613886978531,-3.83096221417432,
-2.10633836415309));
#54603=CARTESIAN_POINT('Ctrl Pts',(-6.22726533808787,-0.29899301018082,
-4.36159786897168));
#54604=CARTESIAN_POINT('Ctrl Pts',(-6.02839180639044,3.5076915855359,-2.60941229624663));
#54605=CARTESIAN_POINT('Ctrl Pts',(-5.82951827469298,4.09150195011159,1.54030665213598));
#54606=CARTESIAN_POINT('Ctrl Pts',(-5.63064474299553,0.91603192215228,4.2747886858071));
#54607=CARTESIAN_POINT('Ctrl Pts',(-5.43177121129806,-3.10109011711434,
3.08158609776497));
#54608=CARTESIAN_POINT('Ctrl Pts',(-5.23289767960062,-4.26892418869336,
-0.942984124452568));
#54609=CARTESIAN_POINT('Ctrl Pts',(-5.03402414790315,-1.51446195175697,
-4.10113859651792));
#54610=CARTESIAN_POINT('Ctrl Pts',(-4.83515061620571,2.63149103855122,-3.49115850610583));
#54611=CARTESIAN_POINT('Ctrl Pts',(-4.63627708450823,4.35962465476036,0.326505189448822));
#54612=CARTESIAN_POINT('Ctrl Pts',(-4.43740355281079,2.0821261955711,3.84417524382889));
#54613=CARTESIAN_POINT('Ctrl Pts',(-4.23853002111335,-2.10843410407346,
3.8298091961466));
#54614=CARTESIAN_POINT('Ctrl Pts',(-4.0396564894159,-4.36176078799866,0.296606585759418));
#54615=CARTESIAN_POINT('Ctrl Pts',(-3.84078295771845,-2.60749276389598,
-3.509118746429));
#54616=CARTESIAN_POINT('Ctrl Pts',(-3.64190942602098,1.54254507861259,-4.09065860360309));
#54617=CARTESIAN_POINT('Ctrl Pts',(-3.44303589432354,4.27528912217474,-0.913692871629554));
#54618=CARTESIAN_POINT('Ctrl Pts',(-3.24416236262607,3.0798891449889,3.10277562427561));
#54619=CARTESIAN_POINT('Ctrl Pts',(-3.04528883092862,-0.945320063486189,
4.26840773721229));
#54620=CARTESIAN_POINT('Ctrl Pts',(-2.84641529923116,-4.10196581966695,
1.51221761995006));
#54621=CARTESIAN_POINT('Ctrl Pts',(-2.6475417675337,-3.48971967156313,-2.63340032628982));
#54622=CARTESIAN_POINT('Ctrl Pts',(-2.44866823583628,0.328893199341695,
-4.35944620384304));
#54623=CARTESIAN_POINT('Ctrl Pts',(-2.24979470413881,3.84530864969658,-2.08002101598113));
#54624=CARTESIAN_POINT('Ctrl Pts',(-2.05092117244137,3.82866488313315,2.11052619675534));
#54625=CARTESIAN_POINT('Ctrl Pts',(-1.85204764074389,0.294201470937102,
4.36192809626536));
#54626=CARTESIAN_POINT('Ctrl Pts',(-1.65317410904645,-3.51050973320713,
2.60556169774132));
#54627=CARTESIAN_POINT('Ctrl Pts',(-1.45430057734899,-4.08988035329247,
-1.54476273894195));
#54628=CARTESIAN_POINT('Ctrl Pts',(-1.25542704565154,-0.911228319106154,
-4.27582661814505));
#54629=CARTESIAN_POINT('Ctrl Pts',(-1.05655351395407,3.10422373424832,-3.07811887241764));
#54630=CARTESIAN_POINT('Ctrl Pts',(-0.857679982256619,4.26833660246525,
0.947518975425125));
#54631=CARTESIAN_POINT('Ctrl Pts',(-0.658806450559178,1.5091288044425,4.1030503614686));
#54632=CARTESIAN_POINT('Ctrl Pts',(-0.459932918861728,-2.63370883009196,
3.48778877601057));
#54633=CARTESIAN_POINT('Ctrl Pts',(-0.261059387164271,-4.36233900073485,
-0.330330886159537));
#54634=CARTESIAN_POINT('Ctrl Pts',(-0.0621858554668183,-2.07169497223652,
-3.84842048673565));
#54635=CARTESIAN_POINT('Ctrl Pts',(0.0703964989981522,0.707860675536127,
-3.83120820981452));
#54636=CARTESIAN_POINT('Ctrl Pts',(0.136687676230641,1.78615774484833,-3.23603222682011));
#54637=CARTESIAN_POINT('Ctrl Pts',(-109.703687676231,2.00907721869499,-2.81633609132873));
#54638=CARTESIAN_POINT('Ctrl Pts',(-109.637396498998,2.94752490419964,-2.14687981738136));
#54639=CARTESIAN_POINT('Ctrl Pts',(-109.504814144533,4.08614741056074,0.19228903229402));
#54640=CARTESIAN_POINT('Ctrl Pts',(-109.305940612836,2.043016874263,3.5485133391066));
#54641=CARTESIAN_POINT('Ctrl Pts',(-109.107067081138,-1.87881404914145,
3.63353969641206));
#54642=CARTESIAN_POINT('Ctrl Pts',(-108.908193549441,-4.07356171499593,
0.385530372585237));
#54643=CARTESIAN_POINT('Ctrl Pts',(-108.709320017743,-2.5259486660199,-3.21956889940024));
#54644=CARTESIAN_POINT('Ctrl Pts',(-108.510446486046,1.34274209597358,-3.86500887175455));
#54645=CARTESIAN_POINT('Ctrl Pts',(-108.311572954348,3.97759639348424,-0.960071453599377));
#54646=CARTESIAN_POINT('Ctrl Pts',(-108.112699422651,2.9578917106467,2.82740558092371));
#54647=CARTESIAN_POINT('Ctrl Pts',(-107.913825890954,-0.779564242600549,
4.01683202078962));
#54648=CARTESIAN_POINT('Ctrl Pts',(-107.714952359256,-3.80073680723715,
1.51570386947904));
#54649=CARTESIAN_POINT('Ctrl Pts',(-107.516078827559,-3.32979420802159,
-2.37811908816307));
#54650=CARTESIAN_POINT('Ctrl Pts',(-107.317205295861,0.200575240540261,
-4.08688799081147));
#54651=CARTESIAN_POINT('Ctrl Pts',(-107.118331764164,3.54665304843382,-2.04063348034382));
#54652=CARTESIAN_POINT('Ctrl Pts',(-106.919458232466,3.63406018195941,1.88056861694301));
#54653=CARTESIAN_POINT('Ctrl Pts',(-106.720584700769,0.382484601897899,
4.07389545316324));
#54654=CARTESIAN_POINT('Ctrl Pts',(-106.521711169071,-3.22051821498825,
2.52412140612187));
#54655=CARTESIAN_POINT('Ctrl Pts',(-106.322837637374,-3.86450249557726,
-1.34482196121329));
#54656=CARTESIAN_POINT('Ctrl Pts',(-106.123964105676,-0.957773835952048,
-3.9781394133409));
#54657=CARTESIAN_POINT('Ctrl Pts',(-105.925090573979,2.82895933118871,-2.95633459405304));
#54658=CARTESIAN_POINT('Ctrl Pts',(-105.726217042281,4.01643888773492,0.78175672683345));
#54659=CARTESIAN_POINT('Ctrl Pts',(-105.527343510584,1.5136061306901,3.80156825262383));
#54660=CARTESIAN_POINT('Ctrl Pts',(-105.328469978887,-2.37993103823623,
3.32849112014495));
#54661=CARTESIAN_POINT('Ctrl Pts',(-105.129596447189,-4.08678268726703,
-0.20281051848524));
#54662=CARTESIAN_POINT('Ctrl Pts',(-104.930722915492,-2.03869000947797,
-3.54776942006687));
#54663=CARTESIAN_POINT('Ctrl Pts',(-104.731849383794,1.88255523369223,-3.63303050255371));
#54664=CARTESIAN_POINT('Ctrl Pts',(-104.532975852097,4.07410486344261,-0.380255695137597));
#54665=CARTESIAN_POINT('Ctrl Pts',(-104.334102320399,2.52235857904578,3.22189882332731));
#54666=CARTESIAN_POINT('Ctrl Pts',(-104.135228788702,-1.34693594667287,
3.86376608876015));
#54667=CARTESIAN_POINT('Ctrl Pts',(-103.936355257004,-3.9786629590652,0.955597137798683));
#54668=CARTESIAN_POINT('Ctrl Pts',(-103.737481725307,-2.95478627533421,
-2.83057642511528));
#54669=CARTESIAN_POINT('Ctrl Pts',(-103.538608193609,0.783954105126475,
-4.01601055687818));
#54670=CARTESIAN_POINT('Ctrl Pts',(-103.339734661912,3.80239584414084,-1.51152594291659));
#54671=CARTESIAN_POINT('Ctrl Pts',(-103.140861130215,3.3271884741954,2.38175181091827));
#54672=CARTESIAN_POINT('Ctrl Pts',(-102.941987598517,-0.205046497461266,
4.08667111052397));
#54673=CARTESIAN_POINT('Ctrl Pts',(-102.74311406682,-3.54888432623646,2.03674860271566));
#54674=CARTESIAN_POINT('Ctrl Pts',(-102.544240535122,-3.63199994923757,
-1.88454270325992));
#54675=CARTESIAN_POINT('Ctrl Pts',(-102.345367003425,-0.37802656139399,
-4.07431230400465));
#54676=CARTESIAN_POINT('Ctrl Pts',(-102.146493471727,3.2232784072503,-2.520595394154));
#54677=CARTESIAN_POINT('Ctrl Pts',(-101.94761994003,3.8630285570437,1.34904973931353));
#54678=CARTESIAN_POINT('Ctrl Pts',(-101.748746408332,0.953420136774898,
3.97918520233359));
#54679=CARTESIAN_POINT('Ctrl Pts',(-101.549872876635,-2.83219266279414,
2.95323713109742));
#54680=CARTESIAN_POINT('Ctrl Pts',(-101.350999344938,-4.01558102852441,
-0.786151279991661));
#54681=CARTESIAN_POINT('Ctrl Pts',(-101.15212581324,-1.50944530016411,-3.80322228084165));
#54682=CARTESIAN_POINT('Ctrl Pts',(-100.953252281543,2.38357186928961,-3.32588484100231));
#54683=CARTESIAN_POINT('Ctrl Pts',(-100.754378749845,4.0865583111173,0.20728241969803));
#54684=CARTESIAN_POINT('Ctrl Pts',(-100.555505218148,2.03480658587235,3.54999816757252));
#54685=CARTESIAN_POINT('Ctrl Pts',(-100.35663168645,-1.88652960848464,3.63096830996754));
#54686=CARTESIAN_POINT('Ctrl Pts',(-100.157758154753,-4.07451852500647,
0.375797313796782));
#54687=CARTESIAN_POINT('Ctrl Pts',(-99.9588846230556,-2.51883145465525,
-3.22465702590479));
#54688=CARTESIAN_POINT('Ctrl Pts',(-99.7600110913579,1.35116312808074,-3.86228986910522));
#54689=CARTESIAN_POINT('Ctrl Pts',(-99.5611375596606,3.97970625442996,-0.951242850237956));
#54690=CARTESIAN_POINT('Ctrl Pts',(-99.362264027963,2.95168710278726,2.8338080525888));
#54691=CARTESIAN_POINT('Ctrl Pts',(-99.1633904962657,-0.788348219514519,
4.01515029811662));
#54692=CARTESIAN_POINT('Ctrl Pts',(-98.9645169645681,-3.80404757903259,
1.50736420553696));
#54693=CARTESIAN_POINT('Ctrl Pts',(-98.7656434328706,-3.32458021218899,
-2.38539121411965));
#54694=CARTESIAN_POINT('Ctrl Pts',(-98.5667699011732,0.209518279883212,
-4.08644428838477));
#54695=CARTESIAN_POINT('Ctrl Pts',(-98.3678963694758,3.55111094620056,-2.03286395989802));
#54696=CARTESIAN_POINT('Ctrl Pts',(-98.1690228377782,3.62993558375018,1.88851594896682));
#54697=CARTESIAN_POINT('Ctrl Pts',(-97.970149306081,0.373567953702973,4.07472352628297));
#54698=CARTESIAN_POINT('Ctrl Pts',(-97.7712757743833,-3.22603467924333,
2.51706676113231));
#54699=CARTESIAN_POINT('Ctrl Pts',(-97.5724022426861,-3.86155002497238,
-1.35327611237084));
#54700=CARTESIAN_POINT('Ctrl Pts',(-97.3735287109885,-0.949065278942077,
-3.98022611518296));
#54701=CARTESIAN_POINT('Ctrl Pts',(-97.1746551792911,2.83542259406991,-2.95013619087587));
#54702=CARTESIAN_POINT('Ctrl Pts',(-96.9757816475935,4.01471836575504,0.790544923041662));
#54703=CARTESIAN_POINT('Ctrl Pts',(-96.7769081158962,1.50528265967335,3.80487173846432));
#54704=CARTESIAN_POINT('Ctrl Pts',(-96.5780345841988,-2.3872098448718,3.3232745881472));
#54705=CARTESIAN_POINT('Ctrl Pts',(-96.3791610525012,-4.08632904235626,
-0.211754077348115));
#54706=CARTESIAN_POINT('Ctrl Pts',(-96.1802875208037,-2.03092072537648,
-3.55222266178712));
#54707=CARTESIAN_POINT('Ctrl Pts',(-95.9814139891064,1.89050172411301,-3.62890177089481));
#54708=CARTESIAN_POINT('Ctrl Pts',(-95.7825404574088,4.07492730777215,-0.371338481779884));
#54709=CARTESIAN_POINT('Ctrl Pts',(-95.5836669257115,2.51530131411378,3.22741136685351));
#54710=CARTESIAN_POINT('Ctrl Pts',(-95.3847933940139,-1.35538869155151,
3.86080902486668));
#54711=CARTESIAN_POINT('Ctrl Pts',(-95.1859198623165,-3.98074478443685,
0.946887423539108));
#54712=CARTESIAN_POINT('Ctrl Pts',(-94.9870463306191,-2.94858439582757,
-2.83703628675417));
#54713=CARTESIAN_POINT('Ctrl Pts',(-94.7881727989216,0.792741389915535,
-4.01428523156895));
#54714=CARTESIAN_POINT('Ctrl Pts',(-94.5892992672241,3.8056947588901,-1.50320066319643));
#54715=CARTESIAN_POINT('Ctrl Pts',(-94.3904257355267,3.32196796926779,2.38902776100164));
#54716=CARTESIAN_POINT('Ctrl Pts',(-94.1915522038292,-0.213989811423434,
4.08621257306625));
#54717=CARTESIAN_POINT('Ctrl Pts',(-93.9926786721318,-3.55333331399942,
2.02897688288942));
#54718=CARTESIAN_POINT('Ctrl Pts',(-93.7938051404342,-3.62786687171092,
-1.89248693332876));
#54719=CARTESIAN_POINT('Ctrl Pts',(-93.594931608737,-0.369108898694929,
-4.075129869413));
#54720=CARTESIAN_POINT('Ctrl Pts',(-93.3960580770394,3.22878708832316,-2.5135351141282));
#54721=CARTESIAN_POINT('Ctrl Pts',(-93.197184545342,3.86006686900996,1.35750086499028));
#54722=CARTESIAN_POINT('Ctrl Pts',(-92.9983110136445,0.944709284681018,
3.98126226203641));
#54723=CARTESIAN_POINT('Ctrl Pts',(-92.799437481947,-2.83864913015849,2.94703171810691));
#54724=CARTESIAN_POINT('Ctrl Pts',(-92.6005639502496,-4.01385089568802,
-0.794937619478581));
#54725=CARTESIAN_POINT('Ctrl Pts',(-92.4016904185521,-1.50111821672946,
-3.80651664006356));
#54726=CARTESIAN_POINT('Ctrl Pts',(-92.2028168868548,2.39084496196498,-3.32066035594194));
#54727=CARTESIAN_POINT('Ctrl Pts',(-92.0039433551572,4.08609488054962,0.216225481439941));
#54728=CARTESIAN_POINT('Ctrl Pts',(-91.8050698234598,2.02703243301877,3.55444290250494));
#54729=CARTESIAN_POINT('Ctrl Pts',(-91.6061962917624,-1.89447157601982,
3.62683088650832));
#54730=CARTESIAN_POINT('Ctrl Pts',(-91.4073227600648,-4.07533121114487,
0.366879205115507));
#54731=CARTESIAN_POINT('Ctrl Pts',(-91.2084492283676,-2.51176816170427,
-3.23016184324044));
#54732=CARTESIAN_POINT('Ctrl Pts',(-91.0095756966699,1.35961263205489,-3.85932355762439));
#54733=CARTESIAN_POINT('Ctrl Pts',(-90.8107021649726,3.98177854782669,-0.942530863019847));
#54734=CARTESIAN_POINT('Ctrl Pts',(-90.611828633275,2.94547815817867,2.84026112380008));
#54735=CARTESIAN_POINT('Ctrl Pts',(-90.4129551015776,-0.797133611073388,
4.01341535824226));
#54736=CARTESIAN_POINT('Ctrl Pts',(-90.2140815698802,-3.80733738173865,
1.49903532089581));
#54737=CARTESIAN_POINT('Ctrl Pts',(-90.0152080381827,-3.31935174856106,
-2.39266144721782));
#54738=CARTESIAN_POINT('Ctrl Pts',(-89.8163345064853,0.218461086728334,
-4.0859759648416));
#54739=CARTESIAN_POINT('Ctrl Pts',(-89.6174609747877,3.55555142697156,-2.02508737634657));
#54740=CARTESIAN_POINT('Ctrl Pts',(-89.4185874430905,3.62579381559713,1.89645565159203));
#54741=CARTESIAN_POINT('Ctrl Pts',(-89.2197139113928,0.364649401709092,
4.07553133290752));
#54742=CARTESIAN_POINT('Ctrl Pts',(-89.0208403796955,-3.23153563119388,
2.51000045737091));
#54743=CARTESIAN_POINT('Ctrl Pts',(-88.8219668479979,-3.85857909093245,
-1.36172399211318));
#54744=CARTESIAN_POINT('Ctrl Pts',(-88.6230933163006,-0.940352159207695,
-3.98229364165315));
#54745=CARTESIAN_POINT('Ctrl Pts',(-88.424219784603,2.84187226719637,-2.94392371650794));
#54746=CARTESIAN_POINT('Ctrl Pts',(-88.2253462529057,4.01297861936206,0.799329364042572));
#54747=CARTESIAN_POINT('Ctrl Pts',(-88.0264727212081,1.496951976319,3.80815698366971));
#54748=CARTESIAN_POINT('Ctrl Pts',(-87.8275991895108,-2.39447721621638,
3.31804214751687));
#54749=CARTESIAN_POINT('Ctrl Pts',(-87.6287256578132,-4.08585582597779,
-0.220696626619384));
#54750=CARTESIAN_POINT('Ctrl Pts',(-87.4298521261159,-2.02314171345511,
-3.55665888706742));
#54751=CARTESIAN_POINT('Ctrl Pts',(-87.2309785944184,1.89843915945149,-3.62475565928779));
#54752=CARTESIAN_POINT('Ctrl Pts',(-87.0321050627209,4.07573023464101,-0.362419489143201));
#54753=CARTESIAN_POINT('Ctrl Pts',(-86.8332315310234,2.50823200165732,3.23290845177216));
#54754=CARTESIAN_POINT('Ctrl Pts',(-86.6343579993261,-1.36383494453309,
3.85783346915704));
#54755=CARTESIAN_POINT('Ctrl Pts',(-86.4354844676284,-3.9828075433616,0.938173173896801));
#54756=CARTESIAN_POINT('Ctrl Pts',(-86.2366109359312,-2.94236839356005,
-2.84348255986502));
#54757=CARTESIAN_POINT('Ctrl Pts',(-86.0377374042336,0.801524877728764,
-4.01254067917819));
#54758=CARTESIAN_POINT('Ctrl Pts',(-85.8388638725363,3.80897544561137,-1.49486818362271));
#54759=CARTESIAN_POINT('Ctrl Pts',(-85.6399903408386,3.31673155320144,2.39629226841711));
#54760=CARTESIAN_POINT('Ctrl Pts',(-85.4411168091414,-0.222932100443837,
4.08573446399413));
#54761=CARTESIAN_POINT('Ctrl Pts',(-85.2422432774438,-3.55776528246097,
2.02119544492689));
#54762=CARTESIAN_POINT('Ctrl Pts',(-85.0433697457463,-3.62371641789112,
-1.90042209900436));
#54763=CARTESIAN_POINT('Ctrl Pts',(-84.844496214049,-0.360189468085367,
-4.07592791628584));
#54764=CARTESIAN_POINT('Ctrl Pts',(-84.6456226823514,3.23428030456434,-2.50646279509289));
#54765=CARTESIAN_POINT('Ctrl Pts',(-84.446749150654,3.85708669252133,1.36594548868265));
#54766=CARTESIAN_POINT('Ctrl Pts',(-84.2478756189565,0.935993907739473,
3.98332025279822));
#54767=CARTESIAN_POINT('Ctrl Pts',(-84.0490020872593,-2.84509200132407,
2.94081218980056));
#54768=CARTESIAN_POINT('Ctrl Pts',(-83.8501285555615,-4.01210153782168,
-0.803720151474848));
#54769=CARTESIAN_POINT('Ctrl Pts',(-83.6512550238644,-1.49278394343067,
-3.80979276731864));
#54770=CARTESIAN_POINT('Ctrl Pts',(-83.4523814921666,2.39810660327672,-3.31541996600705));
#54771=CARTESIAN_POINT('Ctrl Pts',(-83.2535079604693,4.08561187892698,0.225167507532613));
#54772=CARTESIAN_POINT('Ctrl Pts',(-83.0546344287719,2.01924857134438,3.55887061282109));
#54773=CARTESIAN_POINT('Ctrl Pts',(-82.8557608970742,-1.90240446965716,
3.62267609171814));
#54774=CARTESIAN_POINT('Ctrl Pts',(-82.6568873653771,-4.07612437778279,
0.357959339203114));
#54775=CARTESIAN_POINT('Ctrl Pts',(-82.4580138336794,-2.5046928382072,-3.2356511891598));
#54776=CARTESIAN_POINT('Ctrl Pts',(-82.2591403019821,1.3680556239302,-3.85633876124889));
#54777=CARTESIAN_POINT('Ctrl Pts',(-82.0602667702846,3.9838317698095,-0.933814361387948));
#54778=CARTESIAN_POINT('Ctrl Pts',(-81.861393238587,2.93925510569533,2.84670059109168));
#54779=CARTESIAN_POINT('Ctrl Pts',(-81.6625197068898,-0.805915184623597,
4.01166119542403));
#54780=CARTESIAN_POINT('Ctrl Pts',(-81.4636461751921,-3.81060894854679,
1.49069925636689));
#54781=CARTESIAN_POINT('Ctrl Pts',(-81.2647726434948,-3.31410738632641,
-2.399920220252));
#54782=CARTESIAN_POINT('Ctrl Pts',(-81.0658991117973,0.227402847216426,
-4.08548807081304));
#54783=CARTESIAN_POINT('Ctrl Pts',(-80.8670255800998,3.55997487781682,-2.01730109329047));
#54784=CARTESIAN_POINT('Ctrl Pts',(-80.6681520484024,3.62163468108033,1.90438627081639));
#54785=CARTESIAN_POINT('Ctrl Pts',(-80.4692785167049,0.355729103164104,
4.07631961907303));
#54786=CARTESIAN_POINT('Ctrl Pts',(-80.2704049850075,-3.23702110514808,
2.50292213153017));
#54787=CARTESIAN_POINT('Ctrl Pts',(-80.07153145331,-3.85558967556364,-1.37016534964396));
#54788=CARTESIAN_POINT('Ctrl Pts',(-79.8726579216126,-0.93163453549478,
-3.98434209424231));
#54789=CARTESIAN_POINT('Ctrl Pts',(-79.6737843899152,2.84830832868632,-2.93769714171049));
#54790=CARTESIAN_POINT('Ctrl Pts',(-79.4749108582176,4.01121965211704,0.808109976517873));
#54791=CARTESIAN_POINT('Ctrl Pts',(-79.2760373265203,1.48861412305541,3.81142398905155));
#54792=CARTESIAN_POINT('Ctrl Pts',(-79.0771637948227,-2.40173311880008,
3.31279381455241));
#54793=CARTESIAN_POINT('Ctrl Pts',(-78.8782902631253,-4.08536303968935,
-0.229638118826185));
#54794=CARTESIAN_POINT('Ctrl Pts',(-78.6794167314278,-2.01535301134818,
-3.56107807711758));
#54795=CARTESIAN_POINT('Ctrl Pts',(-78.4805431997303,1.9063675018887,-3.62059218628946));
#54796=CARTESIAN_POINT('Ctrl Pts',(-78.281669668033,4.0765136400982,-0.353498760635994));
#54797=CARTESIAN_POINT('Ctrl Pts',(-78.0827961363354,2.50115067559183,3.23839005211916));
#54798=CARTESIAN_POINT('Ctrl Pts',(-77.8839226046381,-1.3722746651924,3.85483943568976));
#54799=CARTESIAN_POINT('Ctrl Pts',(-77.6850490729406,-3.98485122594388,
0.929454430712534));
#54800=CARTESIAN_POINT('Ctrl Pts',(-77.4861755412431,-2.93613829831247,
-2.84991521362661));
#54801=CARTESIAN_POINT('Ctrl Pts',(-77.2873020095457,0.810304526500643,
-4.01077690803296));
#54802=CARTESIAN_POINT('Ctrl Pts',(-77.0884284778482,3.81223788858895,-1.4865285441204));
#54803=CARTESIAN_POINT('Ctrl Pts',(-76.8895549461508,3.31147925107822,2.40354529837827));
#54804=CARTESIAN_POINT('Ctrl Pts',(-76.6906814144534,-0.231873321692669,
4.08523678559332));
#54805=CARTESIAN_POINT('Ctrl Pts',(-76.4918078827558,-3.56218021039318,
2.01340432610067));
#54806=CARTESIAN_POINT('Ctrl Pts',(-76.2929343510585,-3.61954860765759,
-1.90834816228115));
#54807=CARTESIAN_POINT('Ctrl Pts',(-76.0940608193609,-0.351268312286318,
-4.07670644080014));
#54808=CARTESIAN_POINT('Ctrl Pts',(-75.8951872876636,3.23975802966322,-2.49937847092243));
#54809=CARTESIAN_POINT('Ctrl Pts',(-75.6963137559659,3.85408804185186,1.37438356994404));
#54810=CARTESIAN_POINT('Ctrl Pts',(-75.4974402242687,0.927274047693834,
3.98535916476184));
#54811=CARTESIAN_POINT('Ctrl Pts',(-75.2985666925711,-2.85152124543167,
2.93457857596787));
#54812=CARTESIAN_POINT('Ctrl Pts',(-75.0996931608737,-4.01033296330422,
-0.81249883391509));
#54813=CARTESIAN_POINT('Ctrl Pts',(-74.9008196291762,-1.48444252018617,
-3.8130506469153));
#54814=CARTESIAN_POINT('Ctrl Pts',(-74.7019460974788,2.40535675844402,-3.31016369629741));
#54815=CARTESIAN_POINT('Ctrl Pts',(-74.5030725657813,4.0851093085628,0.234108455146787));
#54816=CARTESIAN_POINT('Ctrl Pts',(-74.304199034084,2.01145503813126,3.56328127731368));
#54817=CARTESIAN_POINT('Ctrl Pts',(-74.1053255023863,-1.91032825140077,
3.61850394549707));
#54818=CARTESIAN_POINT('Ctrl Pts',(-73.906451970689,-4.07689802112117,0.349037758782845));
#54819=CARTESIAN_POINT('Ctrl Pts',(-73.7075784389915,-2.49760551805255,
-3.24112503737069));
#54820=CARTESIAN_POINT('Ctrl Pts',(-73.5087049072941,1.37649206326759,-3.85333549427492));
#54821=CARTESIAN_POINT('Ctrl Pts',(-73.3098313755965,3.98586591054412,-0.92509338709135));
#54822=CARTESIAN_POINT('Ctrl Pts',(-73.1109578438992,2.93301797514357,2.85312642362068));
#54823=CARTESIAN_POINT('Ctrl Pts',(-72.9120843122017,-0.814692898104216,
4.00988781806376));
#54824=CARTESIAN_POINT('Ctrl Pts',(-72.7132107805042,-3.81386226378726,
1.48235605187727));
#54825=CARTESIAN_POINT('Ctrl Pts',(-72.5143372488068,-3.30884715060387,
-2.40716749845509));
#54826=CARTESIAN_POINT('Ctrl Pts',(-72.3154637171093,0.236343518519478,
-4.08498060863594));
#54827=CARTESIAN_POINT('Ctrl Pts',(-72.116590185412,3.56438127754945,-2.00950514802345));
#54828=CARTESIAN_POINT('Ctrl Pts',(-71.9177166537144,3.61745820012068,1.91230776865477));
#54829=CARTESIAN_POINT('Ctrl Pts',(-71.718843122017,0.346807100793382,4.07708838100389));
#54830=CARTESIAN_POINT('Ctrl Pts',(-71.5199695903195,-3.24249107483239,
2.49583181751297));
#54831=CARTESIAN_POINT('Ctrl Pts',(-71.321096058622,-3.85258179318421,-1.3786001445319));
#54832=CARTESIAN_POINT('Ctrl Pts',(-71.1222225269247,-0.922912449557835,
-3.986371463139));
#54833=CARTESIAN_POINT('Ctrl Pts',(-70.9233489952271,2.85473074771306,-2.93145649630679));
#54834=CARTESIAN_POINT('Ctrl Pts',(-70.7244754635297,4.00944147244488,0.816886718411246));
#54835=CARTESIAN_POINT('Ctrl Pts',(-70.5256019318323,1.48026913981821,3.81467273896198));
#54836=CARTESIAN_POINT('Ctrl Pts',(-70.3267284001348,-2.40897751786949,
3.30752961439156));
#54837=CARTESIAN_POINT('Ctrl Pts',(-70.1278548684374,-4.08485068585123,
-0.238578511141671));
#54838=CARTESIAN_POINT('Ctrl Pts',(-69.9289813367398,-2.007554656361,-3.56548021077119));
#54839=CARTESIAN_POINT('Ctrl Pts',(-69.7301078050425,1.91428671345058,-3.61641137184146));
#54840=CARTESIAN_POINT('Ctrl Pts',(-69.5312342733449,4.07727752039141,-0.344576338985572));
#54841=CARTESIAN_POINT('Ctrl Pts',(-69.3323607416475,2.49405736983453,3.24385614163944));
#54842=CARTESIAN_POINT('Ctrl Pts',(-69.1334872099502,-1.38070781310592,
3.85182693880529));
#54843=CARTESIAN_POINT('Ctrl Pts',(-68.9346136782525,-3.98687582239513,
0.920731235746244));
#54844=CARTESIAN_POINT('Ctrl Pts',(-68.7357401465552,-2.92989413992499,
-2.85633421722859));
#54845=CARTESIAN_POINT('Ctrl Pts',(-68.5368666148576,0.819080294179483,
-4.00899392658117));
#54846=CARTESIAN_POINT('Ctrl Pts',(-68.3379930831603,3.81548207219677,-1.47818178463369));
#54847=CARTESIAN_POINT('Ctrl Pts',(-68.1391195514627,3.30621108805498,2.41078681614534));
#54848=CARTESIAN_POINT('Ctrl Pts',(-67.9402460197655,-0.240813432344258,
4.08471954024756));
#54849=CARTESIAN_POINT('Ctrl Pts',(-67.7413724880678,-3.56657807664994,
2.0056035637278));
#54850=CARTESIAN_POINT('Ctrl Pts',(-67.5424989563705,-3.6153634609728,-1.91626508519584));
#54851=CARTESIAN_POINT('Ctrl Pts',(-67.343625424673,-0.342345474027202,
-4.07746543922704));
#54852=CARTESIAN_POINT('Ctrl Pts',(-67.1447518929755,3.24522023738312,-2.49228217554848));
#54853=CARTESIAN_POINT('Ctrl Pts',(-66.9458783612781,3.85107093136417,1.38281506835858));
#54854=CARTESIAN_POINT('Ctrl Pts',(-66.7470048295806,0.918549746309561,
3.98737898816158));
#54855=CARTESIAN_POINT('Ctrl Pts',(-66.5481312978832,-2.8579368316873,2.92833090646582));
#54856=CARTESIAN_POINT('Ctrl Pts',(-66.3492577661857,-4.00854518060657,
-0.821273624752269));
#54857=CARTESIAN_POINT('Ctrl Pts',(-66.1503842344883,-1.47609398694865,
-3.81629026324934));
#54858=CARTESIAN_POINT('Ctrl Pts',(-65.9515107027908,2.41259539274093,-3.30489157198884));
#54859=CARTESIAN_POINT('Ctrl Pts',(-65.7526371710934,4.08458717186426,0.243048281458172));
#54860=CARTESIAN_POINT('Ctrl Pts',(-65.5537636393959,2.0036518707079,3.56767487485709));
#54861=CARTESIAN_POINT('Ctrl Pts',(-65.3548901076985,-1.91824288329831,
3.61431446782833));
#54862=CARTESIAN_POINT('Ctrl Pts',(-65.156016576001,-4.07765213745451,0.340114506586169));
#54863=CARTESIAN_POINT('Ctrl Pts',(-64.9571430443035,-2.49050623518628,
-3.24658336165513));
#54864=CARTESIAN_POINT('Ctrl Pts',(-64.7582695126061,1.38492190965922,-3.85031377108719));
#54865=CARTESIAN_POINT('Ctrl Pts',(-64.5593959809086,3.98788096028769,-0.916367981900684));
#54866=CARTESIAN_POINT('Ctrl Pts',(-64.3605224492112,2.92676679639723,2.85953859060943));
#54867=CARTESIAN_POINT('Ctrl Pts',(-64.1616489175137,-0.823466709472965,
4.00809523465541));
#54868=CARTESIAN_POINT('Ctrl Pts',(-63.9627753858163,-3.81709731187778,
1.47400574738807));
#54869=CARTESIAN_POINT('Ctrl Pts',(-63.7639018541188,-3.30357106658815,
-2.414403247115));
#54870=CARTESIAN_POINT('Ctrl Pts',(-63.5650283224214,0.245283057814545,
-4.08445358074088));
#54871=CARTESIAN_POINT('Ctrl Pts',(-63.3661547907239,3.56877060506427,-2.00169957788552));
#54872=CARTESIAN_POINT('Ctrl Pts',(-63.1672812590265,3.61326439272212,1.92022010716586));
#54873=CARTESIAN_POINT('Ctrl Pts',(-62.968407727329,0.337883437330299,4.07783761501798));
#54874=CARTESIAN_POINT('Ctrl Pts',(-62.7695341956316,-3.24794551404742,
2.48872954927952));
#54875=CARTESIAN_POINT('Ctrl Pts',(-62.5706606639341,-3.84955545820096,
-1.3870283363771));
#54876=CARTESIAN_POINT('Ctrl Pts',(-62.3717871322367,-0.914185943172807,
-3.98838173862321));
#54877=CARTESIAN_POINT('Ctrl Pts',(-62.1729136005392,2.8611394935154,-2.92520181018747));
#54878=CARTESIAN_POINT('Ctrl Pts',(-61.9740400688418,4.00764408886245,0.825659547685083));
#54879=CARTESIAN_POINT('Ctrl Pts',(-61.7751665371443,1.47191706657705,3.81790321784053));
#54880=CARTESIAN_POINT('Ctrl Pts',(-61.5762930054469,-2.41621037872631,
3.30224957224815));
#54881=CARTESIAN_POINT('Ctrl Pts',(-61.3774194737494,-4.08431876691742,
-0.24751776074427));
#54882=CARTESIAN_POINT('Ctrl Pts',(-61.1785459420519,-1.99974668584517,
-3.56986526694341));
#54883=CARTESIAN_POINT('Ctrl Pts',(-60.9796724103544,1.92219675620662,-3.61221323596857));
#54884=CARTESIAN_POINT('Ctrl Pts',(-60.780798878657,4.07802187186193,-0.335652266927447));
#54885=CARTESIAN_POINT('Ctrl Pts',(-60.5819253469596,2.48695211836003,3.24930669415222));
#54886=CARTESIAN_POINT('Ctrl Pts',(-60.3830518152621,-1.38913434788157,
3.84879599293248));
#54887=CARTESIAN_POINT('Ctrl Pts',(-60.1841782835647,-3.98888132301813,
0.912003630779297));
#54888=CARTESIAN_POINT('Ctrl Pts',(-59.9853047518673,-2.92363594830518,
-2.86273953992596));
#54889=CARTESIAN_POINT('Ctrl Pts',(-59.7864312201697,0.827852138732109,
-4.00719174336274));
#54890=CARTESIAN_POINT('Ctrl Pts',(-59.5875576884723,3.81870798089624,-1.46982794514092));
#54891=CARTESIAN_POINT('Ctrl Pts',(-59.3886841567749,3.30092708936454,2.41801678703378));
#54892=CARTESIAN_POINT('Ctrl Pts',(-59.1898106250773,-0.249752389578364,
4.0841827304343));
#54893=CARTESIAN_POINT('Ctrl Pts',(-58.99093709338,-3.57095886016693,1.99779319517138));
#54894=CARTESIAN_POINT('Ctrl Pts',(-58.7920635616823,-3.61116099788224,
-1.92417282982888));
#54895=CARTESIAN_POINT('Ctrl Pts',(-58.5931900299852,-0.333420996045656,
-4.07820490793111));
#54896=CARTESIAN_POINT('Ctrl Pts',(-58.3943164982874,3.25066690156188,-2.48517394296011));
#54897=CARTESIAN_POINT('Ctrl Pts',(-58.1954429665903,3.84803537550925,1.39123994354218));
#54898=CARTESIAN_POINT('Ctrl Pts',(-57.9965694348925,0.909821045373206,
3.98937971332309));
#54899=CARTESIAN_POINT('Ctrl Pts',(-57.7976959031954,-2.86433872936233,
2.92206921121879));
#54900=CARTESIAN_POINT('Ctrl Pts',(-57.5988223714976,-4.0067381982916,-0.830044481957909));
#54901=CARTESIAN_POINT('Ctrl Pts',(-57.3999488398004,-1.4677383837049,-3.81951160080411));
#54902=CARTESIAN_POINT('Ctrl Pts',(-57.2010753081027,2.41982247149684,-3.29960361833307));
#54903=CARTESIAN_POINT('Ctrl Pts',(-57.0022017764055,4.08404547133213,0.251986943647925));
#54904=CARTESIAN_POINT('Ctrl Pts',(-56.8033282447079,1.99583910644906,3.57205138440731));
#54905=CARTESIAN_POINT('Ctrl Pts',(-56.6044547130105,-1.92614832744107,
3.61010767877826));
#54906=CARTESIAN_POINT('Ctrl Pts',(-56.4055811813131,-4.07838672317089,
0.33118962535267));
#54907=CARTESIAN_POINT('Ctrl Pts',(-56.2067076496156,-2.48339502361169,
-3.25202613586953));
#54908=CARTESIAN_POINT('Ctrl Pts',(-56.0078341179182,1.39334512272882,-3.84727360615874));
#54909=CARTESIAN_POINT('Ctrl Pts',(-55.8089605862207,3.98987690938877,-0.907638187607902));
#54910=CARTESIAN_POINT('Ctrl Pts',(-55.6100870545232,2.92050159939748,2.86593706134566));
#54911=CARTESIAN_POINT('Ctrl Pts',(-55.4112135228258,-0.832236576706052,
4.00628345378487));
#54912=CARTESIAN_POINT('Ctrl Pts',(-55.2123399911283,-3.82031407732352,
1.46564838289459));
#54913=CARTESIAN_POINT('Ctrl Pts',(-55.0134664594308,-3.29827915955003,
-2.42162743157478));
#54914=CARTESIAN_POINT('Ctrl Pts',(-54.8145929277335,0.254221422284016,
-4.08390698965212));
#54915=CARTESIAN_POINT('Ctrl Pts',(-54.6157193960359,3.57314283933769,-1.99388442026303));
#54916=CARTESIAN_POINT('Ctrl Pts',(-54.4168458643385,3.60905327897176,1.92812324845197));
#54917=CARTESIAN_POINT('Ctrl Pts',(-54.217972332641,0.328958155516463,4.07856731752671));
#54918=CARTESIAN_POINT('Ctrl Pts',(-54.0190988009436,-3.25338439666812,
2.48161536084749));
#54919=CARTESIAN_POINT('Ctrl Pts',(-53.8202252692462,-3.84651068510908,
-1.39544988481116));
#54920=CARTESIAN_POINT('Ctrl Pts',(-53.6213517375487,-0.90545505813692,
-3.99037291106635));
#54921=CARTESIAN_POINT('Ctrl Pts',(-53.4224782058513,2.86753453539748,-2.9189331133105));
#54922=CARTESIAN_POINT('Ctrl Pts',(-53.2236046741537,4.00582750997863,0.834428422320255));
#54923=CARTESIAN_POINT('Ctrl Pts',(-53.0247311424564,1.46355794333582,3.82111541021416));
#54924=CARTESIAN_POINT('Ctrl Pts',(-52.8258576107589,-2.42343166672732,
3.29695371341198));
#54925=CARTESIAN_POINT('Ctrl Pts',(-52.6269840790614,-4.0837672854357,-0.256455824817776));
#54926=CARTESIAN_POINT('Ctrl Pts',(-52.428110547364,-1.99192913719839,-3.57423322463125));
#54927=CARTESIAN_POINT('Ctrl Pts',(-52.2292370156665,1.93009759227027,-3.60799779877848));
#54928=CARTESIAN_POINT('Ctrl Pts',(-52.030363483969,4.07874669094455,-0.326726587205112));
#54929=CARTESIAN_POINT('Ctrl Pts',(-51.8314899522717,2.47983495520026,3.25474168355105));
#54930=CARTESIAN_POINT('Ctrl Pts',(-51.6326164205741,-1.39755422915913,
3.84574661258867));
#54931=CARTESIAN_POINT('Ctrl Pts',(-51.4337428888767,-3.99086771820734,
0.90327165761377));
#54932=CARTESIAN_POINT('Ctrl Pts',(-51.2348693571792,-2.91736375342743,
-2.86913115103951));
#54933=CARTESIAN_POINT('Ctrl Pts',(-51.0359958254819,0.836620018144438,
-4.00537036700946));
#54934=CARTESIAN_POINT('Ctrl Pts',(-50.8371222937842,3.82191559923634,-1.46146706565414));
#54935=CARTESIAN_POINT('Ctrl Pts',(-50.638248762087,3.29562728031547,2.4252351764145));
#54936=CARTESIAN_POINT('Ctrl Pts',(-50.4393752303894,-0.258690150580364,
4.08362635872462));
#54937=CARTESIAN_POINT('Ctrl Pts',(-50.240501698692,-3.57532253996157,1.98997325784056));
#54938=CARTESIAN_POINT('Ctrl Pts',(-50.0416281669945,-3.60694123851437,
-1.93207135830493));
#54939=CARTESIAN_POINT('Ctrl Pts',(-49.842754635297,-0.324494921086645,
-4.07892484337071));
#54940=CARTESIAN_POINT('Ctrl Pts',(-49.6438811035996,3.25609799611201,-2.47805380720297));
#54941=CARTESIAN_POINT('Ctrl Pts',(-49.4450075719021,3.84498138882624,1.39965815514278));
#54942=CARTESIAN_POINT('Ctrl Pts',(-49.2461340402047,0.901087986692135,
3.99136133066359));
#54943=CARTESIAN_POINT('Ctrl Pts',(-49.0472605085072,-2.87072690779386,
2.91579352021808));
#54944=CARTESIAN_POINT('Ctrl Pts',(-48.8483869768098,-4.00491202501419,
-0.838811363522581));
#54945=CARTESIAN_POINT('Ctrl Pts',(-48.6495134451123,-1.45937575047546,
-3.82271464415041));
#54946=CARTESIAN_POINT('Ctrl Pts',(-48.4506399134149,2.42703796009631,-3.2942998606577));
#54947=CARTESIAN_POINT('Ctrl Pts',(-48.2517663817175,4.08348420956112,0.26092439890286));
#54948=CARTESIAN_POINT('Ctrl Pts',(-48.0528928500199,1.98801678277504,3.57641078500256));
#54949=CARTESIAN_POINT('Ctrl Pts',(-47.8540193183226,-1.93404454596509,
3.60588359849573));
#54950=CARTESIAN_POINT('Ctrl Pts',(-47.655145786625,-4.07910177475187,0.32226315782912));
#54951=CARTESIAN_POINT('Ctrl Pts',(-47.4562722549277,-2.47627191738885,
-3.25745333394491));
#54952=CARTESIAN_POINT('Ctrl Pts',(-47.2573987232301,1.40176166213211,-3.84421501405087));
#54953=CARTESIAN_POINT('Ctrl Pts',(-47.0585251915328,3.99185374828742,-0.898904046025764));
#54954=CARTESIAN_POINT('Ctrl Pts',(-46.8596516598352,2.91422241415247,2.8723218051829));
#54955=CARTESIAN_POINT('Ctrl Pts',(-46.6607781281379,-0.84100245779873,
4.00445248412992));
#54956=CARTESIAN_POINT('Ctrl Pts',(-46.4619045964403,-3.82351254471717,
1.45728399842591));
#54957=CARTESIAN_POINT('Ctrl Pts',(-46.2630310647429,-3.29297145483604,
-2.4288400172331));
#54958=CARTESIAN_POINT('Ctrl Pts',(-46.0641575330455,0.263158569116434,
-4.08334083798774));
#54959=CARTESIAN_POINT('Ctrl Pts',(-45.865284001348,3.57749795942844,-1.9860597125875));
#54960=CARTESIAN_POINT('Ctrl Pts',(-45.6664104696506,3.60482487903916,1.93601715466008));
#54961=CARTESIAN_POINT('Ctrl Pts',(-45.467536937953,0.320031298100702,4.079277485035));
#54962=CARTESIAN_POINT('Ctrl Pts',(-45.2686634062557,-3.25880769664411,
2.47448928629133));
#54963=CARTESIAN_POINT('Ctrl Pts',(-45.0697898745582,-3.843447488492,-1.40386474949774));
#54964=CARTESIAN_POINT('Ctrl Pts',(-44.8709163428607,-0.896719836268132,
-3.99234497093138));
#54965=CARTESIAN_POINT('Ctrl Pts',(-44.6720428111633,2.87391584272915,-2.91265043570083));
#54966=CARTESIAN_POINT('Ctrl Pts',(-44.4731692794658,4.0039917444943,0.843193300316898));
#54967=CARTESIAN_POINT('Ctrl Pts',(-44.2742957477683,1.45519181013165,3.82430930069778));
#54968=CARTESIAN_POINT('Ctrl Pts',(-44.0754222160709,-2.43064134728539,
3.29164206324814));
#54969=CARTESIAN_POINT('Ctrl Pts',(-43.8765486843734,-4.0831962440474,-0.265392660552267));
#54970=CARTESIAN_POINT('Ctrl Pts',(-43.677675152676,-1.9841020478638,-3.57858406291378));
#54971=CARTESIAN_POINT('Ctrl Pts',(-43.4788016209785,1.93798918379931,-3.6037650804616));
#54972=CARTESIAN_POINT('Ctrl Pts',(-43.2799280892811,4.07945197416759,-0.31779934256946));
#54973=CARTESIAN_POINT('Ctrl Pts',(-43.0810545575837,2.47270591444402,3.26016108380421));
#54974=CARTESIAN_POINT('Ctrl Pts',(-42.8821810258862,-1.40596741661001,
3.8426788123793));
#54975=CARTESIAN_POINT('Ctrl Pts',(-42.6833074941888,-3.99283499844841,
0.894535358073276));
#54976=CARTESIAN_POINT('Ctrl Pts',(-42.4844339624912,-2.91107758533382,
-2.8755090199554));
#54977=CARTESIAN_POINT('Ctrl Pts',(-42.2855604307939,0.845383890421254,
-4.00352980624524));
#54978=CARTESIAN_POINT('Ctrl Pts',(-42.0866868990963,3.82510491185373,-1.45309918621901));
#54979=CARTESIAN_POINT('Ctrl Pts',(-41.887813367399,3.29031168629198,2.43244194971396));
#54980=CARTESIAN_POINT('Ctrl Pts',(-41.6889398357014,-0.267626672541508,
4.08305042778336));
#54981=CARTESIAN_POINT('Ctrl Pts',(-41.4900663040041,-3.57966909513332,
1.98214378919011));
#54982=CARTESIAN_POINT('Ctrl Pts',(-41.2911927723065,-3.60270420308042,
-1.93996063279246));
#54983=CARTESIAN_POINT('Ctrl Pts',(-41.0923192406092,-0.315567291903492,
-4.07962524209743));
#54984=CARTESIAN_POINT('Ctrl Pts',(-40.8934457089116,3.26151349502002,-2.47092180238066));
#54985=CARTESIAN_POINT('Ctrl Pts',(-40.6945721772142,3.84190898594293,1.40806966283943));
#54986=CARTESIAN_POINT('Ctrl Pts',(-40.4956986455167,0.89235061209512,3.99332383069183));
#54987=CARTESIAN_POINT('Ctrl Pts',(-40.2968251138193,-2.87710133638473,
2.90950386352227));
#54988=CARTESIAN_POINT('Ctrl Pts',(-40.0979515821219,-4.00306666952103,
-0.847574227456036));
#54989=CARTESIAN_POINT('Ctrl Pts',(-39.8990780504243,-1.45100612731439,
-3.82589937794683));
#54990=CARTESIAN_POINT('Ctrl Pts',(-39.700204518727,2.4342418239797,-3.28898032436581));
#54991=CARTESIAN_POINT('Ctrl Pts',(-39.5013309870295,4.08290338923934,0.269860604415452));
#54992=CARTESIAN_POINT('Ctrl Pts',(-39.302457455332,1.98018493715246,3.58075305576247));
#54993=CARTESIAN_POINT('Ctrl Pts',(-39.1035839236346,-1.94193150104956,
3.60164224721296));
#54994=CARTESIAN_POINT('Ctrl Pts',(-38.9047103919371,-4.07979728877255,
0.313335146770926));
#54995=CARTESIAN_POINT('Ctrl Pts',(-38.7058368602396,-2.46913695063545,
-3.2628649298867));
#54996=CARTESIAN_POINT('Ctrl Pts',(-38.5069633285422,1.4101714875567,-3.84113800941335));
#54997=CARTESIAN_POINT('Ctrl Pts',(-38.3080897968447,3.9938114675153,-0.890165598987688));
#54998=CARTESIAN_POINT('Ctrl Pts',(-38.1092162651473,2.9079292707373,2.87869279154047));
#54999=CARTESIAN_POINT('Ctrl Pts',(-37.9103427334498,-0.849764310765561,
4.00260233446029));
#55000=CARTESIAN_POINT('Ctrl Pts',(-37.7114692017524,-3.8266926987392,1.44891263404444));
#55001=CARTESIAN_POINT('Ctrl Pts',(-37.512595670055,-3.28764797786823,-2.43604096954391));
#55002=CARTESIAN_POINT('Ctrl Pts',(-37.3137221383575,0.272094455505398,
-4.08275512845934));
#55003=CARTESIAN_POINT('Ctrl Pts',(-37.1148486066601,3.58183594447665,-1.97822549233722));
#55004=CARTESIAN_POINT('Ctrl Pts',(-36.9159750749626,3.60057921317725,1.94390178798048));
#55005=CARTESIAN_POINT('Ctrl Pts',(-36.7171015432651,0.311102907840033,
4.0799681141415));
#55006=CARTESIAN_POINT('Ctrl Pts',(-36.5182280115677,-3.26421538799967,
2.46735135974267));
#55007=CARTESIAN_POINT('Ctrl Pts',(-36.3193544798702,-3.84036588302135,
-1.4122728901326));
#55008=CARTESIAN_POINT('Ctrl Pts',(-36.1204809481728,-0.887980319405062,
-3.99429790877284));
#55009=CARTESIAN_POINT('Ctrl Pts',(-35.9216074164752,2.88028338494615,-2.90635380745027));
#55010=CARTESIAN_POINT('Ctrl Pts',(-35.7227338847779,4.00213680120204,0.851954139694033));
#55011=CARTESIAN_POINT('Ctrl Pts',(-35.5238603530804,1.44681870703591,3.82748487399346));
#55012=CARTESIAN_POINT('Ctrl Pts',(-35.324986821383,-2.43783938586804,3.28631464719804));
#55013=CARTESIAN_POINT('Ctrl Pts',(-35.1261132896855,-4.08260564548768,
-0.274328225142681));
#55014=CARTESIAN_POINT('Ctrl Pts',(-34.9272397579881,-1.97626545533103,
-3.58291776095168));
#55015=CARTESIAN_POINT('Ctrl Pts',(-34.7283662262906,1.94587149299542,-3.59951510129151));
#55016=CARTESIAN_POINT('Ctrl Pts',(-34.5294926945931,4.08013771815312,-0.308870575779051));
#55017=CARTESIAN_POINT('Ctrl Pts',(-34.3306191628957,2.46556503023685,3.26556486895468));
#55018=CARTESIAN_POINT('Ctrl Pts',(-34.1317456311982,-1.41437386993809,
3.83959260699806));
#55019=CARTESIAN_POINT('Ctrl Pts',(-33.9328720995008,-3.99478315431879,
0.885794774001494));
#55020=CARTESIAN_POINT('Ctrl Pts',(-33.7339985678033,-2.90477747413283,
-2.88187311612569));
#55021=CARTESIAN_POINT('Ctrl Pts',(-33.5351250361059,0.854143713586202,
-4.0016700698857));
#55022=CARTESIAN_POINT('Ctrl Pts',(-33.3362515044084,3.82827590347246,-1.44472434691534));
#55023=CARTESIAN_POINT('Ctrl Pts',(-33.137377972711,3.28498033275429,2.4396370724137));
#55024=CARTESIAN_POINT('Ctrl Pts',(-32.9385044410135,-0.276561912658538,
4.08245494036915));
#55025=CARTESIAN_POINT('Ctrl Pts',(-32.739630909316,-3.58399850486372,1.97430482672065));
#55026=CARTESIAN_POINT('Ctrl Pts',(-32.5407573776186,-3.59844991187427,
-1.94784061550473));
#55027=CARTESIAN_POINT('Ctrl Pts',(-32.3418838459211,-0.306638151256235,
-4.08030610075666));
#55028=CARTESIAN_POINT('Ctrl Pts',(-32.1430103142237,3.26691337234775,-2.46377796265275));
#55029=CARTESIAN_POINT('Ctrl Pts',(-31.9441367825262,3.83881818157496,1.41647442634414));
#55030=CARTESIAN_POINT('Ctrl Pts',(-31.7452632508288,0.883608963431191,
3.99526720400796));
#55031=CARTESIAN_POINT('Ctrl Pts',(-31.5463897191313,-2.88346198460323,
2.90320027125685));
#55032=CARTESIAN_POINT('Ctrl Pts',(-31.3475161874339,-4.00120214065086,
-0.856333031786573));
#55033=CARTESIAN_POINT('Ctrl Pts',(-31.1486426557364,-1.44262955430986,
-3.82906578693936));
#55034=CARTESIAN_POINT('Ctrl Pts',(-30.949769124039,2.44143402864274,-3.2836450349365));
#55035=CARTESIAN_POINT('Ctrl Pts',(-30.7508955923415,4.08230301314886,0.27879551738431));
#55036=CARTESIAN_POINT('Ctrl Pts',(-30.5520220606441,1.97234360709299,3.58507817588923));
#55037=CARTESIAN_POINT('Ctrl Pts',(-30.3531485289466,-1.94980915491895,
3.59738364524442));
#55038=CARTESIAN_POINT('Ctrl Pts',(-30.1542749972491,-4.08047326190165,
0.304405634939932));
#55039=CARTESIAN_POINT('Ctrl Pts',(-29.9554014655517,-2.46199015752543,
-3.26826089777505));
#55040=CARTESIAN_POINT('Ctrl Pts',(-29.7565279338542,1.41857455872196,-3.83804260698401));
#55041=CARTESIAN_POINT('Ctrl Pts',(-29.5576544021568,3.99575005769547,-0.881422888348441));
#55042=CARTESIAN_POINT('Ctrl Pts',(-29.3587808704593,2.90162219929436,2.88504998990312));
#55043=CARTESIAN_POINT('Ctrl Pts',(-29.1599073387619,-0.858522093639685,
4.00073301363767));
#55044=CARTESIAN_POINT('Ctrl Pts',(-28.9610338070644,-3.82985452415772,
1.44053432984656));
#55045=CARTESIAN_POINT('Ctrl Pts',(-28.762160275367,-3.28230875414438,-2.44323025401721));
#55046=CARTESIAN_POINT('Ctrl Pts',(-28.5632867436695,0.281029038651357,
-4.08214986387229));
#55047=CARTESIAN_POINT('Ctrl Pts',(-28.364413211972,3.58615677370501,-1.97038179703515));
#55048=CARTESIAN_POINT('Ctrl Pts',(-28.1655396802746,3.59631630172115,1.9517771106487));
#55049=CARTESIAN_POINT('Ctrl Pts',(-27.9666661485772,0.302173027498423,
4.08063920153816));
#55050=CARTESIAN_POINT('Ctrl Pts',(-27.7677926168797,-3.26960744483348,
2.46020161538995));
#55051=CARTESIAN_POINT('Ctrl Pts',(-27.5689190851823,-3.83726588345715,
-1.42067426644308));
#55052=CARTESIAN_POINT('Ctrl Pts',(-27.3700455534848,-0.879236549407603,
-3.9962317152367));
#55053=CARTESIAN_POINT('Ctrl Pts',(-27.1711720217874,2.88663713154996,-2.90004325871786));
#55054=CARTESIAN_POINT('Ctrl Pts',(-26.9722984900899,4.00026268898655,0.860710898490242));
#55055=CARTESIAN_POINT('Ctrl Pts',(-26.7734249583925,1.43843867415264,3.83064211489142));
#55056=CARTESIAN_POINT('Ctrl Pts',(-26.5745514266949,-2.4450257479994,3.28097149077797));
#55057=CARTESIAN_POINT('Ctrl Pts',(-26.3756778949976,-4.08199549258528,
-0.283262475791065));
#55058=CARTESIAN_POINT('Ctrl Pts',(-26.1768043633001,-1.96841939713446,
-3.58723429798812));
#55059=CARTESIAN_POINT('Ctrl Pts',(-25.9779308316026,1.95374448210496,-3.59524788162401));
#55060=CARTESIAN_POINT('Ctrl Pts',(-25.7790572999052,4.08080391961648,-0.299940329600006));
#55061=CARTESIAN_POINT('Ctrl Pts',(-25.5801837682077,2.45841233678166,3.27095301311981));
#55062=CARTESIAN_POINT('Ctrl Pts',(-25.3813102365102,-1.42277354887878,
3.83648801122703));
#55063=CARTESIAN_POINT('Ctrl Pts',(-25.1824367048128,-3.99671217648749,
0.877049947263231));
#55064=CARTESIAN_POINT('Ctrl Pts',(-24.9835631731153,-2.89846345,-2.88822340906861));
#55065=CARTESIAN_POINT('Ctrl Pts',(-24.7846896414179,0.862899445683009,
-3.99979116683832));
#55066=CARTESIAN_POINT('Ctrl Pts',(-24.5858161097205,3.83142855890469,-1.43634258785545));
#55067=CARTESIAN_POINT('Ctrl Pts',(-24.386942578023,3.27963324523758,2.44682051005175));
#55068=CARTESIAN_POINT('Ctrl Pts',(-24.1880690463255,-0.285495828134668,
4.08183989933402));
#55069=CARTESIAN_POINT('Ctrl Pts',(-23.9891955146281,-3.58831074841608,
1.96645640797843));
#55070=CARTESIAN_POINT('Ctrl Pts',(-23.7903219829306,-3.59417838527282,
-1.95571126869881));
#55071=CARTESIAN_POINT('Ctrl Pts',(-23.5914484512332,-0.297707541912983,
-4.08096741608726));
#55072=CARTESIAN_POINT('Ctrl Pts',(-23.3925749195357,3.27229760223123,-2.45662232223627));
#55073=CARTESIAN_POINT('Ctrl Pts',(-23.1937013878383,3.83570899052647,1.42487240540064));
#55074=CARTESIAN_POINT('Ctrl Pts',(-22.9948278561408,0.874863082569913,
3.99719144130402));
#55075=CARTESIAN_POINT('Ctrl Pts',(-22.7959543244434,-2.88980882198426,
2.8968827736137));
#55076=CARTESIAN_POINT('Ctrl Pts',(-22.5970807927459,-3.99931844733409,
-0.865087734562843));
#55077=CARTESIAN_POINT('Ctrl Pts',(-22.3982072610485,-1.43424607158253,
-3.83221385596205));
#55078=CARTESIAN_POINT('Ctrl Pts',(-22.199333729351,2.44861453963709,-3.27829401792386));
#55079=CARTESIAN_POINT('Ctrl Pts',(-22.0004601976536,4.08168308416519,0.287729095013874));
#55080=CARTESIAN_POINT('Ctrl Pts',(-21.8015866659561,1.96449283015443,3.58938612466668));
#55081=CARTESIAN_POINT('Ctrl Pts',(-21.6027131342586,-1.95767746984148,
3.59310781298765));
#55082=CARTESIAN_POINT('Ctrl Pts',(-21.4038396025612,-4.08112969090158,
0.295474665105836));
#55083=CARTESIAN_POINT('Ctrl Pts',(-21.2049660708637,-2.45483157228964,
-3.27364121176524));
#55084=CARTESIAN_POINT('Ctrl Pts',(-21.0060925391663,1.42697083538037,-3.8349288215887));
#55085=CARTESIAN_POINT('Ctrl Pts',(-20.8072190074688,3.9976695095428,-0.872675955982284));
#55086=CARTESIAN_POINT('Ctrl Pts',(-20.6083454757714,2.89530123003215,2.89139336982226));
#55087=CARTESIAN_POINT('Ctrl Pts',(-20.4094719440739,-0.867275764474581,
3.99884453061537));
#55088=CARTESIAN_POINT('Ctrl Pts',(-20.2105984123765,-3.83299800582851,
1.43214912596145));
#55089=CARTESIAN_POINT('Ctrl Pts',(-20.011724880679,-3.2769538092377,-2.45040783621837));
#55090=CARTESIAN_POINT('Ctrl Pts',(-19.8128513489816,0.289962275760122,
-4.08152504712563));
#55091=CARTESIAN_POINT('Ctrl Pts',(-19.6139778172841,3.59046042641794,-1.96252866425041));
#55092=CARTESIAN_POINT('Ctrl Pts',(-19.4151042855866,3.59203616508904,1.95964308494436));
#55093=CARTESIAN_POINT('Ctrl Pts',(-19.2162307538892,0.293241699846985,
4.08129074401085));
#55094=CARTESIAN_POINT('Ctrl Pts',(-19.0173572221917,-3.27498384131962,
2.45304008747782));
#55095=CARTESIAN_POINT('Ctrl Pts',(-18.8184836904943,-3.83414750464725,
-1.42906883818977));
#55096=CARTESIAN_POINT('Ctrl Pts',(-18.6196101587969,-0.87048856815513,
-3.99814638106069));
#55097=CARTESIAN_POINT('Ctrl Pts',(-18.4207366270994,2.89297705210815,-2.89371881972889));
#55098=CARTESIAN_POINT('Ctrl Pts',(-18.221863095402,3.99836941682417,0.869463534763232));
#55099=CARTESIAN_POINT('Ctrl Pts',(-18.0229895637045,1.43005175161989,3.83378100826934));
#55100=CARTESIAN_POINT('Ctrl Pts',(-17.824116032007,-2.45220039925878,3.27561261958018));
#55101=CARTESIAN_POINT('Ctrl Pts',(-17.6252425003095,-4.08136578826266,
-0.292195369704815));
#55102=CARTESIAN_POINT('Ctrl Pts',(-17.4263689686121,-1.96056391085437,
-3.59153365334828));
#55103=CARTESIAN_POINT('Ctrl Pts',(-17.2274954369147,1.96160811341902,-3.5909634418978));
#55104=CARTESIAN_POINT('Ctrl Pts',(-17.0286219052172,4.08145057536688,-0.291008646804869));
#55105=CARTESIAN_POINT('Ctrl Pts',(-16.8297483735198,2.45124786833711,3.27632549049245));
#55106=CARTESIAN_POINT('Ctrl Pts',(-16.6308748418223,-1.43116641320073,
3.83336503993602));
#55107=CARTESIAN_POINT('Ctrl Pts',(-16.4320013101249,-3.99862205571501,
0.868300919743232));
#55108=CARTESIAN_POINT('Ctrl Pts',(-16.2331277784274,-2.8921355431775,-2.8945598683681));
#55109=CARTESIAN_POINT('Ctrl Pts',(-16.03425424673,0.871651044774114,-3.99789310610252));
#55110=CARTESIAN_POINT('Ctrl Pts',(-15.8353807150324,3.83456286305009,-1.42795394918566));
#55111=CARTESIAN_POINT('Ctrl Pts',(-15.6365071833351,3.27427044935288,2.45399222822166));
#55112=CARTESIAN_POINT('Ctrl Pts',(-15.4376336516376,-0.294428376179469,
4.08120530762398));
#55113=CARTESIAN_POINT('Ctrl Pts',(-15.2387601199401,-3.59260580513641,
1.95859857055446));
#55114=CARTESIAN_POINT('Ctrl Pts',(-15.0398865882427,-3.58988964373505,
-1.96357255467723));
#55115=CARTESIAN_POINT('Ctrl Pts',(-14.8410130565452,-0.288775506647972,
-4.08160918492181));
#55116=CARTESIAN_POINT('Ctrl Pts',(-14.6421395248478,3.27766615888202,-2.44945491540405));
#55117=CARTESIAN_POINT('Ctrl Pts',(-14.4432659931503,3.83258142768927,1.4332635597854));
#55118=CARTESIAN_POINT('Ctrl Pts',(-14.2443924614529,0.866113011401431,
3.99909653336338));
#55119=CARTESIAN_POINT('Ctrl Pts',(-14.0455189297554,-2.89614181812821,
2.89055140085189));
#55120=CARTESIAN_POINT('Ctrl Pts',(-13.846645398058,-3.99741559859308,-0.873838293852223));
#55121=CARTESIAN_POINT('Ctrl Pts',(-13.6477718663605,-1.42585571928681,
-3.83534356993671));
#55122=CARTESIAN_POINT('Ctrl Pts',(-13.448898334663,2.45578332257062,-3.27292729895759));
#55123=CARTESIAN_POINT('Ctrl Pts',(-13.2500248029656,4.08104360525762,0.296661294515633));
#55124=CARTESIAN_POINT('Ctrl Pts',(-13.0511512712681,1.95663264393901,3.59367688146139));
#55125=CARTESIAN_POINT('Ctrl Pts',(-12.8522777395707,-1.96553640813083,
3.58881477092224));
#55126=CARTESIAN_POINT('Ctrl Pts',(-12.6534042078732,-4.0817665726281,0.286542280044954));
#55127=CARTESIAN_POINT('Ctrl Pts',(-12.4545306761758,-2.44766122921548,
-3.27900584608708));
#55128=CARTESIAN_POINT('Ctrl Pts',(-12.2556571444783,1.43536027731604,-3.8317966681416));
#55129=CARTESIAN_POINT('Ctrl Pts',(-12.0567836127809,3.99956981386368,-0.863924843784606));
#55130=CARTESIAN_POINT('Ctrl Pts',(-11.8579100810834,2.88896639322636,2.89772290091486));
#55131=CARTESIAN_POINT('Ctrl Pts',(-11.659036549386,-0.876025281342798,
3.9969368944388));
#55132=CARTESIAN_POINT('Ctrl Pts',(-11.4601630176885,-3.83612312869551,
1.42375706255146));
#55133=CARTESIAN_POINT('Ctrl Pts',(-11.261289485991,-3.27158316879638,-2.45757368176949));
#55134=CARTESIAN_POINT('Ctrl Pts',(-11.0624159542936,0.298894124044868,
-4.08088068121199));
#55135=CARTESIAN_POINT('Ctrl Pts',(-10.8635424225961,3.59474688200251,-1.95466613159658));
#55136=CARTESIAN_POINT('Ctrl Pts',(-10.6646688908987,3.58773882378118,1.96749967319203));
#55137=CARTESIAN_POINT('Ctrl Pts',(-10.4657953592012,0.284308967664094,
4.08192273843878));
#55138=CARTESIAN_POINT('Ctrl Pts',(-10.2669218275038,-3.28034455170665,
2.44586681030803));
#55139=CARTESIAN_POINT('Ctrl Pts',(-10.0680482958063,-3.83101076152782,
-1.43745656516507));
#55140=CARTESIAN_POINT('Ctrl Pts',(-9.86917476410886,-0.861736417547805,
-4.00004189707429));
#55141=CARTESIAN_POINT('Ctrl Pts',(-9.67030123241143,2.89930311625488,-2.88738052077529));
#55142=CARTESIAN_POINT('Ctrl Pts',(-9.47142770071396,3.99645699378297,0.878212006591244));
#55143=CARTESIAN_POINT('Ctrl Pts',(-9.27255416901651,1.42165797960771,3.83690153909317));
#55144=CARTESIAN_POINT('Ctrl Pts',(-9.07368063731905,-2.45936330528239,
3.27023805927156));
#55145=CARTESIAN_POINT('Ctrl Pts',(-8.8748071056216,-4.0807165355358,-0.301126864098756));
#55146=CARTESIAN_POINT('Ctrl Pts',(-8.67593357392414,-1.95269903411579,
-3.59581580643962));
#55147=CARTESIAN_POINT('Ctrl Pts',(-8.4770600422267,1.9694623492732,-3.58666180263391));
#55148=CARTESIAN_POINT('Ctrl Pts',(-8.27818651052923,4.08207768230702,-0.282075570173808));
#55149=CARTESIAN_POINT('Ctrl Pts',(-8.07931297883178,2.44407165921894,3.28168227533997));
#55150=CARTESIAN_POINT('Ctrl Pts',(-7.88043944713432,-1.43955242270476,
3.83022370808317));
#55151=CARTESIAN_POINT('Ctrl Pts',(-7.68156591543689,-4.00051278285394,
0.859547733346342));
#55152=CARTESIAN_POINT('Ctrl Pts',(-7.48269238373941,-2.88579378397343,
-2.90088246367505));
#55153=CARTESIAN_POINT('Ctrl Pts',(-7.28381885204198,0.880398468942455,
-3.99597589676918));
#55154=CARTESIAN_POINT('Ctrl Pts',(-7.0849453203445,3.83767880089717,-1.4195584710844));
#55155=CARTESIAN_POINT('Ctrl Pts',(-6.88607178864706,3.26889197078478,2.46115219257381));
#55156=CARTESIAN_POINT('Ctrl Pts',(-6.68719825694958,-0.303359514006894,
4.0805511682777));
#55157=CARTESIAN_POINT('Ctrl Pts',(-6.48832472525215,-3.59688365445685,
1.95073135208659));
#55158=CARTESIAN_POINT('Ctrl Pts',(-6.28945119355468,-3.58558370779488,
-1.97142443578932));
#55159=CARTESIAN_POINT('Ctrl Pts',(-6.09057766185723,-0.279842088257574,
-4.08223140418192));
#55160=CARTESIAN_POINT('Ctrl Pts',(-5.89170413015981,3.28301901661428,-2.44227577649414));
#55161=CARTESIAN_POINT('Ctrl Pts',(-5.69283059846233,3.82943550799096,1.44164784932378));
#55162=CARTESIAN_POINT('Ctrl Pts',(-5.49395706676489,0.857358791934341,
4.00098247103127));
#55163=CARTESIAN_POINT('Ctrl Pts',(-5.29508353506742,-2.90246094288968,
2.88420618335313));
#55164=CARTESIAN_POINT('Ctrl Pts',(-5.09621000336997,-3.99549360318837,
-0.882584667850434));
#55165=CARTESIAN_POINT('Ctrl Pts',(-4.89733647167251,-1.41745853827654,
-3.83845491367013));
#55166=CARTESIAN_POINT('Ctrl Pts',(-4.69846293997506,2.46294034436706,-3.26754490412554));
#55167=CARTESIAN_POINT('Ctrl Pts',(-4.49958940827759,4.0803845771102,0.305592073830688));
#55168=CARTESIAN_POINT('Ctrl Pts',(-4.30071587658015,1.94876309058629,3.59795042435585));
#55169=CARTESIAN_POINT('Ctrl Pts',(-4.10184234488271,-1.97338594062652,
3.58450454219004));
#55170=CARTESIAN_POINT('Ctrl Pts',(-3.90296881318525,-4.08238388801658,
0.277608517669592));
#55171=CARTESIAN_POINT('Ctrl Pts',(-3.70409528148781,-2.44047919288451,
-3.28435476584923));
#55172=CARTESIAN_POINT('Ctrl Pts',(-3.50522174979033,1.44374290144303,-3.82864617900992));
#55173=CARTESIAN_POINT('Ctrl Pts',(-3.3063482180929,4.00145085374723,-0.855169560880336));
#55174=CARTESIAN_POINT('Ctrl Pts',(-3.10747468639542,2.88261792278395,2.90403849095175));
#55175=CARTESIAN_POINT('Ctrl Pts',(-2.90860115469799,-0.884770986710579,
3.99501023114948));
#55176=CARTESIAN_POINT('Ctrl Pts',(-2.70972762300051,-3.8392291520155,1.41535795907167));
#55177=CARTESIAN_POINT('Ctrl Pts',(-2.51085409130307,-3.26619822895463,
-2.4647273395464));
#55178=CARTESIAN_POINT('Ctrl Pts',(-2.31198055960563,0.307827128338472,
-4.08021755622459));
#55179=CARTESIAN_POINT('Ctrl Pts',(-2.11310702790817,3.59901123398703,-1.94679275070356));
#55180=CARTESIAN_POINT('Ctrl Pts',(-1.91423349621072,3.58343352403109,1.97534403183598));
#55181=CARTESIAN_POINT('Ctrl Pts',(-1.71535996451326,0.275357453827102,
4.08254047995398));
#55182=CARTESIAN_POINT('Ctrl Pts',(-1.51648643281581,-3.28565665797204,
2.43867181422721));
#55183=CARTESIAN_POINT('Ctrl Pts',(-1.31761290111835,-3.82791777672393,
-1.44581851751593));
#55184=CARTESIAN_POINT('Ctrl Pts',(-1.11873936942089,-0.852862866404934,
-4.00195392234629));
#55185=CARTESIAN_POINT('Ctrl Pts',(-0.919865837723433,2.90539384744835,
-2.88096103865537));
#55186=CARTESIAN_POINT('Ctrl Pts',(-0.720992306025977,3.99494365268282,
0.886829055253763));
#55187=CARTESIAN_POINT('Ctrl Pts',(-0.522118774328538,1.41246698653237,
3.84024422739266));
#55188=CARTESIAN_POINT('Ctrl Pts',(-0.323245242631086,-2.46501608324706,
3.26439100997213));
#55189=CARTESIAN_POINT('Ctrl Pts',(-0.124371710933631,-4.08292506541557,
-0.309172729297909));
#55190=CARTESIAN_POINT('Ctrl Pts',(0.074501820763823,-1.93900000174599,
-3.60192375349645));
#55191=CARTESIAN_POINT('Ctrl Pts',(0.207084175228793,0.662521205821,-3.58581394706895));
#55192=CARTESIAN_POINT('Ctrl Pts',(0.273375352461282,1.6717518345084,-3.02875982108483));
#55193=CARTESIAN_POINT('Ctrl Pts',(-109.567,1.87158653173818,-2.62360084935118));
#55194=CARTESIAN_POINT('Ctrl Pts',(-109.500708822768,2.74581178927839,-1.99995864473678));
#55195=CARTESIAN_POINT('Ctrl Pts',(-109.368126468303,3.80651295487345,0.179129781420444));
#55196=CARTESIAN_POINT('Ctrl Pts',(-109.169252936605,1.9032035356359,3.30567173395145));
#55197=CARTESIAN_POINT('Ctrl Pts',(-108.970379404908,-1.7502378889635,3.3848793341849));
#55198=CARTESIAN_POINT('Ctrl Pts',(-108.77150587321,-3.79478855817402,0.359146699884545));
#55199=CARTESIAN_POINT('Ctrl Pts',(-108.572632341513,-2.35308601341721,
-2.99923852306436));
#55200=CARTESIAN_POINT('Ctrl Pts',(-108.373758809815,1.25085188316156,-3.60050797555933));
#55201=CARTESIAN_POINT('Ctrl Pts',(-108.174885278118,3.70539059895966,-0.894369208581839));
#55202=CARTESIAN_POINT('Ctrl Pts',(-107.97601174642,2.7554691459713,2.63391280124896));
#55203=CARTESIAN_POINT('Ctrl Pts',(-107.777138214723,-0.726214962520435,
3.74194114611939));
#55204=CARTESIAN_POINT('Ctrl Pts',(-107.578264683026,-3.5406343533814,1.41197706181962));
#55205=CARTESIAN_POINT('Ctrl Pts',(-107.379391151328,-3.10192059080864,
-2.21537311500977));
#55206=CARTESIAN_POINT('Ctrl Pts',(-107.180517619631,0.186848925119125,
-3.80720285370364));
#55207=CARTESIAN_POINT('Ctrl Pts',(-106.981644087933,3.3039387517963,-1.90098324867159));
#55208=CARTESIAN_POINT('Ctrl Pts',(-106.782770556236,3.3853642004366,1.75187238336515));
#55209=CARTESIAN_POINT('Ctrl Pts',(-106.583897024538,0.356309365737235,
3.79509945705497));
#55210=CARTESIAN_POINT('Ctrl Pts',(-106.385023492841,-3.00012287248227,
2.35138380158418));
#55211=CARTESIAN_POINT('Ctrl Pts',(-106.186149961143,-3.60003625310656,
-1.25278941335415));
#55212=CARTESIAN_POINT('Ctrl Pts',(-105.987276429446,-0.89222882781209,
-3.70589645739097));
#55213=CARTESIAN_POINT('Ctrl Pts',(-105.788402897748,2.63536022101092,-2.75401859025452));
#55214=CARTESIAN_POINT('Ctrl Pts',(-105.589529366051,3.74157491702501,0.728257404654141));
#55215=CARTESIAN_POINT('Ctrl Pts',(-105.390655834353,1.41002288124958,3.54140889901514));
#55216=CARTESIAN_POINT('Ctrl Pts',(-105.191782302656,-2.21706106474189,
3.10070667941842));
#55217=CARTESIAN_POINT('Ctrl Pts',(-104.992908770959,-3.80710475658041,
-0.188931232388143));
#55218=CARTESIAN_POINT('Ctrl Pts',(-104.794035239261,-1.89917277873868,
-3.30497872482143));
#55219=CARTESIAN_POINT('Ctrl Pts',(-104.595161707564,1.75372304650391,-3.38440498687836));
#55220=CARTESIAN_POINT('Ctrl Pts',(-104.396288175866,3.79529453639531,-0.354232993642497));
#55221=CARTESIAN_POINT('Ctrl Pts',(-104.197414644169,2.34974161312935,3.00140899924184));
#55222=CARTESIAN_POINT('Ctrl Pts',(-103.998541112471,-1.25475872875807,
3.59935024210211));
#55223=CARTESIAN_POINT('Ctrl Pts',(-103.799667580774,-3.70638417439717,
0.890201091441595));
#55224=CARTESIAN_POINT('Ctrl Pts',(-103.600794049076,-2.75257623033224,
-2.63686664952715));
#55225=CARTESIAN_POINT('Ctrl Pts',(-103.401920517379,0.730304405924223,
-3.74117589888118));
#55226=CARTESIAN_POINT('Ctrl Pts',(-103.203046985682,3.5421798545178,-1.40808505059571));
#55227=CARTESIAN_POINT('Ctrl Pts',(-103.004173453984,3.09949317971213,2.2187572333099));
#55228=CARTESIAN_POINT('Ctrl Pts',(-102.805299922287,-0.191014192713332,
3.80700081556329));
#55229=CARTESIAN_POINT('Ctrl Pts',(-102.606426390589,-3.30601733267171,
1.8973642316529));
#55230=CARTESIAN_POINT('Ctrl Pts',(-102.407552858892,-3.38344495921552,
-1.75557450409872));
#55231=CARTESIAN_POINT('Ctrl Pts',(-102.208679327194,-0.352156410097993,
-3.79548778081539));
#55232=CARTESIAN_POINT('Ctrl Pts',(-102.009805795497,3.00269417169098,-2.34809909134587));
#55233=CARTESIAN_POINT('Ctrl Pts',(-101.810932263799,3.59866318318054,1.25672786453859));
#55234=CARTESIAN_POINT('Ctrl Pts',(-101.612058732102,0.888173072927529,
3.70687067808071));
#55235=CARTESIAN_POINT('Ctrl Pts',(-101.413185200404,-2.63837228039274,
2.75113310138612));
#55236=CARTESIAN_POINT('Ctrl Pts',(-101.214311668707,-3.74077576519073,
-0.732351217687996));
#55237=CARTESIAN_POINT('Ctrl Pts',(-101.015438137009,-1.40614679609923,
-3.54294973423381));
#55238=CARTESIAN_POINT('Ctrl Pts',(-100.816564605312,2.22045273645088,-3.09827876032406));
#55239=CARTESIAN_POINT('Ctrl Pts',(-100.617691073615,3.80689573555524,0.193097100182191));
#55240=CARTESIAN_POINT('Ctrl Pts',(-100.418817541917,1.89555511623687,3.30705494856008));
#55241=CARTESIAN_POINT('Ctrl Pts',(-100.21994401022,-1.75742543597124,3.38248391991576));
#55242=CARTESIAN_POINT('Ctrl Pts',(-100.021070478522,-3.79567988913556,
0.35007972049143));
#55243=CARTESIAN_POINT('Ctrl Pts',(-99.8221969468248,-2.34645586659674,
-3.00397844492953));
#55244=CARTESIAN_POINT('Ctrl Pts',(-99.6233234151273,1.25869662408462,-3.5979750471627));
#55245=CARTESIAN_POINT('Ctrl Pts',(-99.4244498834298,3.70735607210978,-0.886144788439325));
#55246=CARTESIAN_POINT('Ctrl Pts',(-99.2255763517325,2.74968914886796,2.63987712139888));
#55247=CARTESIAN_POINT('Ctrl Pts',(-99.0267028200349,-0.734397810215034,
3.74037451170853));
#55248=CARTESIAN_POINT('Ctrl Pts',(-98.8278292883376,-3.54371855335358,
1.40420812065201));
#55249=CARTESIAN_POINT('Ctrl Pts',(-98.6289557566399,-3.09706341345078,
-2.22214757488159));
#55250=CARTESIAN_POINT('Ctrl Pts',(-98.4300822249426,0.195179949845956,
-3.80678951593933));
#55251=CARTESIAN_POINT('Ctrl Pts',(-98.2312086932451,3.30809157446657,-1.89374543337553));
#55252=CARTESIAN_POINT('Ctrl Pts',(-98.0323351615477,3.38152186805364,1.75927584174923));
#55253=CARTESIAN_POINT('Ctrl Pts',(-97.8334616298501,0.348002926086945,
3.795870861202));
#55254=CARTESIAN_POINT('Ctrl Pts',(-97.6345880981528,-3.00526181891328,
2.34481193942487));
#55255=CARTESIAN_POINT('Ctrl Pts',(-97.4357145664553,-3.59728583407436,
-1.26066500683384));
#55256=CARTESIAN_POINT('Ctrl Pts',(-97.236841034758,-0.884116238679596,
-3.70784035632476));
#55257=CARTESIAN_POINT('Ctrl Pts',(-97.0379675030604,2.6413811721456,-2.74824437321759));
#55258=CARTESIAN_POINT('Ctrl Pts',(-96.8390939713629,3.73997213852792,0.736444182896666));
#55259=CARTESIAN_POINT('Ctrl Pts',(-96.6402204396655,1.4022690248486,3.54448631164484));
#55260=CARTESIAN_POINT('Ctrl Pts',(-96.4413469079681,-2.22384174810214,
3.09584713945722));
#55261=CARTESIAN_POINT('Ctrl Pts',(-96.2424733762705,-3.80668215674337,
-0.197262741081687));
#55262=CARTESIAN_POINT('Ctrl Pts',(-96.0435998445732,-1.89193518361277,
-3.30912721008056));
#55263=CARTESIAN_POINT('Ctrl Pts',(-95.8447263128756,1.76112572087986,-3.38055880391732));
#55264=CARTESIAN_POINT('Ctrl Pts',(-95.6458527811783,3.79606069695695,-0.345926027506187));
#55265=CARTESIAN_POINT('Ctrl Pts',(-95.4469792494807,2.3431673103227,3.00654429325805));
#55266=CARTESIAN_POINT('Ctrl Pts',(-95.2481057177834,-1.26263301219719,
3.59659554412187));
#55267=CARTESIAN_POINT('Ctrl Pts',(-95.0492321860857,-3.70832353058058,
0.882087424255571));
#55268=CARTESIAN_POINT('Ctrl Pts',(-94.8503586543885,-2.74679877486757,
-2.64288443218266));
#55269=CARTESIAN_POINT('Ctrl Pts',(-94.6514851226908,0.738490335120334,
-3.73956864576937));
#55270=CARTESIAN_POINT('Ctrl Pts',(-94.4526115909935,3.54525300887773,-1.40032950926946));
#55271=CARTESIAN_POINT('Ctrl Pts',(-94.2537380592961,3.09462993870752,2.22553525560538));
#55272=CARTESIAN_POINT('Ctrl Pts',(-94.0548645275986,-0.199345473265892,
3.80657365799952));
#55273=CARTESIAN_POINT('Ctrl Pts',(-93.8559909959012,-3.31016185509202,
1.89012436749044));
#55274=CARTESIAN_POINT('Ctrl Pts',(-93.6571174642037,-3.37959472779509,
-1.76297507280934));
#55275=CARTESIAN_POINT('Ctrl Pts',(-93.4582439325062,-0.343849025370891,
-3.79624939634358));
#55276=CARTESIAN_POINT('Ctrl Pts',(-93.2593704008088,3.00782586757985,-2.34152197978259));
#55277=CARTESIAN_POINT('Ctrl Pts',(-93.0604968691114,3.59590417751189,1.26460063958548));
#55278=CARTESIAN_POINT('Ctrl Pts',(-92.8616233374138,0.880058345774601,
3.70880559473261));
#55279=CARTESIAN_POINT('Ctrl Pts',(-92.6627498057164,-2.64438690106003,
2.74535235425065));
#55280=CARTESIAN_POINT('Ctrl Pts',(-92.4638762740191,-3.73916403355365,
-0.74053626627348));
#55281=CARTESIAN_POINT('Ctrl Pts',(-92.2650027423214,-1.39838957449524,
-3.54601864482274));
#55282=CARTESIAN_POINT('Ctrl Pts',(-92.0661292106243,2.22722809688435,-3.09341181156606));
#55283=CARTESIAN_POINT('Ctrl Pts',(-91.8672556789264,3.80646401974024,0.201428145775125));
#55284=CARTESIAN_POINT('Ctrl Pts',(-91.6683821472293,1.88831298555067,3.31119550919123));
#55285=CARTESIAN_POINT('Ctrl Pts',(-91.4695086155316,-1.7648238969841,3.37862963997555));
#55286=CARTESIAN_POINT('Ctrl Pts',(-91.2706350838343,-3.79643695930539,
0.341771920302796));
#55287=CARTESIAN_POINT('Ctrl Pts',(-91.0717615521368,-2.33987594829705,
-3.00910654149507));
#55288=CARTESIAN_POINT('Ctrl Pts',(-90.8728880204393,1.26656788840972,-3.59521173445138));
#55289=CARTESIAN_POINT('Ctrl Pts',(-90.6740144887419,3.70928654863654,-0.878029003844108));
#55290=CARTESIAN_POINT('Ctrl Pts',(-90.4751409570445,2.74390511179979,2.64588857832797));
#55291=CARTESIAN_POINT('Ctrl Pts',(-90.276267425347,-0.742581975743678,
3.73875830200189));
#55292=CARTESIAN_POINT('Ctrl Pts',(-90.0773938936495,-3.54678321925067,
1.39644922110663));
#55293=CARTESIAN_POINT('Ctrl Pts',(-89.8785203619521,-3.09219275839747,
-2.22892027143228));
#55294=CARTESIAN_POINT('Ctrl Pts',(-89.6796468302546,0.203510757985896,
-3.80635324199837));
#55295=CARTESIAN_POINT('Ctrl Pts',(-89.4807732985572,3.31222817206875,-1.88650103833566));
#55296=CARTESIAN_POINT('Ctrl Pts',(-89.2818997668597,3.37766354074761,1.76667219285066));
#55297=CARTESIAN_POINT('Ctrl Pts',(-89.0830262351624,0.339694712923688,
3.79662338578627));
#55298=CARTESIAN_POINT('Ctrl Pts',(-88.8841527034647,-3.01038631462036,
2.33822921635881));
#55299=CARTESIAN_POINT('Ctrl Pts',(-88.6852791717675,-3.59451821514758,
-1.26853475808103));
#55300=CARTESIAN_POINT('Ctrl Pts',(-88.4864056400698,-0.875999399071568,
-3.70976639214839));
#55301=CARTESIAN_POINT('Ctrl Pts',(-88.2875321083726,2.64738946353692,-2.74245704794827));
#55302=CARTESIAN_POINT('Ctrl Pts',(-88.0886585766749,3.73835145123555,0.744627462918542));
#55303=CARTESIAN_POINT('Ctrl Pts',(-87.8897850449776,1.39450844968449,3.54754673193265));
#55304=CARTESIAN_POINT('Ctrl Pts',(-87.69091151328,-2.23061177874262,3.09097277956667));
#55305=CARTESIAN_POINT('Ctrl Pts',(-87.4920379815828,-3.80624132480706,
-0.205593309274777));
#55306=CARTESIAN_POINT('Ctrl Pts',(-87.2931644498851,-1.88468852638785,
-3.31325984341546));
#55307=CARTESIAN_POINT('Ctrl Pts',(-87.0942909181878,1.76851995985574,-3.37669643040047));
#55308=CARTESIAN_POINT('Ctrl Pts',(-86.8954173864903,3.79680867573037,-0.337617403855405));
#55309=CARTESIAN_POINT('Ctrl Pts',(-86.6965438547928,2.33658178446086,3.01166518657256));
#55310=CARTESIAN_POINT('Ctrl Pts',(-86.4976703230953,-1.27050124801057,
3.59382361980817));
#55311=CARTESIAN_POINT('Ctrl Pts',(-86.298796791398,-3.71024512512451,0.873969532064579));
#55312=CARTESIAN_POINT('Ctrl Pts',(-86.0999232597003,-2.74100816312956,
-2.64888955623758));
#55313=CARTESIAN_POINT('Ctrl Pts',(-85.9010497280032,0.746672727185684,
-3.73794348137644));
#55314=CARTESIAN_POINT('Ctrl Pts',(-85.7021761963054,3.54830918264012,-1.3925672608098));
#55315=CARTESIAN_POINT('Ctrl Pts',(-85.5033026646083,3.08975187543889,2.23230261830901));
#55316=CARTESIAN_POINT('Ctrl Pts',(-85.3044291329105,-0.20767579901831,
3.80612826819978));
#55317=CARTESIAN_POINT('Ctrl Pts',(-85.1055556012133,-3.31429052292249,
1.88287545024988));
#55318=CARTESIAN_POINT('Ctrl Pts',(-84.9066820695157,-3.37572830922368,
-1.77036719744615));
#55319=CARTESIAN_POINT('Ctrl Pts',(-84.7078085378184,-0.335539993719798,
-3.79699282908225));
#55320=CARTESIAN_POINT('Ctrl Pts',(-84.5089350061207,3.01294315696887,-2.33493365309634));
#55321=CARTESIAN_POINT('Ctrl Pts',(-84.3100614744234,3.59312794864103,1.27246735760964));
#55322=CARTESIAN_POINT('Ctrl Pts',(-84.1111879427259,0.871939403430806,
3.71072274742162));
#55323=CARTESIAN_POINT('Ctrl Pts',(-83.9123144110285,-2.65038885598094,
2.73955845777738));
#55324=CARTESIAN_POINT('Ctrl Pts',(-83.7134408793309,-3.73753439254664,
-0.748717767932958));
#55325=CARTESIAN_POINT('Ctrl Pts',(-83.5145673476336,-1.39062565506363,
-3.54907057114484));
#55326=CARTESIAN_POINT('Ctrl Pts',(-83.3156938159361,2.23399278962533,-3.08853004637957));
#55327=CARTESIAN_POINT('Ctrl Pts',(-83.1168202842386,3.80601407221043,0.209758226593208));
#55328=CARTESIAN_POINT('Ctrl Pts',(-82.9179467525413,1.88106181046435,3.31532021028137));
#55329=CARTESIAN_POINT('Ctrl Pts',(-82.7190732208437,-1.77221390506902,
3.37475917750697));
#55330=CARTESIAN_POINT('Ctrl Pts',(-82.5201996891463,-3.79717584578678,
0.333462483138709));
#55331=CARTESIAN_POINT('Ctrl Pts',(-82.3213261574489,-2.33328482275862,
-3.01422022542674));
#55332=CARTESIAN_POINT('Ctrl Pts',(-82.1224526257514,1.27443308628981,-3.59243120185442));
#55333=CARTESIAN_POINT('Ctrl Pts',(-81.9235790940539,3.71119925889672,-0.86990901377786));
#55334=CARTESIAN_POINT('Ctrl Pts',(-81.7247055623564,2.73810793232568,2.65188736231815));
#55335=CARTESIAN_POINT('Ctrl Pts',(-81.525832030659,-0.750762584548115,
3.73712418486865));
#55336=CARTESIAN_POINT('Ctrl Pts',(-81.3269584989616,-3.54983089721885,
1.38868363302726));
#55337=CARTESIAN_POINT('Ctrl Pts',(-81.128084967264,-3.08730729275454,-2.23568229218554));
#55338=CARTESIAN_POINT('Ctrl Pts',(-80.9292114355667,0.211840591375986,
-3.8058987368732));
#55339=CARTESIAN_POINT('Ctrl Pts',(-80.7303379038692,3.31634890518381,-1.87924760757427));
#55340=CARTESIAN_POINT('Ctrl Pts',(-80.5314643721718,3.3737890355405,1.77406008217146));
#55341=CARTESIAN_POINT('Ctrl Pts',(-80.3325908404742,0.331384872734104,
3.79735772578913));
#55342=CARTESIAN_POINT('Ctrl Pts',(-80.1337173087769,-3.01549639156382,
2.33163529394134));
#55343=CARTESIAN_POINT('Ctrl Pts',(-79.9348437770794,-3.59173337965695,
-1.27639843346252));
#55344=CARTESIAN_POINT('Ctrl Pts',(-79.7359702453819,-0.867878363713628,
-3.71167465940716));
#55345=CARTESIAN_POINT('Ctrl Pts',(-79.5370967136845,2.65338507480061,-2.73665658720871));
#55346=CARTESIAN_POINT('Ctrl Pts',(-79.338223181987,3.73671285846524,0.752807176418981));
#55347=CARTESIAN_POINT('Ctrl Pts',(-79.1393496502896,1.38674119528204,3.55059016063458));
#55348=CARTESIAN_POINT('Ctrl Pts',(-78.9404761185921,-2.23737112548394,
3.0860836149298));
#55349=CARTESIAN_POINT('Ctrl Pts',(-78.7416025868947,-3.80578226222256,
-0.21392289274333));
#55350=CARTESIAN_POINT('Ctrl Pts',(-78.5427290551972,-1.87743284212275,
-3.31737660732185));
#55351=CARTESIAN_POINT('Ctrl Pts',(-78.3438555234997,1.77590572820074,-3.3728178836147));
#55352=CARTESIAN_POINT('Ctrl Pts',(-78.1449819918024,3.79753846903493,-0.329307163127962));
#55353=CARTESIAN_POINT('Ctrl Pts',(-77.9461084601048,2.32998506713825,3.01677165499815));
#55354=CARTESIAN_POINT('Ctrl Pts',(-77.7472349284074,-1.27836339853949,
3.59103448225746));
#55355=CARTESIAN_POINT('Ctrl Pts',(-77.5483613967099,-3.71214894881061,
0.865847453846025));
#55356=CARTESIAN_POINT('Ctrl Pts',(-77.3494878650125,-2.73520442286098,
-2.65488199297993));
#55357=CARTESIAN_POINT('Ctrl Pts',(-77.150614333315,0.754851542933501,-3.73630041345961));
#55358=CARTESIAN_POINT('Ctrl Pts',(-76.9517408016175,3.55134836116475,-1.38479834240944));
#55359=CARTESIAN_POINT('Ctrl Pts',(-76.7528672699202,3.08485901327164,2.23905928901498));
#55360=CARTESIAN_POINT('Ctrl Pts',(-76.5539937382226,-0.216005130071836,
3.80566464829338));
#55361=CARTESIAN_POINT('Ctrl Pts',(-76.3551202065253,-3.31840331638788,
1.87561751465306));
#55362=CARTESIAN_POINT('Ctrl Pts',(-76.1562466748277,-3.37184572202029,
-1.77775084260449));
#55363=CARTESIAN_POINT('Ctrl Pts',(-75.9573731431304,-0.327229354942119,
-3.79771807547001));
#55364=CARTESIAN_POINT('Ctrl Pts',(-75.7584996114328,3.01804601534794,-2.32833414284333));
#55365=CARTESIAN_POINT('Ctrl Pts',(-75.5596260797355,3.59033450986518,1.28032798093242));
#55366=CARTESIAN_POINT('Ctrl Pts',(-75.3607525480379,0.863816284783001,
3.71262212696513));
#55367=CARTESIAN_POINT('Ctrl Pts',(-75.1618790163406,-2.6563781164081,2.73375143971716));
#55368=CARTESIAN_POINT('Ctrl Pts',(-74.9630054846429,-3.73588684997514,
-0.756895683479796));
#55369=CARTESIAN_POINT('Ctrl Pts',(-74.7641319529457,-1.38285507499101,
-3.55210549858237));
#55370=CARTESIAN_POINT('Ctrl Pts',(-74.5652584212481,2.24074678227322,-3.08363348814666));
#55371=CARTESIAN_POINT('Ctrl Pts',(-74.3663848895507,3.80554589512093,0.218087302738192));
#55372=CARTESIAN_POINT('Ctrl Pts',(-74.1675113578533,1.87380162570858,3.31942903207455));
#55373=CARTESIAN_POINT('Ctrl Pts',(-73.9686378261556,-1.77959542483032,
3.37087255104825));
#55374=CARTESIAN_POINT('Ctrl Pts',(-73.7697642944585,-3.79789654504064,
0.325151448798652));
#55375=CARTESIAN_POINT('Ctrl Pts',(-73.5708907627607,-2.32668252155082,
-3.01931947223166));
#55376=CARTESIAN_POINT('Ctrl Pts',(-73.3720172310635,1.28229218005324,-3.5896334626897));
#55377=CARTESIAN_POINT('Ctrl Pts',(-73.1731436993659,3.71309419372906,-0.861784857132571));
#55378=CARTESIAN_POINT('Ctrl Pts',(-72.9742701676686,2.73229763821218,2.65787344463722));
#55379=CARTESIAN_POINT('Ctrl Pts',(-72.7753966359709,-0.758939597445834,
3.73547216813566));
#55380=CARTESIAN_POINT('Ctrl Pts',(-72.5765231042737,-3.55286157266074,
1.38091139360858));
#55381=CARTESIAN_POINT('Ctrl Pts',(-72.3776495725761,-3.08240703992181,
-2.24243360475354));
#55382=CARTESIAN_POINT('Ctrl Pts',(-72.1787760408787,0.220169410119124,
-3.80542600274073));
#55383=CARTESIAN_POINT('Ctrl Pts',(-71.9799025091812,3.3204537540748,-1.87198517583289));
#55384=CARTESIAN_POINT('Ctrl Pts',(-71.7810289774838,3.36989837098991,1.78143947432599));
#55385=CARTESIAN_POINT('Ctrl Pts',(-71.5821554457863,0.323073445319674,
3.79807387769336));
#55386=CARTESIAN_POINT('Ctrl Pts',(-71.3832819140889,-3.02059202526815,
2.32503020375521));
#55387=CARTESIAN_POINT('Ctrl Pts',(-71.1844083823913,-3.58893134094086,
-1.28425599531399));
#55388=CARTESIAN_POINT('Ctrl Pts',(-70.9855348506941,-0.859753171502819,
-3.71356514896109));
#55389=CARTESIAN_POINT('Ctrl Pts',(-70.7866613189964,2.65936797721959,-2.73084301878126));
#55390=CARTESIAN_POINT('Ctrl Pts',(-70.5877877872991,3.73505636806534,0.760983284219782));
#55391=CARTESIAN_POINT('Ctrl Pts',(-70.3889142556016,1.37896729884392,3.55361658317363));
#55392=CARTESIAN_POINT('Ctrl Pts',(-70.1900407239041,-2.24411975595105,
3.0811796689641));
#55393=CARTESIAN_POINT('Ctrl Pts',(-69.9911671922068,-3.80530497118865,
-0.222251451591354));
#55394=CARTESIAN_POINT('Ctrl Pts',(-69.7922936605092,-1.8701681655698,-3.32147748208183));
#55395=CARTESIAN_POINT('Ctrl Pts',(-69.5934201288118,1.78328299053953,-3.36892318213695));
#55396=CARTESIAN_POINT('Ctrl Pts',(-69.3945465971144,3.79825007337514,-0.320995345127123));
#55397=CARTESIAN_POINT('Ctrl Pts',(-69.1956730654169,2.32337718995098,3.02186367407648));
#55398=CARTESIAN_POINT('Ctrl Pts',(-68.9967995337195,-1.2862194261268,3.58822814482881));
#55399=CARTESIAN_POINT('Ctrl Pts',(-68.7979260020219,-3.71403499252018,
0.85772122850201));
#55400=CARTESIAN_POINT('Ctrl Pts',(-68.5990524703245,-2.7293875818599,-2.66086171370786));
#55401=CARTESIAN_POINT('Ctrl Pts',(-68.4001789386271,0.76302674318989,-3.73463944988864));
#55402=CARTESIAN_POINT('Ctrl Pts',(-68.2013054069296,3.55437052989495,-1.37702279127899));
#55403=CARTESIAN_POINT('Ctrl Pts',(-68.0024318752321,3.07995137564101,2.24580523536093));
#55404=CARTESIAN_POINT('Ctrl Pts',(-67.8035583435348,-0.224333426531556,
3.80518280050091));
#55405=CARTESIAN_POINT('Ctrl Pts',(-67.6046848118372,-3.32250021578923,
1.86835059546325));
#55406=CARTESIAN_POINT('Ctrl Pts',(-67.4058112801399,-3.36794698478127,
-1.78512597291907));
#55407=CARTESIAN_POINT('Ctrl Pts',(-67.2069377484423,-0.318917148843096,
-3.79842513203319));
#55408=CARTESIAN_POINT('Ctrl Pts',(-67.008064216745,3.02313441827591,-2.32172348063307));
#55409=CARTESIAN_POINT('Ctrl Pts',(-66.8091906850474,3.58752387456407,1.28818247190379));
#55410=CARTESIAN_POINT('Ctrl Pts',(-66.61031715335,0.855689028738441,3.71450372426576));
#55411=CARTESIAN_POINT('Ctrl Pts',(-66.4114436216526,-2.66235465365491,
2.72793132788374));
#55412=CARTESIAN_POINT('Ctrl Pts',(-66.212570089955,-3.73422141373034,-0.765069973744436));
#55413=CARTESIAN_POINT('Ctrl Pts',(-66.0136965582577,-1.37507787149593,
-3.555123412599));
#55414=CARTESIAN_POINT('Ctrl Pts',(-65.8148230265601,2.24749004247856,-3.07872216032026));
#55415=CARTESIAN_POINT('Ctrl Pts',(-65.6159494948628,3.80505949071416,0.22641533431646));
#55416=CARTESIAN_POINT('Ctrl Pts',(-65.4170759631652,1.8665324660573,3.32352195489086));
#55417=CARTESIAN_POINT('Ctrl Pts',(-65.2182024314679,-1.78696842091292,
3.36696977921506));
#55418=CARTESIAN_POINT('Ctrl Pts',(-65.0193288997703,-3.79859905361509,
0.316838857089779));
#55419=CARTESIAN_POINT('Ctrl Pts',(-64.8204553680729,-2.32006907629652,
-3.02440425748609));
#55420=CARTESIAN_POINT('Ctrl Pts',(-64.6215818363755,1.29014513205747,-3.5868185303575));
#55421=CARTESIAN_POINT('Ctrl Pts',(-64.422708304678,3.71497134405747,-0.853656572820322));
#55422=CARTESIAN_POINT('Ctrl Pts',(-64.2238347729806,2.72647425728869,2.66384679661379));
#55423=CARTESIAN_POINT('Ctrl Pts',(-64.024961241283,-0.767112975271716,
3.73380225971558));
#55424=CARTESIAN_POINT('Ctrl Pts',(-63.8260877095857,-3.55587523106043,
1.37313254007699));
#55425=CARTESIAN_POINT('Ctrl Pts',(-63.6272141778881,-3.07749202336981,
-2.24917417679972));
#55426=CARTESIAN_POINT('Ctrl Pts',(-63.4283406461908,0.228497174322965,
-3.80493504186522));
#55427=CARTESIAN_POINT('Ctrl Pts',(-63.2294671144933,3.32454269908083,-1.8647137778962));
#55428=CARTESIAN_POINT('Ctrl Pts',(-63.0305935827958,3.36599156573087,1.78881033396948));
#55429=CARTESIAN_POINT('Ctrl Pts',(-62.8317200510984,0.314760470489306,
3.79877183806881));
#55430=CARTESIAN_POINT('Ctrl Pts',(-62.6328465194009,-3.0256731913269,2.31841397743656));
#55431=CARTESIAN_POINT('Ctrl Pts',(-62.4339729877036,-3.58611211242019,
-1.29210740600025));
#55432=CARTESIAN_POINT('Ctrl Pts',(-62.2350994560059,-0.851623861356168,
-3.71543785175534));
#55433=CARTESIAN_POINT('Ctrl Pts',(-62.0362259243087,2.66533814213779,-2.72501637051098));
#55434=CARTESIAN_POINT('Ctrl Pts',(-61.837352392611,3.73338198796987,0.76915574716017));
#55435=CARTESIAN_POINT('Ctrl Pts',(-61.6384788609137,1.37118679760446,3.5566259850542));
#55436=CARTESIAN_POINT('Ctrl Pts',(-61.4396053292161,-2.2508576378202,3.07626096515786));
#55437=CARTESIAN_POINT('Ctrl Pts',(-61.2407317975188,-3.80480945399139,
-0.230578945927754));
#55438=CARTESIAN_POINT('Ctrl Pts',(-61.0418582658212,-1.86289453152446,
-3.32556244805351));
#55439=CARTESIAN_POINT('Ctrl Pts',(-60.8429847341239,1.79065171153737,-3.3650123446216));
#55440=CARTESIAN_POINT('Ctrl Pts',(-60.6441112024263,3.79894348534265,-0.312681989663811));
#55441=CARTESIAN_POINT('Ctrl Pts',(-60.445237670729,2.31675818454863,3.02694121941845));
#55442=CARTESIAN_POINT('Ctrl Pts',(-60.2463641390315,-1.29406929314464,
3.58540462096363));
#55443=CARTESIAN_POINT('Ctrl Pts',(-60.047490607334,-3.71590324721964,0.84959089495461));
#55444=CARTESIAN_POINT('Ctrl Pts',(-59.8486170756366,-2.72355766798716,
-2.6668286897804));
#55445=CARTESIAN_POINT('Ctrl Pts',(-59.6497435439391,0.77119828879821,-3.73296059861904));
#55446=CARTESIAN_POINT('Ctrl Pts',(-59.4508700122417,3.55737567435549,-1.36924064466089));
#55447=CARTESIAN_POINT('Ctrl Pts',(-59.2519964805442,3.07502898605303,2.25254042503595));
#55448=CARTESIAN_POINT('Ctrl Pts',(-59.0531229488468,-0.232660648507626,
3.80468272713029));
#55449=CARTESIAN_POINT('Ctrl Pts',(-58.8542494171493,-3.32658120150376,
1.86107472748661));
#55450=CARTESIAN_POINT('Ctrl Pts',(-58.6553758854518,-3.36403211618028,
-1.79249255306538));
#55451=CARTESIAN_POINT('Ctrl Pts',(-58.4565023537544,-0.310603415235633,
-3.79911399538513));
#55452=CARTESIAN_POINT('Ctrl Pts',(-58.2576288220569,3.02820834138102,-2.3151016981286));
#55453=CARTESIAN_POINT('Ctrl Pts',(-58.0587552903595,3.58469605619972,1.29603079290335));
#55454=CARTESIAN_POINT('Ctrl Pts',(-57.859881758662,0.84755767422402,3.71636753031121));
#55455=CARTESIAN_POINT('Ctrl Pts',(-57.6610082269646,-2.66831843909564,
2.72209815015362));
#55456=CARTESIAN_POINT('Ctrl Pts',(-57.4621346952671,-3.73253809178915,
-0.773240599574607));
#55457=CARTESIAN_POINT('Ctrl Pts',(-57.2632611635696,-1.3672940818287,-3.55812429873996));
#55458=CARTESIAN_POINT('Ctrl Pts',(-57.0643876318723,2.25422253794341,-3.073796086424));
#55459=CARTESIAN_POINT('Ctrl Pts',(-56.8655141001747,3.80455486131976,0.234742281439464));
#55460=CARTESIAN_POINT('Ctrl Pts',(-56.6666405684773,1.85925436632751,3.32759895912643));
#55461=CARTESIAN_POINT('Ctrl Pts',(-56.4677670367798,-1.79433285800241,
3.3630508807005));
#55462=CARTESIAN_POINT('Ctrl Pts',(-56.2688935050825,-3.79928336814536,
0.308524747826809));
#55463=CARTESIAN_POINT('Ctrl Pts',(-56.0700199733849,-2.313444518672,-3.02947455683556));
#55464=CARTESIAN_POINT('Ctrl Pts',(-55.8711464416876,1.29799190468937,-3.58398641834039));
#55465=CARTESIAN_POINT('Ctrl Pts',(-55.67227290999,3.71683070089097,-0.845524199773049));
#55466=CARTESIAN_POINT('Ctrl Pts',(-55.4733993782926,2.7206378174474,2.66980738963741));
#55467=CARTESIAN_POINT('Ctrl Pts',(-55.2745258465951,-0.77528267887785,
3.73211446760674));
#55468=CARTESIAN_POINT('Ctrl Pts',(-55.0756523148976,-3.55887185798348,
1.3653471096907));
#55469=CARTESIAN_POINT('Ctrl Pts',(-54.8767787832002,-3.0725622666399,-2.25590397603884));
#55470=CARTESIAN_POINT('Ctrl Pts',(-54.6779052515027,0.236823844100095,
-3.80442585659819));
#55471=CARTESIAN_POINT('Ctrl Pts',(-54.4790317198054,3.32861572061708,-1.857433448592));
#55472=CARTESIAN_POINT('Ctrl Pts',(-54.2801581881078,3.36206863847578,1.79617262579773));
#55473=CARTESIAN_POINT('Ctrl Pts',(-54.0812846564105,0.306445988059607,
3.7994516035725));
#55474=CARTESIAN_POINT('Ctrl Pts',(-53.8824111247129,-3.03073986540288,
2.31178664667509));
#55475=CARTESIAN_POINT('Ctrl Pts',(-53.6835375930156,-3.58327570759815,
-1.29995262791552));
#55476=CARTESIAN_POINT('Ctrl Pts',(-53.484664061318,-0.843490472210508,
-3.71729275882027));
#55477=CARTESIAN_POINT('Ctrl Pts',(-53.2857905296207,2.67129554096001,-2.71917667030568));
#55478=CARTESIAN_POINT('Ctrl Pts',(-53.086916997923,3.73168972619857,0.777324526096578));
#55479=CARTESIAN_POINT('Ctrl Pts',(-52.8880434662258,1.36339972882987,3.55961835186216));
#55480=CARTESIAN_POINT('Ctrl Pts',(-52.6891699345281,-2.25758473881897,
3.07132752707021));
#55481=CARTESIAN_POINT('Ctrl Pts',(-52.4902964028309,-3.80429571300419,
-0.238905335866445));
#55482=CARTESIAN_POINT('Ctrl Pts',(-52.2914228711333,-1.8556119748251,-3.32963148567123));
#55483=CARTESIAN_POINT('Ctrl Pts',(-52.0925493394359,1.79801185590047,-3.36108538980027));
#55484=CARTESIAN_POINT('Ctrl Pts',(-51.8936758077384,3.79961870161625,-0.304367136556382));
#55485=CARTESIAN_POINT('Ctrl Pts',(-51.694802276041,2.31012808263415,3.03200426670422));
#55486=CARTESIAN_POINT('Ctrl Pts',(-51.4959287443436,-1.30191296199484,
3.58256392418577));
#55487=CARTESIAN_POINT('Ctrl Pts',(-51.297055212646,-3.71775370396079,0.841456492145185));
#55488=CARTESIAN_POINT('Ctrl Pts',(-51.0981816809486,-2.71771470916588,
-2.67278289261786));
#55489=CARTESIAN_POINT('Ctrl Pts',(-50.8993081492511,0.779366140619599,
-3.73126386769187));
#55490=CARTESIAN_POINT('Ctrl Pts',(-50.7004346175537,3.56036378015273,-1.36145193982897));
#55491=CARTESIAN_POINT('Ctrl Pts',(-50.5015610858562,3.07009186808429,2.25926482578078));
#55492=CARTESIAN_POINT('Ctrl Pts',(-50.3026875541588,-0.240986756115434,
3.80416443057663));
#55493=CARTESIAN_POINT('Ctrl Pts',(-50.1038140224613,-3.3306462539848,1.8537899455722));
#55494=CARTESIAN_POINT('Ctrl Pts',(-49.9049404907639,-3.36010113496832,
-1.79985054776005));
#55495=CARTESIAN_POINT('Ctrl Pts',(-49.7060669590664,-0.302288193939447,
-3.79978466222657));
#55496=CARTESIAN_POINT('Ctrl Pts',(-49.507193427369,3.03326776036106,-2.30846882704571));
#55497=CARTESIAN_POINT('Ctrl Pts',(-49.3083198956714,3.58185106831631,1.3038729063405));
#55498=CARTESIAN_POINT('Ctrl Pts',(-49.1094463639741,0.839422260186034,
3.71821353617451));
#55499=CARTESIAN_POINT('Ctrl Pts',(-48.9105728322766,-2.6742694441658,2.71625193446565));
#55500=CARTESIAN_POINT('Ctrl Pts',(-48.7116993005792,-3.73083689221413,
-0.781407521835786));
#55501=CARTESIAN_POINT('Ctrl Pts',(-48.5128257688817,-1.35950374327106,
-3.56110814263194));
#55502=CARTESIAN_POINT('Ctrl Pts',(-48.3139522371842,2.26094423642121,-3.06885529005218));
#55503=CARTESIAN_POINT('Ctrl Pts',(-48.1150787054868,3.80403200935488,0.243068104223925));
#55504=CARTESIAN_POINT('Ctrl Pts',(-47.9162051737893,1.85196736137869,3.33166002525401));
#55505=CARTESIAN_POINT('Ctrl Pts',(-47.7173316420919,-1.80168870082603,
3.35911587427456));
#55506=CARTESIAN_POINT('Ctrl Pts',(-47.5184581103944,-3.79994948535379,
0.300209160831137));
#55507=CARTESIAN_POINT('Ctrl Pts',(-47.319584578697,-2.30680888040646,-3.0345303459951));
#55508=CARTESIAN_POINT('Ctrl Pts',(-47.1207110469995,1.30583246036561,-3.5811371402032));
#55509=CARTESIAN_POINT('Ctrl Pts',(-46.9218375153022,3.71867225532388,-0.837387776942048));
#55510=CARTESIAN_POINT('Ctrl Pts',(-46.7229639836046,2.71478834664286,2.67575519515887));
#55511=CARTESIAN_POINT('Ctrl Pts',(-46.5240904519072,-0.783448669134082,
3.73040879989306));
#55512=CARTESIAN_POINT('Ctrl Pts',(-46.3252169202097,-3.56185143907695,
1.35755513973942));
#55513=CARTESIAN_POINT('Ctrl Pts',(-46.1263433885122,-3.06761779334405,
-2.26262297023752));
#55514=CARTESIAN_POINT('Ctrl Pts',(-45.9274698568148,0.245149379568856,
-3.80389844937855));
#55515=CARTESIAN_POINT('Ctrl Pts',(-45.7285963251173,3.33267279917539,-1.8501442227902));
#55516=CARTESIAN_POINT('Ctrl Pts',(-45.5297227934199,3.35812960801393,1.80352631454818));
#55517=CARTESIAN_POINT('Ctrl Pts',(-45.3308492617224,0.298130037853896,
3.80011317094853));
#55518=CARTESIAN_POINT('Ctrl Pts',(-45.131975730025,-3.03579202322847,2.30514824321336));
#55519=CARTESIAN_POINT('Ctrl Pts',(-44.9331021983275,-3.58042214006016,
-1.30779162348385));
#55520=CARTESIAN_POINT('Ctrl Pts',(-44.7342286666301,-0.835353043022,-3.7191298612715));
#55521=CARTESIAN_POINT('Ctrl Pts',(-44.5353551349326,2.67724014515226,-2.71332394613555));
#55522=CARTESIAN_POINT('Ctrl Pts',(-44.3364816032351,3.72997959085687,0.785489581903391));
#55523=CARTESIAN_POINT('Ctrl Pts',(-44.1376080715378,1.35560612981737,3.56259366926528));
#55524=CARTESIAN_POINT('Ctrl Pts',(-43.9387345398402,-2.2643010267272,3.06637937833035));
#55525=CARTESIAN_POINT('Ctrl Pts',(-43.7398610081428,-3.80376375068764,
-0.247230581527181));
#55526=CARTESIAN_POINT('Ctrl Pts',(-43.5409874764454,-1.84832053035247,
-3.33368457544577));
#55527=CARTESIAN_POINT('Ctrl Pts',(-43.3421139447478,1.80536338837631,-3.35714233648167));
#55528=CARTESIAN_POINT('Ctrl Pts',(-43.1432404130505,3.80027571896185,-0.296050825630079));
#55529=CARTESIAN_POINT('Ctrl Pts',(-42.944366881353,2.30348691596348,3.03705279168351));
#55530=CARTESIAN_POINT('Ctrl Pts',(-42.7454933496556,-1.30975039510868,
3.57970606810114));
#55531=CARTESIAN_POINT('Ctrl Pts',(-42.546619817958,-3.71958635388042,0.833318059035165));
#55532=CARTESIAN_POINT('Ctrl Pts',(-42.3477462862607,-2.71185873338217,
-2.67872429370146));
#55533=CARTESIAN_POINT('Ctrl Pts',(-42.1488727545632,0.787530259532762,
-3.72954926523403));
#55534=CARTESIAN_POINT('Ctrl Pts',(-41.9499992228658,3.56333483297472,-1.35365671408838));
#55535=CARTESIAN_POINT('Ctrl Pts',(-41.7511256911682,3.06514004538181,2.2659784053879));
#55536=CARTESIAN_POINT('Ctrl Pts',(-41.5522521594708,-0.249311709475826,
3.80362791332241));
#55537=CARTESIAN_POINT('Ctrl Pts',(-41.3533786277734,-3.33469535376215,
1.84649628461158));
#55538=CARTESIAN_POINT('Ctrl Pts',(-41.154505096076,-3.35615405997345,-1.80719992176053));
#55539=CARTESIAN_POINT('Ctrl Pts',(-40.9556315643784,-0.293971524782049,
-3.8004371293451));
#55540=CARTESIAN_POINT('Ctrl Pts',(-40.7567580326811,3.03831265098276,-2.30182489915407));
#55541=CARTESIAN_POINT('Ctrl Pts',(-40.5578845009835,3.57898892454058,1.31170877465366));
#55542=CARTESIAN_POINT('Ctrl Pts',(-40.3590109692861,0.831282825590706,
3.72004173301395));
#55543=CARTESIAN_POINT('Ctrl Pts',(-40.1601374375886,-2.68020764036213,
2.71039270882136));
#55544=CARTESIAN_POINT('Ctrl Pts',(-39.9612639058912,-3.7291178231534,-0.789570701411317));
#55545=CARTESIAN_POINT('Ctrl Pts',(-39.7623903741938,-1.35170689313597,
-3.56407492998341));
#55546=CARTESIAN_POINT('Ctrl Pts',(-39.5635168424963,2.2676551057174,-3.06389979486944));
#55547=CARTESIAN_POINT('Ctrl Pts',(-39.3646433107988,3.80349093732365,0.251392762791839));
#55548=CARTESIAN_POINT('Ctrl Pts',(-39.1657697791013,1.84467148611344,3.33570513382216));
#55549=CARTESIAN_POINT('Ctrl Pts',(-38.966896247404,-1.80903591415121,3.35516477878489));
#55550=CARTESIAN_POINT('Ctrl Pts',(-38.7680227157065,-3.8005974020499,0.291892135932223));
#55551=CARTESIAN_POINT('Ctrl Pts',(-38.569149184009,-2.30016219328273,-3.03957160074908));
#55552=CARTESIAN_POINT('Ctrl Pts',(-38.3702756523116,1.31366676153256,-3.57827070959312));
#55553=CARTESIAN_POINT('Ctrl Pts',(-38.1714021206141,3.7204959985358,-0.829247343297895));
#55554=CARTESIAN_POINT('Ctrl Pts',(-37.9725285889167,2.70892587289195,2.68169018469027));
#55555=CARTESIAN_POINT('Ctrl Pts',(-37.7736550572192,-0.791610906928228,
3.7286852647441));
#55556=CARTESIAN_POINT('Ctrl Pts',(-37.5747815255217,-3.56481396006973,
1.34975666754391));
#55557=CARTESIAN_POINT('Ctrl Pts',(-37.3759079938243,-3.06265862716454,
-2.26933112721388));
#55558=CARTESIAN_POINT('Ctrl Pts',(-37.1770344621268,0.253473740852287,
-3.80335282273231));
#55559=CARTESIAN_POINT('Ctrl Pts',(-36.9781609304294,3.33671391532343,-1.84284613540428));
#55560=CARTESIAN_POINT('Ctrl Pts',(-36.7792873987319,3.35417449321223,1.81087136499863));
#55561=CARTESIAN_POINT('Ctrl Pts',(-36.5804138670345,0.289812659703135,
3.80075653702829));
#55562=CARTESIAN_POINT('Ctrl Pts',(-36.381540335337,-3.04082964060558,2.29849879884721));
#55563=CARTESIAN_POINT('Ctrl Pts',(-36.1826668036395,-3.57755142347379,
-1.31562435515925));
#55564=CARTESIAN_POINT('Ctrl Pts',(-35.9837932719421,-0.827211612766053,
-3.72094915030997));
#55565=CARTESIAN_POINT('Ctrl Pts',(-35.7849197402446,2.68317192624198,-2.70745822603308));
#55566=CARTESIAN_POINT('Ctrl Pts',(-35.5860462085473,3.72825159013562,0.793650875472599));
#55567=CARTESIAN_POINT('Ctrl Pts',(-35.3871726768497,1.34780603789606,3.56555192301254));
#55568=CARTESIAN_POINT('Ctrl Pts',(-35.1882991451524,-2.27100646937564,
3.06141654263865));
#55569=CARTESIAN_POINT('Ctrl Pts',(-34.9894256134548,-3.80321356958969,
-0.255554643034271));
#55570=CARTESIAN_POINT('Ctrl Pts',(-34.7905520817575,-1.84102023303062,
-3.33772169796395));
#55571=CARTESIAN_POINT('Ctrl Pts',(-34.5916785500599,1.81270627375333,-3.35318320355194));
#55572=CARTESIAN_POINT('Ctrl Pts',(-34.3928050183625,3.80091453423265,-0.287733096717287));
#55573=CARTESIAN_POINT('Ctrl Pts',(-34.193931486665,2.29683471634544,3.04208677017568));
#55574=CARTESIAN_POINT('Ctrl Pts',(-33.9950579549676,-1.3175815549477,3.5768310663979));
#55575=CARTESIAN_POINT('Ctrl Pts',(-33.7961844232701,-3.72140118820076,
0.825175634604654));
#55576=CARTESIAN_POINT('Ctrl Pts',(-33.5973108915727,-2.70598976868411,
-2.68465286457377));
#55577=CARTESIAN_POINT('Ctrl Pts',(-33.3984373598752,0.795690606434006,
-3.72781679945786));
#55578=CARTESIAN_POINT('Ctrl Pts',(-33.1995638281778,3.56628881859093,-1.34585500477608));
#55579=CARTESIAN_POINT('Ctrl Pts',(-33.0006902964803,3.06017354166348,2.27268113170112));
#55580=CARTESIAN_POINT('Ctrl Pts',(-32.8018167647829,-0.257635468714778,
3.8030731779375));
#55581=CARTESIAN_POINT('Ctrl Pts',(-32.6029432330854,-3.33872848144206,
1.83919377953904));
#55582=CARTESIAN_POINT('Ctrl Pts',(-32.4040697013879,-3.35219091010075,
-1.81454063986603));
#55583=CARTESIAN_POINT('Ctrl Pts',(-32.2051961696905,-0.285653447597213,
-3.80107139361567));
#55584=CARTESIAN_POINT('Ctrl Pts',(-32.0063226379931,3.04334298908304,-2.29516994627558));
#55585=CARTESIAN_POINT('Ctrl Pts',(-31.8074491062956,3.57610963858108,1.31953836031194));
#55586=CARTESIAN_POINT('Ctrl Pts',(-31.6085755745982,0.823139409423143,
3.72185211207294));
#55587=CARTESIAN_POINT('Ctrl Pts',(-31.4097020429007,-2.68613299924237,
2.7045205012846));
#55588=CARTESIAN_POINT('Ctrl Pts',(-31.2108285112032,-3.72738089284084,
-0.797730099201816));
#55589=CARTESIAN_POINT('Ctrl Pts',(-31.0119549795058,-1.34390356876819,
-3.56702464658427));
#55590=CARTESIAN_POINT('Ctrl Pts',(-30.8130814478083,2.27435511368902,-3.05892962461122));
#55591=CARTESIAN_POINT('Ctrl Pts',(-30.6142079161109,3.80293164781777,0.259716217270925));
#55592=CARTESIAN_POINT('Ctrl Pts',(-30.4153343844134,1.83736677547631,3.33973426545636));
#55593=CARTESIAN_POINT('Ctrl Pts',(-30.216460852716,-1.81637446278761,3.35119761315571));
#55594=CARTESIAN_POINT('Ctrl Pts',(-30.0175873210184,-3.80122711513034,
0.283573712965513));
#55595=CARTESIAN_POINT('Ctrl Pts',(-29.8187137893211,-2.29350448913609,
-3.04459829695148));
#55596=CARTESIAN_POINT('Ctrl Pts',(-29.6198402576236,1.32149477066622,-3.57538714023941));
#55597=CARTESIAN_POINT('Ctrl Pts',(-29.4209667259261,3.72230192179151,-0.821102937831022));
#55598=CARTESIAN_POINT('Ctrl Pts',(-29.2220931942287,2.70305042427431,2.68761232980465));
#55599=CARTESIAN_POINT('Ctrl Pts',(-29.0232196625312,-0.799769353165428,
3.72694387041513));
#55600=CARTESIAN_POINT('Ctrl Pts',(-28.8243461308338,-3.5677594067723,1.34195173045655));
#55601=CARTESIAN_POINT('Ctrl Pts',(-28.6254725991363,-3.05768479185423,
-2.27602841483819));
#55602=CARTESIAN_POINT('Ctrl Pts',(-28.4265990674389,0.261796888079818,
-3.80278897927288));
#55603=CARTESIAN_POINT('Ctrl Pts',(-28.2277255357414,3.34073904970577,-1.83553922138932));
#55604=CARTESIAN_POINT('Ctrl Pts',(-28.028852004044,3.35020331301418,1.81820774196901));
#55605=CARTESIAN_POINT('Ctrl Pts',(-27.8299784723465,0.281493893444737,
3.80138169873015));
#55606=CARTESIAN_POINT('Ctrl Pts',(-27.6311049406491,-3.04585269340545,
2.2918383454254));
#55607=CARTESIAN_POINT('Ctrl Pts',(-27.4322314089516,-3.57466357158898,
-1.32345078542506));
#55608=CARTESIAN_POINT('Ctrl Pts',(-27.2333578772542,-0.819066220437877,
-3.72275061722178));
#55609=CARTESIAN_POINT('Ctrl Pts',(-27.0344843455567,2.68909085581776,-2.70157953809338));
#55610=CARTESIAN_POINT('Ctrl Pts',(-26.8356108138592,3.72650573231153,0.801808367714392));
#55611=CARTESIAN_POINT('Ctrl Pts',(-26.6367372821618,1.33999949042545,3.56849309893504));
#55612=CARTESIAN_POINT('Ctrl Pts',(-26.4378637504643,-2.27770103464773,
3.05643904376517));
#55613=CARTESIAN_POINT('Ctrl Pts',(-26.2389902187669,-3.80264517234552,
-0.263877480518609));
#55614=CARTESIAN_POINT('Ctrl Pts',(-26.0401166870694,-1.83371111782523,
-3.34174283388943));
#55615=CARTESIAN_POINT('Ctrl Pts',(-25.841243155372,1.82004047686151,-3.34920800997384));
#55616=CARTESIAN_POINT('Ctrl Pts',(-25.6423696236745,3.80153514436882,-0.279413989657449));
#55617=CARTESIAN_POINT('Ctrl Pts',(-25.4434960919771,2.29017151564223,3.04710617806936));
#55618=CARTESIAN_POINT('Ctrl Pts',(-25.2446225602796,-1.32540640400279,
3.57393893284649));
#55619=CARTESIAN_POINT('Ctrl Pts',(-25.0457490285822,-3.72319819822944,
0.817029257853469));
#55620=CARTESIAN_POINT('Ctrl Pts',(-24.8468754968847,-2.70010784318212,
-2.69056857683908));
#55621=CARTESIAN_POINT('Ctrl Pts',(-24.6480019651872,0.803847142238303,
-3.72606647866122));
#55622=CARTESIAN_POINT('Ctrl Pts',(-24.4491284334898,3.56922572285289,-1.33804684925931));
#55623=CARTESIAN_POINT('Ctrl Pts',(-24.2502549017923,3.05519238071696,2.27937297261687));
#55624=CARTESIAN_POINT('Ctrl Pts',(-24.0513813700949,-0.265957993964293,
3.80250022707872));
#55625=CARTESIAN_POINT('Ctrl Pts',(-23.8525078383974,-3.34274561770695,
1.83188246533136));
#55626=CARTESIAN_POINT('Ctrl Pts',(-23.6536343067,-3.34821170433262,-1.82187266691653));
#55627=CARTESIAN_POINT('Ctrl Pts',(-23.4547607750025,-0.277334002226216,
-3.80168745200032));
#55628=CARTESIAN_POINT('Ctrl Pts',(-23.2558872433051,3.04835875056794,-2.28850400028564));
#55629=CARTESIAN_POINT('Ctrl Pts',(-23.0570137116076,3.57321322422885,1.32736162581399));
#55630=CARTESIAN_POINT('Ctrl Pts',(-22.8581401799102,0.814992050687579,
3.7236446646805));
#55631=CARTESIAN_POINT('Ctrl Pts',(-22.6592666482127,-2.69204549242627,
2.69863533998111));
#55632=CARTESIAN_POINT('Ctrl Pts',(-22.4603931165153,-3.72562610959568,
-0.80588567612687));
#55633=CARTESIAN_POINT('Ctrl Pts',(-22.2615195848178,-1.33609380754272,
-3.56995727830645));
#55634=CARTESIAN_POINT('Ctrl Pts',(-22.0626460531204,2.28104422824517,-3.05394480308283));
#55635=CARTESIAN_POINT('Ctrl Pts',(-21.8637725214229,3.80235414351597,0.268038427794315));
#55636=CARTESIAN_POINT('Ctrl Pts',(-21.6648989897255,1.83005326445484,3.34374740085816));
#55637=CARTESIAN_POINT('Ctrl Pts',(-21.466025458028,-1.82370431158557,3.34721439638869));
#55638=CARTESIAN_POINT('Ctrl Pts',(-21.2671519263306,-3.80183862157912,
0.275253931773772));
#55639=CARTESIAN_POINT('Ctrl Pts',(-21.0682783946331,-2.28683579985479,
-3.04961041052624));
#55640=CARTESIAN_POINT('Ctrl Pts',(-20.8694048629357,1.32931645027334,-3.57248644595332));
#55641=CARTESIAN_POINT('Ctrl Pts',(-20.6705313312382,3.72409001644133,-0.812954599550049));
#55642=CARTESIAN_POINT('Ctrl Pts',(-20.4716577995407,2.69716202893111,2.69352160213719));
#55643=CARTESIAN_POINT('Ctrl Pts',(-20.2727842678433,-0.807923968769751,
3.72518462524672));
#55644=CARTESIAN_POINT('Ctrl Pts',(-20.0739107361458,-3.57068776507683,
1.33414036586029));
#55645=CARTESIAN_POINT('Ctrl Pts',(-19.8750372044484,-3.05269631123622,
-2.28271480103238));
#55646=CARTESIAN_POINT('Ctrl Pts',(-19.6761636727509,0.270118781385866,
-3.80220692170089));
#55647=CARTESIAN_POINT('Ctrl Pts',(-19.4772901410535,3.34474818304312,-1.82822351574342));
#55648=CARTESIAN_POINT('Ctrl Pts',(-19.278416609356,3.34621608644065,1.82553541032031));
#55649=CARTESIAN_POINT('Ctrl Pts',(-19.0795430776586,0.27317377892279,3.80198865305994));
#55650=CARTESIAN_POINT('Ctrl Pts',(-18.8806695459611,-3.05086115756956,
2.28516691484908));
#55651=CARTESIAN_POINT('Ctrl Pts',(-18.6817960142636,-3.57175859823745,
-1.33127087679568));
#55652=CARTESIAN_POINT('Ctrl Pts',(-18.4829224825662,-0.810916905050859,
-3.72453425337853));
#55653=CARTESIAN_POINT('Ctrl Pts',(-18.2840489508687,2.69499690552984,-2.69568791047329));
#55654=CARTESIAN_POINT('Ctrl Pts',(-18.0851754191713,3.72474202574661,0.809962019556789));
#55655=CARTESIAN_POINT('Ctrl Pts',(-17.8863018874738,1.33218652479678,3.57141718294536));
#55656=CARTESIAN_POINT('Ctrl Pts',(-17.6874283557764,-2.28438469047839,
3.05144690555078));
#55657=CARTESIAN_POINT('Ctrl Pts',(-17.4885548240789,-3.80205856167758,
-0.272199054116103));
#55658=CARTESIAN_POINT('Ctrl Pts',(-17.2896812923814,-1.82639321974484,
-3.34574796396226));
#55659=CARTESIAN_POINT('Ctrl Pts',(-17.0908077606841,1.82736596257257,-3.34521677478736));
#55660=CARTESIAN_POINT('Ctrl Pts',(-16.8919342289865,3.8021375463979,-0.271093544295971));
#55661=CARTESIAN_POINT('Ctrl Pts',(-16.6930606972891,2.28349734576807,3.05211099132349));
#55662=CARTESIAN_POINT('Ctrl Pts',(-16.4941871655916,-1.33322490479584,
3.57102968129913));
#55663=CARTESIAN_POINT('Ctrl Pts',(-16.2953136338942,-3.72497737535923,
0.808878967799967));
#55664=CARTESIAN_POINT('Ctrl Pts',(-16.0964401021967,-2.69421298504881,
-2.6964714021628));
#55665=CARTESIAN_POINT('Ctrl Pts',(-15.8975665704993,0.811999827878098,
-3.7242983112277));
#55666=CARTESIAN_POINT('Ctrl Pts',(-15.6986930388018,3.57214553169364,-1.33023228493699));
#55667=CARTESIAN_POINT('Ctrl Pts',(-15.4998195071044,3.05019658640061,2.28605389608329));
#55668=CARTESIAN_POINT('Ctrl Pts',(-15.3009459754069,-0.274279245362296,
3.80190906349047));
#55669=CARTESIAN_POINT('Ctrl Pts',(-15.1020724437095,-3.34674674331627,
1.824562377007));
#55670=CARTESIAN_POINT('Ctrl Pts',(-14.903198912012,-3.34421646172796,-1.82919596779439));
#55671=CARTESIAN_POINT('Ctrl Pts',(-14.7043253803146,-0.269013228516049,
-3.80228530154838));
#55672=CARTESIAN_POINT('Ctrl Pts',(-14.5054518486171,3.05335991141382,-2.28182709311162));
#55673=CARTESIAN_POINT('Ctrl Pts',(-14.3065783169197,3.5702996953566,1.33517853368896));
#55674=CARTESIAN_POINT('Ctrl Pts',(-14.1077047852222,0.806840788407417,
3.72541938225076));
#55675=CARTESIAN_POINT('Ctrl Pts',(-13.9088312535248,-2.69794509159463,
2.69273725309915));
#55676=CARTESIAN_POINT('Ctrl Pts',(-13.7099577218273,-3.72385348182286,
-0.8140373931235));
#55677=CARTESIAN_POINT('Ctrl Pts',(-13.5110841901299,-1.32827764686602,
-3.57287281110364));
#55678=CARTESIAN_POINT('Ctrl Pts',(-13.3122106584324,2.28772241734737,-3.04894535415999));
#55679=CARTESIAN_POINT('Ctrl Pts',(-13.113337126735,3.80175842718431,0.276359354501727));
#55680=CARTESIAN_POINT('Ctrl Pts',(-12.9144635950375,1.82273098807798,3.34774452080618));
#55681=CARTESIAN_POINT('Ctrl Pts',(-12.7155900633401,-1.83102542543786,
3.3432151475619));
#55682=CARTESIAN_POINT('Ctrl Pts',(-12.5167165316426,-3.80243191846715,
0.266932832205924));
#55683=CARTESIAN_POINT('Ctrl Pts',(-12.3178429999452,-2.28015615737979,
-3.05460791746674));
#55684=CARTESIAN_POINT('Ctrl Pts',(-12.1189694682477,1.33713176289026,-3.56956864062838));
#55685=CARTESIAN_POINT('Ctrl Pts',(-11.9200959365502,3.72586027392076,-0.804802367483259));
#55686=CARTESIAN_POINT('Ctrl Pts',(-11.7212224048527,2.69126071506615,2.6994179733841));
#55687=CARTESIAN_POINT('Ctrl Pts',(-11.5223488731553,-0.816074714683047,
3.72340753766527));
#55688=CARTESIAN_POINT('Ctrl Pts',(-11.3234753414579,-3.57359902095764,
1.32632261116899));
#55689=CARTESIAN_POINT('Ctrl Pts',(-11.1246018097604,-3.04769320920348,
-2.28939025377118));
#55690=CARTESIAN_POINT('Ctrl Pts',(-10.925728278063,0.278439380911714,-3.80160665280418));
#55691=CARTESIAN_POINT('Ctrl Pts',(-10.7268547463655,3.34874129613322,-1.82089905350606));
#55692=CARTESIAN_POINT('Ctrl Pts',(-10.5279812146681,3.34221283258897,1.83285433495541));
#55693=CARTESIAN_POINT('Ctrl Pts',(-10.3291076829706,0.264852355988142,
3.80257739711041));
#55694=CARTESIAN_POINT('Ctrl Pts',(-10.1302341512731,-3.05585500910874,
2.27848453907253));
#55695=CARTESIAN_POINT('Ctrl Pts',(-9.93136061957569,-3.56883651733323,
-1.33908459181509));
#55696=CARTESIAN_POINT('Ctrl Pts',(-9.73248708787821,-0.80276370563772,
-3.72630005023728));
#55697=CARTESIAN_POINT('Ctrl Pts',(-9.53361355618079,2.70089004709043,-2.68978337139171));
#55698=CARTESIAN_POINT('Ctrl Pts',(-9.33474002448332,3.72296047888839,0.818111791946939));
#55699=CARTESIAN_POINT('Ctrl Pts',(-9.13586649278587,1.32436717843105,3.5743241610383));
#55700=CARTESIAN_POINT('Ctrl Pts',(-8.9369929610884,-2.29105740485551,3.04644015190587));
#55701=CARTESIAN_POINT('Ctrl Pts',(-8.73811942939098,-3.80145374039546,
-0.280519323969575));
#55702=CARTESIAN_POINT('Ctrl Pts',(-8.53924589769349,-1.81906657383958,
-3.34973706899915));
#55703=CARTESIAN_POINT('Ctrl Pts',(-8.34037236599607,1.83468269579965,-3.34120951710917));
#55704=CARTESIAN_POINT('Ctrl Pts',(-8.14149883429859,3.80272173743456,-0.262771800485379));
#55705=CARTESIAN_POINT('Ctrl Pts',(-7.94262530260113,2.27681223869029,3.05710118596646));
#55706=CARTESIAN_POINT('Ctrl Pts',(-7.74375177090369,-1.34103701987869,
3.5681033256903));
#55707=CARTESIAN_POINT('Ctrl Pts',(-7.54487823920625,-3.72673871106872,
0.800724803481259));
#55708=CARTESIAN_POINT('Ctrl Pts',(-7.34600470750877,-2.68830522251812,
-2.70236131227278));
#55709=CARTESIAN_POINT('Ctrl Pts',(-7.14713117581134,0.820148624304898,
-3.72251230562602));
#55710=CARTESIAN_POINT('Ctrl Pts',(-6.94825764411385,3.57504823112902,-1.32241134923795));
#55711=CARTESIAN_POINT('Ctrl Pts',(-6.74938411241644,3.04518618264129,2.29272387010146));
#55712=CARTESIAN_POINT('Ctrl Pts',(-6.55051058071893,-0.282599183050784,
3.80129969000349));
#55713=CARTESIAN_POINT('Ctrl Pts',(-6.35163704902152,-3.35073183910972,
1.8172335496281));
#55714=CARTESIAN_POINT('Ctrl Pts',(-6.15276351732402,-3.34020520141543,
-1.83651050742555));
#55715=CARTESIAN_POINT('Ctrl Pts',(-5.9538899856266,-0.260691166334333,
-3.80286493939216));
#55716=CARTESIAN_POINT('Ctrl Pts',(-5.75501645392915,3.05834644769266,-2.27513925674164));
#55717=CARTESIAN_POINT('Ctrl Pts',(-5.5561429222317,3.56736906587033,1.34298904651157));
#55718=CARTESIAN_POINT('Ctrl Pts',(-5.35726939053425,0.798685661716399,
3.72717625625544));
#55719=CARTESIAN_POINT('Ctrl Pts',(-5.15839585883678,-2.70383176866502,
2.68682626894128));
#55720=CARTESIAN_POINT('Ctrl Pts',(-4.95952232713934,-3.72206301768338,
-0.822185211248298));
#55721=CARTESIAN_POINT('Ctrl Pts',(-4.76064879544187,-1.32045512479611,
-3.57577123082234));
#55722=CARTESIAN_POINT('Ctrl Pts',(-4.56177526374442,2.29438965018289,-3.04393130214526));
#55723=CARTESIAN_POINT('Ctrl Pts',(-4.36290173204696,3.80114449946005,0.284678958212554));
#55724=CARTESIAN_POINT('Ctrl Pts',(-4.1640282003495,1.81539998560147,3.35172560488281));
#55725=CARTESIAN_POINT('Ctrl Pts',(-3.96515466865207,-1.83833777717959,
3.33919988823347));
#55726=CARTESIAN_POINT('Ctrl Pts',(-3.76628113695461,-3.80300698803449,
0.258610449579765));
#55727=CARTESIAN_POINT('Ctrl Pts',(-3.56740760525717,-2.27346562187304,
-3.05959078526946));
#55728=CARTESIAN_POINT('Ctrl Pts',(-3.3685340735597,1.34494072427348,-3.56663375441676));
#55729=CARTESIAN_POINT('Ctrl Pts',(-3.16966054186226,3.72761258531972,-0.796646250131117));
#55730=CARTESIAN_POINT('Ctrl Pts',(-2.97078701016478,2.685346700579,2.70530135762789));
#55731=CARTESIAN_POINT('Ctrl Pts',(-2.77191347846734,-0.824221909934967,
3.72161272508666));
#55732=CARTESIAN_POINT('Ctrl Pts',(-2.57303994676988,-3.57649248436405,
1.31849829819329));
#55733=CARTESIAN_POINT('Ctrl Pts',(-2.37416641507242,-3.04267678634614,
-2.29605435280299));
#55734=CARTESIAN_POINT('Ctrl Pts',(-2.175292883375,0.286761057335244,-3.80098890860613));
#55735=CARTESIAN_POINT('Ctrl Pts',(-1.97641935167752,3.35271381827749,-1.813564485426));
#55736=CARTESIAN_POINT('Ctrl Pts',(-1.77754581998009,3.33820216492901,1.84016186691663));
#55737=CARTESIAN_POINT('Ctrl Pts',(-1.57867228828261,0.256513436717102,
3.8031528636426));
#55738=CARTESIAN_POINT('Ctrl Pts',(-1.37979875658517,-3.06080358273695,
2.2717819307131));
#55739=CARTESIAN_POINT('Ctrl Pts',(-1.1809252248877,-3.5659552001554,-1.3468742960899));
#55740=CARTESIAN_POINT('Ctrl Pts',(-0.982051693190254,-0.794497413703714,
-3.72808122654754));
#55741=CARTESIAN_POINT('Ctrl Pts',(-0.783178161492791,2.70656396064839,
-2.6838032048931));
#55742=CARTESIAN_POINT('Ctrl Pts',(-0.584304629795337,3.72155070290039,
0.826139135082401));
#55743=CARTESIAN_POINT('Ctrl Pts',(-0.385431098097896,1.31580516862223,
3.57743809331671));
#55744=CARTESIAN_POINT('Ctrl Pts',(-0.186557566400446,-2.29632333640214,
3.0409932439337));
#55745=CARTESIAN_POINT('Ctrl Pts',(0.0123159652970102,-3.80351113009631,
-0.28801457243628));
#55746=CARTESIAN_POINT('Ctrl Pts',(0.211189496994464,-1.80630503125545,
-3.35542702025725));
#55747=CARTESIAN_POINT('Ctrl Pts',(0.343771851459434,0.617181736105881,
-3.34041968432337));
#55748=CARTESIAN_POINT('Ctrl Pts',(0.410063028691923,1.55734592416847,-2.82148741534955));
#55749=CARTESIAN_POINT('',(0.,1.90056365518826,-3.44330463255539));
#55750=CARTESIAN_POINT('Ctrl Pts',(-3.33066907387547E-15,-3.22795401163284,
-0.0459738408030351));
#55751=CARTESIAN_POINT('Ctrl Pts',(-4.69857332999488E-15,-3.23446946289896,
-0.112579638718265));
#55752=CARTESIAN_POINT('Ctrl Pts',(2.81156677457225E-14,-3.23875117277606,
-0.179298023073995));
#55753=CARTESIAN_POINT('Ctrl Pts',(2.14273043752655E-14,-3.24075548586217,
-0.246033167079983));
#55754=CARTESIAN_POINT('Ctrl Pts',(1.11493109045283E-14,-3.24383550943018,
-0.348584917989921));
#55755=CARTESIAN_POINT('Ctrl Pts',(-1.17848145713982E-14,-3.24154057034996,
-0.45117578255498));
#55756=CARTESIAN_POINT('Ctrl Pts',(-8.99280649946377E-15,-3.2341405851747,
-0.553505501924448));
#55757=CARTESIAN_POINT('Ctrl Pts',(-7.22947464868693E-15,-3.22946702076564,
-0.61813327118452));
#55758=CARTESIAN_POINT('Ctrl Pts',(1.45550265953282E-14,-3.22275614360847,
-0.682657225405645));
#55759=CARTESIAN_POINT('Ctrl Pts',(1.34336985979644E-14,-3.21406567034608,
-0.747003854712476));
#55760=CARTESIAN_POINT('Ctrl Pts',(1.27129131778372E-14,-3.20847946681219,
-0.788365626065484));
#55761=CARTESIAN_POINT('Ctrl Pts',(2.21527997058171E-14,-3.20207516116718,
-0.829654156267173));
#55762=CARTESIAN_POINT('Ctrl Pts',(2.13717932240343E-14,-3.19486642441298,
-0.870850049402691));
#55763=CARTESIAN_POINT('Ctrl Pts',(2.10197089137425E-14,-3.19161666507374,
-0.889421505542671));
#55764=CARTESIAN_POINT('Ctrl Pts',(5.32010578988216E-15,-3.18820341775595,
-0.907973609936308));
#55765=CARTESIAN_POINT('Ctrl Pts',(6.93889390390723E-15,-3.18463068805892,
-0.926491266493227));
#55766=CARTESIAN_POINT('Ctrl Pts',(1.60458093774972E-14,-3.16453136370697,
-1.03066718153223));
#55767=CARTESIAN_POINT('Ctrl Pts',(2.31518269366155E-14,-3.13937025133027,
-1.1338608875346));
#55768=CARTESIAN_POINT('Ctrl Pts',(2.06501482580279E-14,-3.10942517663483,
-1.23575703823851));
#55769=CARTESIAN_POINT('Ctrl Pts',(1.8264438306287E-14,-3.08086824671493,
-1.33292965391417));
#55770=CARTESIAN_POINT('Ctrl Pts',(3.2855666700314E-14,-3.04796004332544,
-1.42892285724832));
#55771=CARTESIAN_POINT('Ctrl Pts',(3.14748227481232E-14,-3.0108994941223,
-1.52346659323359));
#55772=CARTESIAN_POINT('Ctrl Pts',(3.08707035190397E-14,-2.99468550384592,
-1.56482947772715));
#55773=CARTESIAN_POINT('Ctrl Pts',(-7.34111328475694E-15,-2.97767621882812,
-1.6059149164074));
#55774=CARTESIAN_POINT('Ctrl Pts',(-1.09356967925578E-14,-2.95988598833869,
-1.6467000642202));
#55775=CARTESIAN_POINT('Ctrl Pts',(-1.26060361330382E-14,-2.9516191830751,
-1.66565220060851));
#55776=CARTESIAN_POINT('Ctrl Pts',(-3.86060504933494E-15,-2.94318372929767,
-1.68453949171188));
#55777=CARTESIAN_POINT('Ctrl Pts',(-3.77475828372553E-15,-2.93458096810837,
-1.70335962248692));
#55778=CARTESIAN_POINT('Ctrl Pts',(-3.70222812974809E-15,-2.92731267338273,
-1.71926036112627));
#55779=CARTESIAN_POINT('Ctrl Pts',(2.66516022524014E-14,-2.91992517915329,
-1.73511249818651));
#55780=CARTESIAN_POINT('Ctrl Pts',(2.50910403565285E-14,-2.91242529539501,
-1.75090245665729));
#55781=CARTESIAN_POINT('Ctrl Pts',(1.51543221053757E-14,-2.86467055268367,
-1.85144340215677));
#55782=CARTESIAN_POINT('Ctrl Pts',(2.5322651512368E-14,-2.81230465551177,
-1.94959318469319));
#55783=CARTESIAN_POINT('Ctrl Pts',(2.07611705604904E-14,-2.75561827290968,
-2.04501777400763));
#55784=CARTESIAN_POINT('Ctrl Pts',(1.61277689467706E-14,-2.69803811870201,
-2.1419469184637));
#55785=CARTESIAN_POINT('Ctrl Pts',(-1.94004711555511E-15,-2.6359999497671,
-2.23606512208293));
#55786=CARTESIAN_POINT('Ctrl Pts',(-1.0325074129014E-14,-2.56975490805964,
-2.3270183027313));
#55787=CARTESIAN_POINT('Ctrl Pts',(-1.86902749150782E-14,-2.50366650141829,
-2.41775642641696));
#55788=CARTESIAN_POINT('Ctrl Pts',(9.81513156219114E-15,-2.4333907139672,
-2.50534535693934));
#55789=CARTESIAN_POINT('Ctrl Pts',(9.63118473862323E-15,-2.35912878838796,
-2.58941643446989));
#55790=CARTESIAN_POINT('Ctrl Pts',(9.51191154994316E-15,-2.31097652084914,
-2.64392906642701));
#55791=CARTESIAN_POINT('Ctrl Pts',(9.63185103010007E-15,-2.26114736965636,
-2.69696228592345));
#55792=CARTESIAN_POINT('Ctrl Pts',(6.13398221105399E-15,-2.20968648401442,
-2.7484090524039));
#55793=CARTESIAN_POINT('Ctrl Pts',(4.97169167218692E-15,-2.19258678599897,
-2.76550405882894));
#55794=CARTESIAN_POINT('Ctrl Pts',(-3.72567631824288E-14,-2.17530686341184,
-2.78242384826565));
#55795=CARTESIAN_POINT('Ctrl Pts',(-3.7997383017796E-14,-2.15784820071649,
-2.79916433054298));
#55796=CARTESIAN_POINT('Ctrl Pts',(-3.84779372019728E-14,-2.14652007661321,
-2.81002646036904));
#55797=CARTESIAN_POINT('Ctrl Pts',(-3.09033964280681E-14,-2.13511770191699,
-2.82081205931747));
#55798=CARTESIAN_POINT('Ctrl Pts',(-2.93098878501041E-14,-2.12365057671237,
-2.8315117956405));
#55799=CARTESIAN_POINT('Ctrl Pts',(-1.75398363148848E-14,-2.03895153179625,
-2.91054271500724));
#55800=CARTESIAN_POINT('Ctrl Pts',(1.391243074277E-14,-1.95059392907414,
-2.98501608956652));
#55801=CARTESIAN_POINT('Ctrl Pts',(9.18709552877317E-15,-1.85884286719316,
-3.0545692382486));
#55802=CARTESIAN_POINT('Ctrl Pts',(6.63646915186107E-15,-1.80931777152374,
-3.09211241510097));
#55803=CARTESIAN_POINT('Ctrl Pts',(2.81753841844117E-14,-1.75880310091069,
-3.12822176601201));
#55804=CARTESIAN_POINT('Ctrl Pts',(2.38420394538252E-14,-1.70733488200157,
-3.16283746139003));
#55805=CARTESIAN_POINT('Ctrl Pts',(1.6063726518083E-14,-1.61527957422441,
-3.22475059068581));
#55806=CARTESIAN_POINT('Ctrl Pts',(-3.24887086115797E-14,-1.52017596409272,
-3.28188798763151));
#55807=CARTESIAN_POINT('Ctrl Pts',(-4.33542091116124E-14,-1.42240896975834,
-3.33430526031992));
#55808=CARTESIAN_POINT('Ctrl Pts',(-5.44267912925744E-14,-1.32277866930879,
-3.38772153502743));
#55809=CARTESIAN_POINT('Ctrl Pts',(-1.70883232736321E-14,-1.2203818847999,
-3.43623635652515));
#55810=CARTESIAN_POINT('Ctrl Pts',(-1.76247905159244E-14,-1.11559232903488,
-3.47986607025536));
#55811=CARTESIAN_POINT('Ctrl Pts',(-1.77925080830662E-14,-1.08283161604207,
-3.49350617512115));
#55812=CARTESIAN_POINT('Ctrl Pts',(8.62866857219055E-15,-1.04983682877169,
-3.50666848552367));
#55813=CARTESIAN_POINT('Ctrl Pts',(1.26010313294955E-14,-1.01661888205787,
-3.51935259777105));
#55814=CARTESIAN_POINT('Ctrl Pts',(1.4439968170533E-14,-1.00124120642054,
-3.52522448881742));
#55815=CARTESIAN_POINT('Ctrl Pts',(2.40774351471501E-14,-0.985813515346819,
-3.5309946912081));
#55816=CARTESIAN_POINT('Ctrl Pts',(2.27873275804313E-14,-0.970343981558557,
-3.53666053934648));
#55817=CARTESIAN_POINT('Ctrl Pts',(1.38755660225048E-14,-0.863484057557096,
-3.57579889411256));
#55818=CARTESIAN_POINT('Ctrl Pts',(1.6643453337027E-15,-0.754890018819121,
-3.60986751842912));
#55819=CARTESIAN_POINT('Ctrl Pts',(2.4980018054066E-16,-0.644975218151253,
-3.63894883986376));
#55820=CARTESIAN_POINT('Ctrl Pts',(-1.21136733376833E-15,-0.531437707016576,
-3.66898866012576));
#55821=CARTESIAN_POINT('Ctrl Pts',(2.04532639396488E-14,-0.416490357224283,
-3.69370737857038));
#55822=CARTESIAN_POINT('Ctrl Pts',(1.52794443764037E-14,-0.300553728539226,
-3.71315269314144));
#55823=CARTESIAN_POINT('Ctrl Pts',(1.00530934138716E-14,-0.183439959202277,
-3.7327954420396));
#55824=CARTESIAN_POINT('Ctrl Pts',(2.21881067924296E-14,-0.0653159187698008,
-3.74705740395938));
#55825=CARTESIAN_POINT('Ctrl Pts',(2.41057174221737E-14,0.0534092998548874,
-3.75593991159167));
#55826=CARTESIAN_POINT('Ctrl Pts',(2.53745841684414E-14,0.131968773566364,
-3.76181739181798));
#55827=CARTESIAN_POINT('Ctrl Pts',(1.91130766186368E-14,0.210791949105575,
-3.76533856604393));
#55828=CARTESIAN_POINT('Ctrl Pts',(1.82215353916604E-14,0.289763421836197,
-3.7664916895623));
#55829=CARTESIAN_POINT('Ctrl Pts',(1.77888766373465E-14,0.328087728087114,
-3.76705129238259));
#55830=CARTESIAN_POINT('Ctrl Pts',(8.45263385617614E-15,0.366446982717185,
-3.76705304928818));
#55831=CARTESIAN_POINT('Ctrl Pts',(6.10622663543836E-15,0.404828064408706,
-3.76649476841554));
#55832=CARTESIAN_POINT('Ctrl Pts',(4.58792854474581E-15,0.429663447856183,
-3.76613351961972));
#55833=CARTESIAN_POINT('Ctrl Pts',(8.19568885810056E-16,0.454514571692306,
-3.7655374466664));
#55834=CARTESIAN_POINT('Ctrl Pts',(2.77555756156289E-16,0.479341903993956,
-3.76470733785867));
#55835=CARTESIAN_POINT('Ctrl Pts',(-2.39811010131796E-15,0.601902856371859,
-3.76060947809603));
#55836=CARTESIAN_POINT('Ctrl Pts',(-3.76428265862821E-15,0.724010931904768,
-3.75081338181991));
#55837=CARTESIAN_POINT('Ctrl Pts',(-2.49106291150269E-15,0.845225045914971,
-3.7353674895251));
#55838=CARTESIAN_POINT('Ctrl Pts',(-1.21608625440034E-15,0.966606422714429,
-3.71990028351573));
#55839=CARTESIAN_POINT('Ctrl Pts',(-6.83168379424844E-15,1.08709227080374,
-3.69876783461266));
#55840=CARTESIAN_POINT('Ctrl Pts',(-2.06085148946045E-14,1.20625519266052,
-3.67196862668376));
#55841=CARTESIAN_POINT('Ctrl Pts',(-3.43568694124192E-14,1.32517180585928,
-3.64522481246993));
#55842=CARTESIAN_POINT('Ctrl Pts',(-1.46458320159578E-14,1.442771871342,
-3.61283777782025));
#55843=CARTESIAN_POINT('Ctrl Pts',(-9.83241266183654E-15,1.5586324625958,
-3.57475395468793));
#55844=CARTESIAN_POINT('Ctrl Pts',(-5.01899330771531E-15,1.67449305384961,
-3.53667013155561));
#55845=CARTESIAN_POINT('Ctrl Pts',(-5.17908154171191E-16,1.78861510923313,
-3.49288968861999));
#55846=CARTESIAN_POINT('Ctrl Pts',(0.,1.90056365518826,-3.44330463255539));
#55847=CARTESIAN_POINT('Ctrl Pts',(0.,1.90056365518826,-3.44330463255539));
#55848=CARTESIAN_POINT('Ctrl Pts',(-0.0662911772324888,0.753200145251245,
-4.0766024725601));
#55849=CARTESIAN_POINT('Ctrl Pts',(-0.132582354464978,-0.725594898737993,
-4.08575984626747));
#55850=CARTESIAN_POINT('Ctrl Pts',(-0.198873531697467,-1.87121958628713,
-3.46643383696213));
#55851=CARTESIAN_POINT('Ctrl Pts',(-0.265164708929949,-3.01684427383614,
-2.84710782765686));
#55852=CARTESIAN_POINT('Ctrl Pts',(-0.331455886162431,-3.82929860494513,
-1.59929843533901));
#55853=CARTESIAN_POINT('Ctrl Pts',(-0.397747063394914,-3.92896721064676,
-0.298281141668419));
#55854=CARTESIAN_POINT('Ctrl Pts',(-0.402776868251713,-3.93652950864715,
-0.19956720452509));
#55855=CARTESIAN_POINT('Ctrl Pts',(-0.407806673108513,-3.93998835044424,
-0.100546953316975));
#55856=CARTESIAN_POINT('Ctrl Pts',(-0.412836477965312,-3.93946807025562,
-0.00149173430430305));
#55857=CARTESIAN_POINT('Origin',(4.677207419323,0.,0.));
#55858=CARTESIAN_POINT('',(4.53252091062694,6.5,-3.75277674973257));
#55859=CARTESIAN_POINT('',(4.53252091062694,-1.37874781034238E-15,-7.50555349946513));
#55860=CARTESIAN_POINT('Ctrl Pts',(4.53252091062694,6.5,-3.75277674973257));
#55861=CARTESIAN_POINT('Ctrl Pts',(5.61727242352805,3.24999999999854,-5.6291651245997));
#55862=CARTESIAN_POINT('Ctrl Pts',(4.53252091062694,-1.37874781034238E-15,
-7.50555349946513));
#55863=CARTESIAN_POINT('',(4.53252091062694,6.5,3.75277674973257));
#55864=CARTESIAN_POINT('Ctrl Pts',(4.53252091062694,6.5,3.75277674973257));
#55865=CARTESIAN_POINT('Ctrl Pts',(5.61727242352805,6.5,-1.69086966650411E-12));
#55866=CARTESIAN_POINT('Ctrl Pts',(4.53252091062694,6.5,-3.75277674973257));
#55867=CARTESIAN_POINT('',(4.53252091062694,4.5958260344746E-16,7.50555349946513));
#55868=CARTESIAN_POINT('Ctrl Pts',(4.53252091062694,4.5958260344746E-16,
7.50555349946513));
#55869=CARTESIAN_POINT('Ctrl Pts',(5.61727242352806,3.25000000000146,5.62916512459801));
#55870=CARTESIAN_POINT('Ctrl Pts',(4.53252091062694,6.5,3.75277674973257));
#55871=CARTESIAN_POINT('',(4.53252091062694,-6.5,3.75277674973257));
#55872=CARTESIAN_POINT('Ctrl Pts',(4.53252091062694,-6.5,3.75277674973257));
#55873=CARTESIAN_POINT('Ctrl Pts',(5.61727242352806,-3.24999999999854,5.6291651245997));
#55874=CARTESIAN_POINT('Ctrl Pts',(4.53252091062694,4.5958260344746E-16,
7.50555349946513));
#55875=CARTESIAN_POINT('',(5.11383749436743,-6.5,-8.18813977659918E-16));
#55876=CARTESIAN_POINT('Ctrl Pts',(5.11383749436743,-6.5,-8.41607535874056E-16));
#55877=CARTESIAN_POINT('Ctrl Pts',(5.11383749436757,-6.5,1.74166975080303));
#55878=CARTESIAN_POINT('Ctrl Pts',(4.53252091062694,-6.5,3.75277674973257));
#55879=CARTESIAN_POINT('',(5.3,-6.17797863635533,-7.56584176221328E-16));
#55880=CARTESIAN_POINT('',(4.677207419323,-7.25527674973257,-8.8851514484882E-16));
#55881=CARTESIAN_POINT('Origin',(5.3,0.,0.));
#55882=CARTESIAN_POINT('',(4.53252091062694,-6.5,-3.75277674973257));
#55883=CARTESIAN_POINT('Ctrl Pts',(4.53252091062694,-6.5,-3.75277674973257));
#55884=CARTESIAN_POINT('Ctrl Pts',(5.11383749436729,-6.5,-1.74166975080219));
#55885=CARTESIAN_POINT('Ctrl Pts',(5.11383749436743,-6.5,-8.41607535874056E-16));
#55886=CARTESIAN_POINT('Ctrl Pts',(4.53252091062694,-1.37874781034238E-15,
-7.50555349946513));
#55887=CARTESIAN_POINT('Ctrl Pts',(5.61727242352805,-3.25000000000146,-5.629165124598));
#55888=CARTESIAN_POINT('Ctrl Pts',(4.53252091062694,-6.5,-3.75277674973257));
#55889=CARTESIAN_POINT('Origin',(0.,4.5958260344746E-16,7.50555349946513));
#55890=CARTESIAN_POINT('',(0.,4.5958260344746E-16,7.50555349946513));
#55891=CARTESIAN_POINT('',(0.,4.5958260344746E-16,7.50555349946513));
#55892=CARTESIAN_POINT('',(0.,-6.5,3.75277674973257));
#55893=CARTESIAN_POINT('',(0.,4.5958260344746E-16,7.50555349946513));
#55894=CARTESIAN_POINT('',(0.,-6.5,3.75277674973257));
#55895=CARTESIAN_POINT('Origin',(0.,6.5,3.75277674973257));
#55896=CARTESIAN_POINT('',(0.,6.5,3.75277674973257));
#55897=CARTESIAN_POINT('',(0.,6.5,3.75277674973257));
#55898=CARTESIAN_POINT('',(0.,6.5,3.75277674973257));
#55899=CARTESIAN_POINT('Origin',(0.,6.5,-3.75277674973257));
#55900=CARTESIAN_POINT('',(0.,6.5,-3.75277674973257));
#55901=CARTESIAN_POINT('',(0.,6.5,-3.75277674973257));
#55902=CARTESIAN_POINT('',(0.,6.5,-3.75277674973257));
#55903=CARTESIAN_POINT('Origin',(0.,0.,-1.11022302462516E-15));
#55904=CARTESIAN_POINT('',(0.,-1.37874781034238E-15,-7.50555349946513));
#55905=CARTESIAN_POINT('',(0.,-1.37874781034238E-15,-7.50555349946513));
#55906=CARTESIAN_POINT('',(0.,-6.5,-3.75277674973257));
#55907=CARTESIAN_POINT('',(0.,-6.5,-3.75277674973257));
#55908=CARTESIAN_POINT('',(0.,-6.5,3.75277674973257));
#55909=CARTESIAN_POINT('Origin',(0.,0.,0.));
#55910=CARTESIAN_POINT('Origin',(0.,-1.37874781034238E-15,-7.50555349946513));
#55911=CARTESIAN_POINT('',(0.,-1.37874781034238E-15,-7.50555349946513));
#55912=CARTESIAN_POINT('Origin',(0.,-6.5,-3.75277674973257));
#55913=CARTESIAN_POINT('',(0.,-6.5,-3.75277674973257));
#55914=CARTESIAN_POINT('Origin',(0.,-6.5,3.75277674973257));
#55915=CARTESIAN_POINT('Origin',(5.3,0.,-1.11022302462516E-15));
#55916=CARTESIAN_POINT('Origin',(-110.,3.5,0.));
#55917=CARTESIAN_POINT('',(-110.,-3.5,-4.28626379701574E-16));
#55918=CARTESIAN_POINT('Origin',(-110.,0.,0.));
#55919=CARTESIAN_POINT('Origin',(-109.75,0.,0.));
#55920=CARTESIAN_POINT('',(-109.75,-3.75,-4.59242549680257E-16));
#55921=CARTESIAN_POINT('Origin',(-54.75,0.,0.));
#55922=CARTESIAN_POINT('',(0.,0.,0.));
#55923=CARTESIAN_POINT('Origin',(6.73243375990795,0.,-1.96302583630813E-16));
#55924=CARTESIAN_POINT('',(6.8,-5.90797863635533,7.23518712644349E-16));
#55925=CARTESIAN_POINT('Origin',(6.8,0.,0.));
#55926=CARTESIAN_POINT('',(6.69652890400909,-6.29699688036588,-0.000745309284438215));
#55927=CARTESIAN_POINT('',(6.73243375990795,-6.15985379710312,-1.14696969084543E-15));
#55928=CARTESIAN_POINT('',(6.66502947251616,-6.26458164591552,-1.36312261022737));
#55929=CARTESIAN_POINT('Ctrl Pts',(6.69652890400909,-6.29699688036588,-0.000745309284438218));
#55930=CARTESIAN_POINT('Ctrl Pts',(6.69636098644092,-6.29700262112883,-0.0492132156999537));
#55931=CARTESIAN_POINT('Ctrl Pts',(6.69608278371896,-6.29688319686096,-0.0976832249692937));
#55932=CARTESIAN_POINT('Ctrl Pts',(6.69569933387107,-6.29663841314834,-0.146165083532695));
#55933=CARTESIAN_POINT('Ctrl Pts',(6.69481798076397,-6.29607578185022,-0.257599830262322));
#55934=CARTESIAN_POINT('Ctrl Pts',(6.69338166738899,-6.29485127594458,-0.368971942752256));
#55935=CARTESIAN_POINT('Ctrl Pts',(6.69145929669846,-6.29296756829865,-0.480391711796666));
#55936=CARTESIAN_POINT('Ctrl Pts',(6.69067207967973,-6.2921961839218,-0.526018467783933));
#55937=CARTESIAN_POINT('Ctrl Pts',(6.68980345947523,-6.29131421828673,-0.571653020364473));
#55938=CARTESIAN_POINT('Ctrl Pts',(6.68884893267613,-6.29032205090899,-0.61730213483034));
#55939=CARTESIAN_POINT('Ctrl Pts',(6.68640701890517,-6.28778384330171,-0.734083770874912));
#55940=CARTESIAN_POINT('Ctrl Pts',(6.68340625854999,-6.284527919109,-0.850780859498688));
#55941=CARTESIAN_POINT('Ctrl Pts',(6.67978096417448,-6.28057025686126,-0.967522815650963));
#55942=CARTESIAN_POINT('Ctrl Pts',(6.67633867912469,-6.27681238227884,-1.07837149405382));
#55943=CARTESIAN_POINT('Ctrl Pts',(6.6723331936121,-6.27242175564932,-1.18926081995884));
#55944=CARTESIAN_POINT('Ctrl Pts',(6.66772997716308,-6.26741032190845,-1.30025872695154));
#55945=CARTESIAN_POINT('Ctrl Pts',(6.66688688033845,-6.26649245851432,-1.32058842119099));
#55946=CARTESIAN_POINT('Ctrl Pts',(6.66602379657714,-6.26555376669622,-1.34092163259341));
#55947=CARTESIAN_POINT('Ctrl Pts',(6.66514060252649,-6.26459431597002,-1.36125860576499));
#55948=CARTESIAN_POINT('',(6.66836161846084,-4.31130259409624,-4.74443759007071));
#55949=CARTESIAN_POINT('Origin',(6.6648675198159,0.,-3.92605167261626E-16));
#55950=CARTESIAN_POINT('',(6.66503408817778,-1.95314743508685,-6.10607994622927));
#55951=CARTESIAN_POINT('Ctrl Pts',(6.66935871145732,-4.31020955205977,-4.74503293761719));
#55952=CARTESIAN_POINT('Ctrl Pts',(6.67436042918073,-4.21520368992507,-4.80602391498316));
#55953=CARTESIAN_POINT('Ctrl Pts',(6.67866531126362,-4.11997191868513,-4.86641425169366));
#55954=CARTESIAN_POINT('Ctrl Pts',(6.68227076873634,-4.02444968243747,-4.92622621540924));
#55955=CARTESIAN_POINT('Ctrl Pts',(6.68468558542453,-3.96047203412808,-4.96628629910921));
#55956=CARTESIAN_POINT('Ctrl Pts',(6.68678714553132,-3.89636312663956,-5.00608746781467));
#55957=CARTESIAN_POINT('Ctrl Pts',(6.68858007739062,-3.83209320725026,-5.04564199838796));
#55958=CARTESIAN_POINT('Ctrl Pts',(6.69153748848899,-3.72608105073249,-5.11088653464953));
#55959=CARTESIAN_POINT('Ctrl Pts',(6.69364912704048,-3.61978338152845,-5.17536640559943));
#55960=CARTESIAN_POINT('Ctrl Pts',(6.69495610000005,-3.51307967515119,-5.23914030618921));
#55961=CARTESIAN_POINT('Ctrl Pts',(6.69547972661654,-3.47032982303817,-5.26469072905122));
#55962=CARTESIAN_POINT('Ctrl Pts',(6.69587456241581,-3.42751433350044,-5.29012805821525));
#55963=CARTESIAN_POINT('Ctrl Pts',(6.69614463629548,-3.38462385382883,-5.3154568011996));
#55964=CARTESIAN_POINT('Ctrl Pts',(6.69690336884412,-3.26412940618645,-5.38661415170591));
#55965=CARTESIAN_POINT('Ctrl Pts',(6.69667276210013,-3.14322205465598,-5.45680979375134));
#55966=CARTESIAN_POINT('Ctrl Pts',(6.69556561628492,-3.02171103015008,-5.52614860785243));
#55967=CARTESIAN_POINT('Ctrl Pts',(6.69468374538135,-2.92492428760768,-5.58137880590142));
#55968=CARTESIAN_POINT('Ctrl Pts',(6.69324805633593,-2.82786106051647,-5.63600435237614));
#55969=CARTESIAN_POINT('Ctrl Pts',(6.69132764292846,-2.73042720868452,-5.69008268017868));
#55970=CARTESIAN_POINT('Ctrl Pts',(6.69054122742349,-2.69052773105539,-5.71222793041573));
#55971=CARTESIAN_POINT('Ctrl Pts',(6.68967363179484,-2.65056625226925,-5.73428128569138));
#55972=CARTESIAN_POINT('Ctrl Pts',(6.6887203269053,-2.61053709848336,-5.75624646027473));
#55973=CARTESIAN_POINT('Ctrl Pts',(6.68628167961823,-2.50813860209913,-5.81243552842698));
#55974=CARTESIAN_POINT('Ctrl Pts',(6.68328553552123,-2.40545474077465,-5.86796068128634));
#55975=CARTESIAN_POINT('Ctrl Pts',(6.6796657811188,-2.30238136543676,-5.92290049980573));
#55976=CARTESIAN_POINT('Ctrl Pts',(6.67622882675131,-2.20451326496543,-5.97506582049214));
#55977=CARTESIAN_POINT('Ctrl Pts',(6.67222952719711,-2.10629379186944,-6.02670346636737));
#55978=CARTESIAN_POINT('Ctrl Pts',(6.66763300366906,-2.0076700314861,-6.07785777969868));
#55979=CARTESIAN_POINT('Ctrl Pts',(6.66679042891553,-1.98959160980734,-6.0872347213555));
#55980=CARTESIAN_POINT('Ctrl Pts',(6.6659278508756,-1.9714997104692,-6.09659535683047));
#55981=CARTESIAN_POINT('Ctrl Pts',(6.66504514382671,-1.95339415559984,-6.10593986928562));
#55982=CARTESIAN_POINT('',(6.66503408817778,1.95314743508651,-6.10607994622938));
#55983=CARTESIAN_POINT('Origin',(6.6648675198159,0.,-3.92605167261626E-16));
#55984=CARTESIAN_POINT('',(6.6683616184638,4.31130259409795,-4.74443759006966));
#55985=CARTESIAN_POINT('Ctrl Pts',(6.66504514382671,1.95339415559952,-6.10593986928573));
#55986=CARTESIAN_POINT('Ctrl Pts',(6.66991331462735,2.05324714040973,-6.05440444455141));
#55987=CARTESIAN_POINT('Ctrl Pts',(6.67416697695882,2.15269731478132,-6.00237315124276));
#55988=CARTESIAN_POINT('Ctrl Pts',(6.67783901815979,2.25179789322377,-5.94979970935148));
#55989=CARTESIAN_POINT('Ctrl Pts',(6.68032354309352,2.3188499344761,-5.91422820563398));
#55990=CARTESIAN_POINT('Ctrl Pts',(6.68254235212595,2.38574287168437,-5.87840794797414));
#55991=CARTESIAN_POINT('Ctrl Pts',(6.68451150443652,2.45250341609415,-5.84231823937542));
#55992=CARTESIAN_POINT('Ctrl Pts',(6.68725425988621,2.54549157451221,-5.79205029189074));
#55993=CARTESIAN_POINT('Ctrl Pts',(6.68950868260796,2.63811000348344,-5.74132073890011));
#55994=CARTESIAN_POINT('Ctrl Pts',(6.6913278663153,2.730427135972,-5.69008257296905));
#55995=CARTESIAN_POINT('Ctrl Pts',(6.69250789027921,2.79030917437,-5.65684664224831));
#55996=CARTESIAN_POINT('Ctrl Pts',(6.69350522572667,2.85006491766445,-5.62339639406913));
#55997=CARTESIAN_POINT('Ctrl Pts',(6.69430363820578,2.90971680597308,-5.58971757209521));
#55998=CARTESIAN_POINT('Ctrl Pts',(6.69593435114067,3.03155245909875,-5.52093045758735));
#55999=CARTESIAN_POINT('Ctrl Pts',(6.69672978737442,3.15277519167217,-5.45129218342463));
#56000=CARTESIAN_POINT('Ctrl Pts',(6.69656720749179,3.27357451204812,-5.38069560740119));
#56001=CARTESIAN_POINT('Ctrl Pts',(6.69641551950675,3.38628098720044,-5.31482858748203));
#56002=CARTESIAN_POINT('Ctrl Pts',(6.69543013844524,3.49847401422254,-5.24821175049788));
#56003=CARTESIAN_POINT('Ctrl Pts',(6.69353943304081,3.61030941318271,-5.18076617701774));
#56004=CARTESIAN_POINT('Ctrl Pts',(6.69315501085506,3.63304802090655,-5.16705300165168));
#56005=CARTESIAN_POINT('Ctrl Pts',(6.69273328275894,3.65577173256785,-5.1533056124498));
#56006=CARTESIAN_POINT('Ctrl Pts',(6.6922738380125,3.67848166516312,-5.13952343023613));
#56007=CARTESIAN_POINT('Ctrl Pts',(6.6902506558864,3.77848570279241,-5.07883307534723));
#56008=CARTESIAN_POINT('Ctrl Pts',(6.68749862281492,3.87806838929537,-5.01756113610782));
#56009=CARTESIAN_POINT('Ctrl Pts',(6.68399280879373,3.97734644961371,-4.95565755544302));
#56010=CARTESIAN_POINT('Ctrl Pts',(6.68065299539626,4.07192368443615,-4.89668511514642));
#56011=CARTESIAN_POINT('Ctrl Pts',(6.67662905286536,4.16622462203365,-4.83713926971924));
#56012=CARTESIAN_POINT('Ctrl Pts',(6.6719206958442,4.26031186570891,-4.77699710220824));
#56013=CARTESIAN_POINT('Ctrl Pts',(6.67108802535535,4.27695114578758,-4.76636099118337));
#56014=CARTESIAN_POINT('Ctrl Pts',(6.67023400615726,4.29358363828582,-4.75570628669163));
#56015=CARTESIAN_POINT('Ctrl Pts',(6.66935871145733,4.31020955205948,-4.74503293761744));
#56016=CARTESIAN_POINT('',(6.66844118715618,6.2644530578692,-1.36147101261479));
#56017=CARTESIAN_POINT('Origin',(6.6648675198159,0.,-3.92605167261626E-16));
#56018=CARTESIAN_POINT('',(6.66512518996691,6.26459255876718,1.3615171235111));
#56019=CARTESIAN_POINT('Ctrl Pts',(6.66943768476099,6.26442235049373,-1.36025300281069));
#56020=CARTESIAN_POINT('Ctrl Pts',(6.67444551486767,6.26973920227163,-1.24747868336829));
#56021=CARTESIAN_POINT('Ctrl Pts',(6.67875641270276,6.27442290417064,-1.13480902487606));
#56022=CARTESIAN_POINT('Ctrl Pts',(6.682367556141,6.27846046253376,-1.02217693285355));
#56023=CARTESIAN_POINT('Ctrl Pts',(6.68478603761825,6.28116452574297,-0.94674414183892));
#56024=CARTESIAN_POINT('Ctrl Pts',(6.68689115132044,6.28357875541318,-0.871327101016574));
#56025=CARTESIAN_POINT('Ctrl Pts',(6.68868745028096,6.28569890792413,-0.795893893215038));
#56026=CARTESIAN_POINT('Ctrl Pts',(6.69165049748906,6.28919616095181,-0.67146463022138));
#56027=CARTESIAN_POINT('Ctrl Pts',(6.6937672098887,6.29188845823143,-0.547170307559333));
#56028=CARTESIAN_POINT('Ctrl Pts',(6.69507834981273,6.2937663704627,-0.422877132573859));
#56029=CARTESIAN_POINT('Ctrl Pts',(6.69560366022879,6.29451875915703,-0.373078862939984));
#56030=CARTESIAN_POINT('Ctrl Pts',(6.69600002716747,6.29514038349348,-0.323280264512499));
#56031=CARTESIAN_POINT('Ctrl Pts',(6.6962714577742,6.29563047084122,-0.273470978596723));
#56032=CARTESIAN_POINT('Ctrl Pts',(6.69703398698074,6.29700727178824,-0.133541897922291));
#56033=CARTESIAN_POINT('Ctrl Pts',(6.69680582961814,6.29734476924276,0.00626420573700309));
#56034=CARTESIAN_POINT('Ctrl Pts',(6.69569933387107,6.29663841314834,0.146165083532808));
#56035=CARTESIAN_POINT('Ctrl Pts',(6.69481798076397,6.29607578185022,0.257599830262394));
#56036=CARTESIAN_POINT('Ctrl Pts',(6.69338166738899,6.29485127594458,0.368971942752287));
#56037=CARTESIAN_POINT('Ctrl Pts',(6.69145929669845,6.29296756829865,0.480391711796661));
#56038=CARTESIAN_POINT('Ctrl Pts',(6.69067207967973,6.2921961839218,0.526018467783964));
#56039=CARTESIAN_POINT('Ctrl Pts',(6.68980345947522,6.29131421828673,0.57165302036454));
#56040=CARTESIAN_POINT('Ctrl Pts',(6.68884893267613,6.29032205090899,0.617302134830443));
#56041=CARTESIAN_POINT('Ctrl Pts',(6.68640701890508,6.28778384330163,0.734083770878798));
#56042=CARTESIAN_POINT('Ctrl Pts',(6.68340625854979,6.28452791910879,0.850780859506348));
#56043=CARTESIAN_POINT('Ctrl Pts',(6.67978096417412,6.28057025686087,0.967522815662406));
#56044=CARTESIAN_POINT('Ctrl Pts',(6.67633867912425,6.27681238227837,1.07837149406654));
#56045=CARTESIAN_POINT('Ctrl Pts',(6.67233319361156,6.27242175564875,1.18926081997286));
#56046=CARTESIAN_POINT('Ctrl Pts',(6.66772997716244,6.26741032190776,1.30025872696685));
#56047=CARTESIAN_POINT('Ctrl Pts',(6.66688688033801,6.26649245851385,1.32058842120122));
#56048=CARTESIAN_POINT('Ctrl Pts',(6.66602379657691,6.26555376669599,1.34092163259858));
#56049=CARTESIAN_POINT('Ctrl Pts',(6.66514060252648,6.26459431597002,1.36125860576509));
#56050=CARTESIAN_POINT('',(6.66836161846091,4.3113025940965,4.74443759007056));
#56051=CARTESIAN_POINT('Origin',(6.6648675198159,0.,-3.92605167261626E-16));
#56052=CARTESIAN_POINT('',(6.66503408817681,1.95314743508669,6.10607994622942));
#56053=CARTESIAN_POINT('Ctrl Pts',(6.66935871145727,4.31020955206015,4.74503293761698));
#56054=CARTESIAN_POINT('Ctrl Pts',(6.67436042918074,4.21520368992431,4.80602391498368));
#56055=CARTESIAN_POINT('Ctrl Pts',(6.67866531126367,4.11997191868325,4.86641425169488));
#56056=CARTESIAN_POINT('Ctrl Pts',(6.68227076873642,4.02444968243447,4.92622621541114));
#56057=CARTESIAN_POINT('Ctrl Pts',(6.68468558542457,3.96047203412598,4.96628629911054));
#56058=CARTESIAN_POINT('Ctrl Pts',(6.68678714553132,3.89636312663836,5.00608746781543));
#56059=CARTESIAN_POINT('Ctrl Pts',(6.68858007739059,3.83209320724997,5.04564199838816));
#56060=CARTESIAN_POINT('Ctrl Pts',(6.691537488489,3.72608105073089,5.11088653465053));
#56061=CARTESIAN_POINT('Ctrl Pts',(6.6936491270405,3.61978338152556,5.17536640560121));
#56062=CARTESIAN_POINT('Ctrl Pts',(6.69495610000006,3.51307967514701,5.23914030619173));
#56063=CARTESIAN_POINT('Ctrl Pts',(6.69547972661653,3.47032982303531,5.26469072905295));
#56064=CARTESIAN_POINT('Ctrl Pts',(6.69587456241578,3.4275143334989,5.29012805821618));
#56065=CARTESIAN_POINT('Ctrl Pts',(6.69614463629545,3.38462385382863,5.31545680119975));
#56066=CARTESIAN_POINT('Ctrl Pts',(6.69690336884408,3.26412940618622,5.38661415170606));
#56067=CARTESIAN_POINT('Ctrl Pts',(6.69667276210009,3.14322205465577,5.45680979375149));
#56068=CARTESIAN_POINT('Ctrl Pts',(6.69556561628488,3.02171103014988,5.52614860785257));
#56069=CARTESIAN_POINT('Ctrl Pts',(6.69468374538131,2.92492428760756,5.58137880590151));
#56070=CARTESIAN_POINT('Ctrl Pts',(6.69324805633589,2.82786106051644,5.63600435237619));
#56071=CARTESIAN_POINT('Ctrl Pts',(6.69132764292842,2.73042720868454,5.6900826801787));
#56072=CARTESIAN_POINT('Ctrl Pts',(6.69054122742345,2.69052773105532,5.71222793041579));
#56073=CARTESIAN_POINT('Ctrl Pts',(6.68967363179479,2.65056625226909,5.73428128569149));
#56074=CARTESIAN_POINT('Ctrl Pts',(6.68872032690526,2.61053709848311,5.7562464602749));
#56075=CARTESIAN_POINT('Ctrl Pts',(6.68628167961827,2.50813860210269,5.81243552842505));
#56076=CARTESIAN_POINT('Ctrl Pts',(6.68328553552141,2.40545474078205,5.86796068128236));
#56077=CARTESIAN_POINT('Ctrl Pts',(6.67966578111915,2.30238136544803,5.92290049979975));
#56078=CARTESIAN_POINT('Ctrl Pts',(6.6762288267517,2.20451326497631,5.97506582048642));
#56079=CARTESIAN_POINT('Ctrl Pts',(6.67222952719752,2.10629379187994,6.0267034663619));
#56080=CARTESIAN_POINT('Ctrl Pts',(6.66763300366949,2.0076700314962,6.07785777969347));
#56081=CARTESIAN_POINT('Ctrl Pts',(6.66679042891581,1.98959160981393,6.08723472135212));
#56082=CARTESIAN_POINT('Ctrl Pts',(6.66592785087571,1.97149971047227,6.09659535682891));
#56083=CARTESIAN_POINT('Ctrl Pts',(6.66504514382665,1.95339415559939,6.10593986928588));
#56084=CARTESIAN_POINT('',(6.66503408817771,-1.95314743508628,6.10607994622951));
#56085=CARTESIAN_POINT('Origin',(6.6648675198159,0.,-3.92605167261626E-16));
#56086=CARTESIAN_POINT('',(6.66836161846092,-4.31130259409623,4.7444375900708));
#56087=CARTESIAN_POINT('Ctrl Pts',(6.66504514382665,-1.95339415559905,6.105939869286));
#56088=CARTESIAN_POINT('Ctrl Pts',(6.6699133146273,-2.05324714040958,6.05440444455152));
#56089=CARTESIAN_POINT('Ctrl Pts',(6.67416697695878,-2.15269731478148,6.00237315124271));
#56090=CARTESIAN_POINT('Ctrl Pts',(6.67783901815976,-2.25179789322423,5.94979970935126));
#56091=CARTESIAN_POINT('Ctrl Pts',(6.6803235430935,-2.31884993447649,5.9142282056338));
#56092=CARTESIAN_POINT('Ctrl Pts',(6.68254235212591,-2.38574287168466,5.87840794797402));
#56093=CARTESIAN_POINT('Ctrl Pts',(6.68451150443648,-2.45250341609436,5.84231823937534));
#56094=CARTESIAN_POINT('Ctrl Pts',(6.68725425988618,-2.54549157451238,5.79205029189068));
#56095=CARTESIAN_POINT('Ctrl Pts',(6.68950868260793,-2.63811000348354,5.74132073890009));
#56096=CARTESIAN_POINT('Ctrl Pts',(6.69132786631526,-2.73042713597201,5.69008257296907));
#56097=CARTESIAN_POINT('Ctrl Pts',(6.69250789027917,-2.79030917437005,5.65684664224831));
#56098=CARTESIAN_POINT('Ctrl Pts',(6.69350522572663,-2.85006491766454,5.62339639406911));
#56099=CARTESIAN_POINT('Ctrl Pts',(6.69430363820574,-2.9097168059732,5.58971757209517));
#56100=CARTESIAN_POINT('Ctrl Pts',(6.69593435114063,-3.03155245909877,5.52093045758737));
#56101=CARTESIAN_POINT('Ctrl Pts',(6.69672978737438,-3.15277519167224,5.45129218342462));
#56102=CARTESIAN_POINT('Ctrl Pts',(6.69656720749175,-3.27357451204824,5.38069560740115));
#56103=CARTESIAN_POINT('Ctrl Pts',(6.69641551950671,-3.38628098720265,5.31482858748076));
#56104=CARTESIAN_POINT('Ctrl Pts',(6.69543013844517,-3.49847401422682,5.24821175049536));
#56105=CARTESIAN_POINT('Ctrl Pts',(6.69353943304067,-3.61030941318907,5.18076617701393));
#56106=CARTESIAN_POINT('Ctrl Pts',(6.69315501085495,-3.63304802091084,5.16705300164911));
#56107=CARTESIAN_POINT('Ctrl Pts',(6.69273328275886,-3.65577173257007,5.15330561244848));
#56108=CARTESIAN_POINT('Ctrl Pts',(6.69227383801246,-3.67848166516327,5.13952343023606));
#56109=CARTESIAN_POINT('Ctrl Pts',(6.69025065588632,-3.77848570279493,5.07883307534573));
#56110=CARTESIAN_POINT('Ctrl Pts',(6.68749862281475,-3.87806838930023,5.01756113610486));
#56111=CARTESIAN_POINT('Ctrl Pts',(6.68399280879344,-3.97734644962088,4.95565755543857));
#56112=CARTESIAN_POINT('Ctrl Pts',(6.68065299539596,-4.07192368444291,4.89668511514219));
#56113=CARTESIAN_POINT('Ctrl Pts',(6.67662905286504,-4.16622462203999,4.83713926971524));
#56114=CARTESIAN_POINT('Ctrl Pts',(6.67192069584387,-4.26031186571482,4.77699710220449));
#56115=CARTESIAN_POINT('Ctrl Pts',(6.67108802535511,-4.27695114579165,4.76636099118079));
#56116=CARTESIAN_POINT('Ctrl Pts',(6.67023400615712,-4.29358363828805,4.75570628669022));
#56117=CARTESIAN_POINT('Ctrl Pts',(6.66935871145727,-4.31020955205987,4.74503293761721));
#56118=CARTESIAN_POINT('',(6.6684411871562,-6.2644530578692,1.36147101261486));
#56119=CARTESIAN_POINT('Origin',(6.6648675198159,0.,-3.92605167261626E-16));
#56120=CARTESIAN_POINT('Ctrl Pts',(6.66943768476097,-6.26442235049373,1.36025300281079));
#56121=CARTESIAN_POINT('Ctrl Pts',(6.67444551486759,-6.26973920227156,1.2474786833699));
#56122=CARTESIAN_POINT('Ctrl Pts',(6.67875641270264,-6.27442290417052,1.13480902487915));
#56123=CARTESIAN_POINT('Ctrl Pts',(6.68236755614085,-6.2784604625336,1.02217693285811));
#56124=CARTESIAN_POINT('Ctrl Pts',(6.68478603761816,-6.28116452574288,0.946744141841997));
#56125=CARTESIAN_POINT('Ctrl Pts',(6.68689115132039,-6.28357875541314,0.871327101018171));
#56126=CARTESIAN_POINT('Ctrl Pts',(6.68868745028095,-6.28569890792413,0.79589389321515));
#56127=CARTESIAN_POINT('Ctrl Pts',(6.69165049748917,-6.28919616095194,0.671464630216681));
#56128=CARTESIAN_POINT('Ctrl Pts',(6.69376720988886,-6.29188845823163,0.547170307549914));
#56129=CARTESIAN_POINT('Ctrl Pts',(6.69507834981288,-6.29376637046291,0.422877132559733));
#56130=CARTESIAN_POINT('Ctrl Pts',(6.69560366022886,-6.29451875915715,0.373078862930602));
#56131=CARTESIAN_POINT('Ctrl Pts',(6.69600002716749,-6.29514038349353,0.323280264507863));
#56132=CARTESIAN_POINT('Ctrl Pts',(6.6962714577742,-6.29563047084122,0.273470978596836));
#56133=CARTESIAN_POINT('Ctrl Pts',(6.69676973994398,-6.29653015488919,0.182032951914047));
#56134=CARTESIAN_POINT('Ctrl Pts',(6.69684570354175,-6.29698595925452,0.0906480036726336));
#56135=CARTESIAN_POINT('Ctrl Pts',(6.69652890400909,-6.29699688036588,-0.000745309284438218));
#56136=CARTESIAN_POINT('Ctrl Pts',(5.82127992530897,0.211713211864508,7.38332081960416));
#56137=CARTESIAN_POINT('Ctrl Pts',(6.14241820370575,1.20871426115459,6.80770199541419));
#56138=CARTESIAN_POINT('Ctrl Pts',(6.49215447047434,3.14708040407219,5.68858578101266));
#56139=CARTESIAN_POINT('Ctrl Pts',(6.2494642965047,4.95895205574989,4.64250119517949));
#56140=CARTESIAN_POINT('Ctrl Pts',(5.82127992530902,6.28828678813546,3.87500942959356));
#56141=CARTESIAN_POINT('Ctrl Pts',(5.94576262842914,0.141142141243011,7.33053715581116));
#56142=CARTESIAN_POINT('Ctrl Pts',(6.27212071493947,1.14515484589772,6.75259524852742));
#56143=CARTESIAN_POINT('Ctrl Pts',(6.63166480681812,3.1065235293192,5.62357322350997));
#56144=CARTESIAN_POINT('Ctrl Pts',(6.38090674377616,4.94116869510222,4.56154066351441));
#56145=CARTESIAN_POINT('Ctrl Pts',(5.94576262842917,6.27786032969667,3.78750125776656));
#56146=CARTESIAN_POINT('Ctrl Pts',(6.07024533154931,0.0705710706215141,
7.27775349201815));
#56147=CARTESIAN_POINT('Ctrl Pts',(6.40182322617319,1.08159543064085,6.69748850164065));
#56148=CARTESIAN_POINT('Ctrl Pts',(6.7711751431619,3.06596665456621,5.55856066600728));
#56149=CARTESIAN_POINT('Ctrl Pts',(6.51234919104763,4.92338533445454,4.48058013184934));
#56150=CARTESIAN_POINT('Ctrl Pts',(6.07024533154933,6.26743387125788,3.69999308593956));
#56151=CARTESIAN_POINT('Ctrl Pts',(6.19472803466948,1.72084568816899E-14,
7.22496982822515));
#56152=CARTESIAN_POINT('Ctrl Pts',(6.53152573740691,1.01803601538398,6.64238175475387));
#56153=CARTESIAN_POINT('Ctrl Pts',(6.91068547950568,3.02540977981322,5.49354810850458));
#56154=CARTESIAN_POINT('Ctrl Pts',(6.64379163831909,4.90560197380687,4.39961960018427));
#56155=CARTESIAN_POINT('Ctrl Pts',(6.19472803466948,6.25700741281908,3.61248491411256));
#56156=CARTESIAN_POINT('',(6.19472803466948,6.25700741281908,3.61248491411256));
#56157=CARTESIAN_POINT('Ctrl Pts',(6.66935871145421,4.31020955208199,4.7450329376043));
#56158=CARTESIAN_POINT('Ctrl Pts',(6.58472768457026,4.91347707050904,4.39484321142667));
#56159=CARTESIAN_POINT('Ctrl Pts',(6.43065501953876,5.54701219617073,4.02602614003615));
#56160=CARTESIAN_POINT('Ctrl Pts',(6.19472803466948,6.25700741281908,3.61248491411256));
#56161=CARTESIAN_POINT('',(5.82838302289405,6.26617314097884,3.8877767497322));
#56162=CARTESIAN_POINT('Ctrl Pts',(5.82838302289405,6.26617314097884,3.8877767497322));
#56163=CARTESIAN_POINT('Ctrl Pts',(5.88949356894947,6.26458780816846,3.84195257738004));
#56164=CARTESIAN_POINT('Ctrl Pts',(5.95058218580133,6.26303119380756,3.7960960923254));
#56165=CARTESIAN_POINT('Ctrl Pts',(6.07269657345126,6.25997595306932,3.70433263349585));
#56166=CARTESIAN_POINT('Ctrl Pts',(6.13372433579515,6.25847726314342,3.65842418692963));
#56167=CARTESIAN_POINT('Ctrl Pts',(6.19472803466948,6.25700741281908,3.61248491411256));
#56168=CARTESIAN_POINT('',(5.82838302289383,0.233826859021799,7.37055349946514));
#56169=CARTESIAN_POINT('Ctrl Pts',(5.82838558568782,6.26617071740664,3.88777814898226));
#56170=CARTESIAN_POINT('Ctrl Pts',(6.25099836192328,4.94745326120368,4.6491400273061));
#56171=CARTESIAN_POINT('Ctrl Pts',(6.49028076601058,3.14668033196789,5.68881676274977));
#56172=CARTESIAN_POINT('Ctrl Pts',(6.14463154721472,1.22101319991002,6.800601199813));
#56173=CARTESIAN_POINT('Ctrl Pts',(5.82838421256034,0.233829133738886,7.37055218615661));
#56174=CARTESIAN_POINT('',(6.19472803466948,1.64850575197389E-14,7.22496982822515));
#56175=CARTESIAN_POINT('Ctrl Pts',(6.19472803466948,1.80893230908424E-14,
7.22496982822515));
#56176=CARTESIAN_POINT('Ctrl Pts',(6.13372354963894,0.0390501553628601,
7.24921270476878));
#56177=CARTESIAN_POINT('Ctrl Pts',(6.07269500050579,0.078059193557057,7.27346514426615));
#56178=CARTESIAN_POINT('Ctrl Pts',(5.95058061166719,0.156001057525407,7.32199279024714));
#56179=CARTESIAN_POINT('Ctrl Pts',(5.88949278160536,0.194935129147796,7.34626878768841));
#56180=CARTESIAN_POINT('Ctrl Pts',(5.82838302289431,0.233826859022126,7.37055349946495));
#56181=CARTESIAN_POINT('Ctrl Pts',(6.19472803466948,1.72084568816899E-14,
7.22496982822515));
#56182=CARTESIAN_POINT('Ctrl Pts',(6.4306550195388,0.71313481548644,6.81686654700397));
#56183=CARTESIAN_POINT('Ctrl Pts',(6.58105248112949,1.34886989409368,6.45303961304062));
#56184=CARTESIAN_POINT('Ctrl Pts',(6.66504514382361,1.95339415557755,6.10593986929842));
#56185=CARTESIAN_POINT('Ctrl Pts',(5.82127992530897,6.5,3.50831139001062));
#56186=CARTESIAN_POINT('Ctrl Pts',(6.14241820370575,6.5,2.35707374163067));
#56187=CARTESIAN_POINT('Ctrl Pts',(6.49243586254982,6.5,0.118785051139947));
#56188=CARTESIAN_POINT('Ctrl Pts',(6.2494642965047,6.5,-1.97332785883874));
#56189=CARTESIAN_POINT('Ctrl Pts',(5.82127992530902,6.5,-3.50831139001059));
#56190=CARTESIAN_POINT('Ctrl Pts',(5.94576262842914,6.4190024709397,3.5430358980446));
#56191=CARTESIAN_POINT('Ctrl Pts',(6.27212071493947,6.4204964496477,2.38456443644942));
#56192=CARTESIAN_POINT('Ctrl Pts',(6.63194145333222,6.42341735463559,0.121399944768468));
#56193=CARTESIAN_POINT('Ctrl Pts',(6.38090674377616,6.42099444255031,-1.99840728258573));
#56194=CARTESIAN_POINT('Ctrl Pts',(5.94576262842917,6.41900247093969,-3.54303589804459));
#56195=CARTESIAN_POINT('Ctrl Pts',(6.07024533154931,6.33800494187939,3.57776040607858));
#56196=CARTESIAN_POINT('Ctrl Pts',(6.40182322617319,6.3409928992954,2.41205513126817));
#56197=CARTESIAN_POINT('Ctrl Pts',(6.77144704411462,6.34683470927118,0.124014838396988));
#56198=CARTESIAN_POINT('Ctrl Pts',(6.51234919104763,6.34198888510063,-2.02348670633271));
#56199=CARTESIAN_POINT('Ctrl Pts',(6.07024533154933,6.33800494187938,-3.5777604060786));
#56200=CARTESIAN_POINT('Ctrl Pts',(6.19472803466948,6.25700741281908,3.61248491411256));
#56201=CARTESIAN_POINT('Ctrl Pts',(6.53152573740691,6.2614893489431,2.43954582608692));
#56202=CARTESIAN_POINT('Ctrl Pts',(6.91095263489701,6.27025206390677,0.12662973202551));
#56203=CARTESIAN_POINT('Ctrl Pts',(6.64379163831909,6.26298332765094,-2.0485661300797));
#56204=CARTESIAN_POINT('Ctrl Pts',(6.19472803466948,6.25700741281906,-3.6124849141126));
#56205=CARTESIAN_POINT('',(6.19472803466948,6.25700741281907,-3.61248491411259));
#56206=CARTESIAN_POINT('Ctrl Pts',(6.66943768475789,6.26442235049367,-1.36025300283622));
#56207=CARTESIAN_POINT('Ctrl Pts',(6.58476982174516,6.2627836062947,-2.05778423124321));
#56208=CARTESIAN_POINT('Ctrl Pts',(6.43065501953876,6.26014701165687,-2.79084040696789));
#56209=CARTESIAN_POINT('Ctrl Pts',(6.19472803466948,6.25700741281906,-3.6124849141126));
#56210=CARTESIAN_POINT('',(5.82838302289405,6.5,-3.4827767497333));
#56211=CARTESIAN_POINT('Ctrl Pts',(5.82838302289405,6.5,-3.4827767497333));
#56212=CARTESIAN_POINT('Ctrl Pts',(5.88949356895823,6.45952243622465,-3.50431589742522));
#56213=CARTESIAN_POINT('Ctrl Pts',(5.9505821858056,6.41903124806158,-3.52589607237054));
#56214=CARTESIAN_POINT('Ctrl Pts',(6.07269657345908,6.33803414120459,-3.56913188569258));
#56215=CARTESIAN_POINT('Ctrl Pts',(6.13372433579894,6.29752691526968,-3.59078820542605));
#56216=CARTESIAN_POINT('Ctrl Pts',(6.19472803466948,6.25700741281906,-3.6124849141126));
#56217=CARTESIAN_POINT('',(5.82838302289382,6.5,3.48277674973257));
#56218=CARTESIAN_POINT('Ctrl Pts',(5.82838560050068,6.5,-3.48277395419486));
#56219=CARTESIAN_POINT('Ctrl Pts',(6.25100014187621,6.5,-1.96005055047028));
#56220=CARTESIAN_POINT('Ctrl Pts',(6.49056037813313,6.5,0.119247370498949));
#56221=CARTESIAN_POINT('Ctrl Pts',(6.14463332716764,6.5,2.34287179454352));
#56222=CARTESIAN_POINT('Ctrl Pts',(5.82838423229859,6.5,3.48277411916905));
#56223=CARTESIAN_POINT('Ctrl Pts',(6.19472803466948,6.25700741281908,3.61248491411256));
#56224=CARTESIAN_POINT('Ctrl Pts',(6.13372354963881,6.29752743744818,3.59078792581838));
#56225=CARTESIAN_POINT('Ctrl Pts',(6.07269500050538,6.33803518525394,3.56913132751359));
#56226=CARTESIAN_POINT('Ctrl Pts',(5.95058061167076,6.41903229144087,3.52589551629059));
#56227=CARTESIAN_POINT('Ctrl Pts',(5.8894927816124,6.45952295773611,3.50431561991468));
#56228=CARTESIAN_POINT('Ctrl Pts',(5.82838302289431,6.5,3.48277674973218));
#56229=CARTESIAN_POINT('Ctrl Pts',(6.19472803466948,6.25700741281908,3.61248491411256));
#56230=CARTESIAN_POINT('Ctrl Pts',(6.4306550195388,6.26014701165697,2.7908404069676));
#56231=CARTESIAN_POINT('Ctrl Pts',(6.58110866402936,6.26293012262745,2.05835104785734));
#56232=CARTESIAN_POINT('Ctrl Pts',(6.66514060252342,6.26459431596996,1.36125860579049));
#56233=CARTESIAN_POINT('Origin',(6.177207419323,0.,0.));
#56234=CARTESIAN_POINT('Origin',(6.177207419323,0.,0.));
#56235=CARTESIAN_POINT('Ctrl Pts',(6.19472803466948,6.25700741281907,-3.61248491411259));
#56236=CARTESIAN_POINT('Ctrl Pts',(6.4306550195388,5.54701219617053,-4.02602614003637));
#56237=CARTESIAN_POINT('Ctrl Pts',(6.58472768457028,4.91347707050872,-4.39484321142696));
#56238=CARTESIAN_POINT('Ctrl Pts',(6.66935871145421,4.3102095520817,-4.74503293760454));
#56239=CARTESIAN_POINT('Origin',(6.177207419323,0.,0.));
#56240=CARTESIAN_POINT('',(6.19472803466948,-1.72045194734352E-14,-7.22496982822515));
#56241=CARTESIAN_POINT('Ctrl Pts',(6.19472803466948,-1.47104550762833E-14,
-7.22496982822515));
#56242=CARTESIAN_POINT('Ctrl Pts',(6.4306550195388,-0.71313481548644,-6.81686654700397));
#56243=CARTESIAN_POINT('Ctrl Pts',(6.58105248112949,-1.34886989409368,-6.45303961304062));
#56244=CARTESIAN_POINT('Ctrl Pts',(6.66504514382362,-1.95339415557755,-6.10593986929842));
#56245=CARTESIAN_POINT('Ctrl Pts',(6.66504514382361,1.9533941555772,-6.10593986929854));
#56246=CARTESIAN_POINT('Ctrl Pts',(6.58105248112947,1.34886989409327,-6.45303961304075));
#56247=CARTESIAN_POINT('Ctrl Pts',(6.43065501953876,0.713134815486147,-6.81686654700404));
#56248=CARTESIAN_POINT('Ctrl Pts',(6.19472803466948,-1.80411241501588E-14,
-7.22496982822515));
#56249=CARTESIAN_POINT('Origin',(6.177207419323,0.,0.));
#56250=CARTESIAN_POINT('',(6.19472803466948,-6.25700741281908,-3.61248491411256));
#56251=CARTESIAN_POINT('Ctrl Pts',(6.19472803466948,-6.25700741281908,-3.61248491411256));
#56252=CARTESIAN_POINT('Ctrl Pts',(6.4306550195388,-6.26014701165697,-2.7908404069676));
#56253=CARTESIAN_POINT('Ctrl Pts',(6.58110866402936,-6.26293012262745,-2.05835104785735));
#56254=CARTESIAN_POINT('Ctrl Pts',(6.66514060252342,-6.26459431596996,-1.3612586057905));
#56255=CARTESIAN_POINT('Ctrl Pts',(6.66935871145421,-4.31020955208199,-4.7450329376043));
#56256=CARTESIAN_POINT('Ctrl Pts',(6.58472768457026,-4.91347707050904,-4.39484321142667));
#56257=CARTESIAN_POINT('Ctrl Pts',(6.43065501953876,-5.54701219617073,-4.02602614003615));
#56258=CARTESIAN_POINT('Ctrl Pts',(6.19472803466948,-6.25700741281908,-3.61248491411256));
#56259=CARTESIAN_POINT('Origin',(6.177207419323,0.,0.));
#56260=CARTESIAN_POINT('',(6.19472803466948,-6.25700741281907,3.61248491411259));
#56261=CARTESIAN_POINT('Ctrl Pts',(6.19472803466948,-6.25700741281907,3.61248491411259));
#56262=CARTESIAN_POINT('Ctrl Pts',(6.4306550195388,-5.54701219617053,4.02602614003637));
#56263=CARTESIAN_POINT('Ctrl Pts',(6.58472768457028,-4.91347707050872,4.39484321142696));
#56264=CARTESIAN_POINT('Ctrl Pts',(6.66935871145421,-4.3102095520817,4.74503293760454));
#56265=CARTESIAN_POINT('Ctrl Pts',(6.66943768475789,-6.26442235049367,1.36025300283621));
#56266=CARTESIAN_POINT('Ctrl Pts',(6.58476982174516,-6.2627836062947,2.0577842312432));
#56267=CARTESIAN_POINT('Ctrl Pts',(6.43065501953876,-6.26014701165688,2.79084040696788));
#56268=CARTESIAN_POINT('Ctrl Pts',(6.19472803466948,-6.25700741281907,3.61248491411259));
#56269=CARTESIAN_POINT('Origin',(6.177207419323,0.,0.));
#56270=CARTESIAN_POINT('Ctrl Pts',(6.66504514382361,-1.9533941555772,6.10593986929854));
#56271=CARTESIAN_POINT('Ctrl Pts',(6.58105248112947,-1.34886989409327,6.45303961304075));
#56272=CARTESIAN_POINT('Ctrl Pts',(6.43065501953876,-0.713134815486151,
6.81686654700403));
#56273=CARTESIAN_POINT('Ctrl Pts',(6.19472803466948,1.49880108324396E-14,
7.22496982822515));
#56274=CARTESIAN_POINT('Ctrl Pts',(5.82127992530896,6.2882867881355,-3.87500942959354));
#56275=CARTESIAN_POINT('Ctrl Pts',(6.24946429650468,4.95895205574871,-4.64250119518017));
#56276=CARTESIAN_POINT('Ctrl Pts',(6.49215447047434,3.14708040407028,-5.68858578101377));
#56277=CARTESIAN_POINT('Ctrl Pts',(6.14241820370578,1.20871426115372,-6.8077019954147));
#56278=CARTESIAN_POINT('Ctrl Pts',(5.82127992530902,0.211713211864542,-7.38332081960414));
#56279=CARTESIAN_POINT('Ctrl Pts',(5.94576262842914,6.27786032969669,-3.78750125776656));
#56280=CARTESIAN_POINT('Ctrl Pts',(6.38090674377625,4.94116869510108,-4.56154066351513));
#56281=CARTESIAN_POINT('Ctrl Pts',(6.63166480681809,3.10652352931727,-5.62357322351106));
#56282=CARTESIAN_POINT('Ctrl Pts',(6.27212071493942,1.14515484589683,-6.75259524852789));
#56283=CARTESIAN_POINT('Ctrl Pts',(5.94576262842918,0.141142141243022,-7.33053715581114));
#56284=CARTESIAN_POINT('Ctrl Pts',(6.07024533154931,6.26743387125788,-3.69999308593957));
#56285=CARTESIAN_POINT('Ctrl Pts',(6.51234919104782,4.92338533445344,-4.4805801318501));
#56286=CARTESIAN_POINT('Ctrl Pts',(6.77117514316185,3.06596665456427,-5.55856066600836));
#56287=CARTESIAN_POINT('Ctrl Pts',(6.40182322617305,1.08159543063994,-6.69748850164107));
#56288=CARTESIAN_POINT('Ctrl Pts',(6.07024533154933,0.0705710706215021,
-7.27775349201815));
#56289=CARTESIAN_POINT('Ctrl Pts',(6.19472803466948,6.25700741281907,-3.61248491411259));
#56290=CARTESIAN_POINT('Ctrl Pts',(6.64379163831939,4.90560197380581,-4.39961960018506));
#56291=CARTESIAN_POINT('Ctrl Pts',(6.9106854795056,3.02540977981126,-5.49354810850567));
#56292=CARTESIAN_POINT('Ctrl Pts',(6.53152573740669,1.01803601538305,-6.64238175475426));
#56293=CARTESIAN_POINT('Ctrl Pts',(6.19472803466948,-1.80411241501588E-14,
-7.22496982822515));
#56294=CARTESIAN_POINT('',(5.82838302289405,0.233826859021164,-7.3705534994655));
#56295=CARTESIAN_POINT('Ctrl Pts',(5.82838302289405,0.23382685902116,-7.3705534994655));
#56296=CARTESIAN_POINT('Ctrl Pts',(5.88949356894673,0.194934628063732,-7.34626847480328));
#56297=CARTESIAN_POINT('Ctrl Pts',(5.95058218580015,0.156000054257608,-7.3219921646949));
#56298=CARTESIAN_POINT('Ctrl Pts',(6.07269657345378,0.0780581881388463,
-7.27346451918466));
#56299=CARTESIAN_POINT('Ctrl Pts',(6.13372433579649,0.0390496521279212,
-7.24921239235379));
#56300=CARTESIAN_POINT('Ctrl Pts',(6.19472803466948,-1.88087850445387E-14,
-7.22496982822515));
#56301=CARTESIAN_POINT('',(5.82838302289383,6.2661731409782,-3.88777674973257));
#56302=CARTESIAN_POINT('Ctrl Pts',(5.82838421256022,0.233829133738336,-7.37055218615693));
#56303=CARTESIAN_POINT('Ctrl Pts',(6.14463154721469,1.22101319990882,-6.80060119981369));
#56304=CARTESIAN_POINT('Ctrl Pts',(6.49028076601056,3.14668033196568,-5.68881676275105));
#56305=CARTESIAN_POINT('Ctrl Pts',(6.2509983619233,4.94745326120219,-4.64914002730696));
#56306=CARTESIAN_POINT('Ctrl Pts',(5.82838558568794,6.26617071740608,-3.88777814898258));
#56307=CARTESIAN_POINT('Ctrl Pts',(6.19472803466948,6.25700741281907,-3.61248491411259));
#56308=CARTESIAN_POINT('Ctrl Pts',(6.13372354963734,6.25847728208528,-3.65842477895156));
#56309=CARTESIAN_POINT('Ctrl Pts',(6.07269500050242,6.25997599169669,-3.70433381675495));
#56310=CARTESIAN_POINT('Ctrl Pts',(5.9505806116696,6.26303123391776,-3.796097273956));
#56311=CARTESIAN_POINT('Ctrl Pts',(5.88949278161014,6.26458782859284,-3.84195316777262));
#56312=CARTESIAN_POINT('Ctrl Pts',(5.82838302289431,6.26617314097787,-3.88777674973276));
#56313=CARTESIAN_POINT('Origin',(6.8,0.,-1.11022302462516E-15));
#56314=CARTESIAN_POINT('',(6.8,-4.37,5.35170651227393E-16));
#56315=CARTESIAN_POINT('Origin',(6.8,0.,0.));
#56316=CARTESIAN_POINT('Origin',(5.82838302289405,6.5,-3.4827767497333));
#56317=CARTESIAN_POINT('',(5.82838302289387,6.5,-3.48277674973257));
#56318=CARTESIAN_POINT('Origin',(6.19472803466948,-1.72045194734352E-14,
-7.22496982822515));
#56319=CARTESIAN_POINT('',(5.82838302289383,-0.2338268590218,-7.37055349946514));
#56320=CARTESIAN_POINT('Ctrl Pts',(6.19472803466948,-1.39959883312281E-14,
-7.22496982822515));
#56321=CARTESIAN_POINT('Ctrl Pts',(6.13372354964118,-0.0390501553614202,
-7.24921270476789));
#56322=CARTESIAN_POINT('Ctrl Pts',(6.07269500051012,-0.0780591935542958,
-7.27346514426443));
#56323=CARTESIAN_POINT('Ctrl Pts',(5.95058061167065,-0.156001057523206,
-7.32199279024577));
#56324=CARTESIAN_POINT('Ctrl Pts',(5.88949278161218,-0.194935129143466,
-7.3462687876857));
#56325=CARTESIAN_POINT('Ctrl Pts',(5.82838302289431,-0.233826859022136,
-7.37055349946494));
#56326=CARTESIAN_POINT('',(5.82838302289387,0.233826859021797,-7.37055349946514));
#56327=CARTESIAN_POINT('Origin',(5.82838302289405,6.26617314097884,3.8877767497322));
#56328=CARTESIAN_POINT('',(5.82838302289387,6.2661731409782,3.88777674973257));
#56329=CARTESIAN_POINT('Origin',(6.19472803466948,-6.25700741281908,-3.61248491411256));
#56330=CARTESIAN_POINT('',(5.82838302289405,-6.26617314097884,-3.8877767497322));
#56331=CARTESIAN_POINT('Ctrl Pts',(5.82838302289405,-6.26617314097884,-3.8877767497322));
#56332=CARTESIAN_POINT('Ctrl Pts',(5.88949356895342,-6.26458780816836,-3.84195257737708));
#56333=CARTESIAN_POINT('Ctrl Pts',(5.95058218580324,-6.26303119380752,-3.79609609232396));
#56334=CARTESIAN_POINT('Ctrl Pts',(6.07269657345032,-6.25997595306935,-3.70433263349656));
#56335=CARTESIAN_POINT('Ctrl Pts',(6.13372433579501,-6.25847726314342,-3.65842418692974));
#56336=CARTESIAN_POINT('Ctrl Pts',(6.19472803466948,-6.25700741281908,-3.61248491411257));
#56337=CARTESIAN_POINT('',(5.82838302289383,-6.5,-3.48277674973257));
#56338=CARTESIAN_POINT('Ctrl Pts',(6.19472803466948,-6.25700741281908,-3.61248491411257));
#56339=CARTESIAN_POINT('Ctrl Pts',(6.13372354964143,-6.29752743744644,-3.59078792581931));
#56340=CARTESIAN_POINT('Ctrl Pts',(6.07269500051088,-6.33803518525029,-3.56913132751554));
#56341=CARTESIAN_POINT('Ctrl Pts',(5.95058061166937,-6.41903229144179,-3.5258955162901));
#56342=CARTESIAN_POINT('Ctrl Pts',(5.88949278160931,-6.45952295773815,-3.5043156199136));
#56343=CARTESIAN_POINT('Ctrl Pts',(5.82838302289431,-6.5,-3.48277674973218));
#56344=CARTESIAN_POINT('',(5.82838302289387,-6.2661731409782,-3.88777674973257));
#56345=CARTESIAN_POINT('Origin',(5.82838302289405,-0.233826859021165,7.3705534994655));
#56346=CARTESIAN_POINT('',(5.82838302289405,-0.233826859021165,7.3705534994655));
#56347=CARTESIAN_POINT('',(5.82838302289388,-0.233826859021798,7.37055349946514));
#56348=CARTESIAN_POINT('Ctrl Pts',(5.82838302289405,-0.233826859021165,
7.3705534994655));
#56349=CARTESIAN_POINT('Ctrl Pts',(5.88949356895343,-0.194934628059473,
7.34626847480061));
#56350=CARTESIAN_POINT('Ctrl Pts',(5.95058218580337,-0.156000054255553,
7.32199216469362));
#56351=CARTESIAN_POINT('Ctrl Pts',(6.07269657344927,-0.0780581881417256,
7.27346451918645));
#56352=CARTESIAN_POINT('Ctrl Pts',(6.13372433579441,-0.0390496521292542,
7.24921239235461));
#56353=CARTESIAN_POINT('Ctrl Pts',(6.19472803466949,1.16722608064283E-14,
7.22496982822515));
#56354=CARTESIAN_POINT('Origin',(6.19472803466948,-6.25700741281907,3.61248491411259));
#56355=CARTESIAN_POINT('',(5.82838302289405,-6.5,3.4827767497333));
#56356=CARTESIAN_POINT('Ctrl Pts',(5.82838302289405,-6.5,3.4827767497333));
#56357=CARTESIAN_POINT('Ctrl Pts',(5.88949356894732,-6.45952243623187,3.50431589742138));
#56358=CARTESIAN_POINT('Ctrl Pts',(5.95058218580049,-6.41903124806498,3.52589607236873));
#56359=CARTESIAN_POINT('Ctrl Pts',(6.07269657345065,-6.33803414121018,3.56913188568959));
#56360=CARTESIAN_POINT('Ctrl Pts',(6.13372433579476,-6.29752691527246,3.59078820542455));
#56361=CARTESIAN_POINT('Ctrl Pts',(6.19472803466948,-6.25700741281907,3.61248491411259));
#56362=CARTESIAN_POINT('',(5.82838302289383,-6.2661731409782,3.88777674973257));
#56363=CARTESIAN_POINT('Ctrl Pts',(6.19472803466948,-6.25700741281907,3.61248491411259));
#56364=CARTESIAN_POINT('Ctrl Pts',(6.13372354964038,-6.25847728208521,3.65842477894927));
#56365=CARTESIAN_POINT('Ctrl Pts',(6.07269500050845,-6.25997599169654,3.70433381675042));
#56366=CARTESIAN_POINT('Ctrl Pts',(5.95058061166901,-6.26303123391778,3.79609727395645));
#56367=CARTESIAN_POINT('Ctrl Pts',(5.88949278160903,-6.26458782859287,3.84195316777345));
#56368=CARTESIAN_POINT('Ctrl Pts',(5.82838302289431,-6.26617314097787,3.88777674973276));
#56369=CARTESIAN_POINT('',(5.82838302289387,-6.5,3.48277674973257));
#56370=CARTESIAN_POINT('Ctrl Pts',(5.82127992530897,-6.2882867881355,3.87500942959354));
#56371=CARTESIAN_POINT('Ctrl Pts',(6.24946429650468,-4.95895205574871,4.64250119518017));
#56372=CARTESIAN_POINT('Ctrl Pts',(6.49215447047434,-3.14708040407028,5.68858578101376));
#56373=CARTESIAN_POINT('Ctrl Pts',(6.14241820370578,-1.20871426115372,6.8077019954147));
#56374=CARTESIAN_POINT('Ctrl Pts',(5.82127992530902,-0.211713211864546,
7.38332081960414));
#56375=CARTESIAN_POINT('Ctrl Pts',(5.94576262842914,-6.27786032969669,3.78750125776656));
#56376=CARTESIAN_POINT('Ctrl Pts',(6.38090674377625,-4.94116869510108,4.56154066351513));
#56377=CARTESIAN_POINT('Ctrl Pts',(6.63166480681809,-3.10652352931728,5.62357322351106));
#56378=CARTESIAN_POINT('Ctrl Pts',(6.27212071493942,-1.14515484589683,6.75259524852789));
#56379=CARTESIAN_POINT('Ctrl Pts',(5.94576262842918,-0.141142141243025,
7.33053715581114));
#56380=CARTESIAN_POINT('Ctrl Pts',(6.07024533154931,-6.26743387125788,3.69999308593957));
#56381=CARTESIAN_POINT('Ctrl Pts',(6.51234919104782,-4.92338533445345,4.4805801318501));
#56382=CARTESIAN_POINT('Ctrl Pts',(6.77117514316185,-3.06596665456427,5.55856066600836));
#56383=CARTESIAN_POINT('Ctrl Pts',(6.40182322617305,-1.08159543063994,6.69748850164107));
#56384=CARTESIAN_POINT('Ctrl Pts',(6.07024533154933,-0.0705710706215052,
7.27775349201815));
#56385=CARTESIAN_POINT('Ctrl Pts',(6.19472803466948,-6.25700741281907,3.61248491411259));
#56386=CARTESIAN_POINT('Ctrl Pts',(6.64379163831939,-4.90560197380581,4.39961960018506));
#56387=CARTESIAN_POINT('Ctrl Pts',(6.9106854795056,-3.02540977981126,5.49354810850567));
#56388=CARTESIAN_POINT('Ctrl Pts',(6.53152573740669,-1.01803601538306,6.64238175475426));
#56389=CARTESIAN_POINT('Ctrl Pts',(6.19472803466948,1.49880108324396E-14,
7.22496982822515));
#56390=CARTESIAN_POINT('Ctrl Pts',(5.82838421256021,-0.233829133738338,
7.37055218615693));
#56391=CARTESIAN_POINT('Ctrl Pts',(6.14463154721469,-1.22101319990882,6.80060119981369));
#56392=CARTESIAN_POINT('Ctrl Pts',(6.49028076601056,-3.14668033196568,5.68881676275105));
#56393=CARTESIAN_POINT('Ctrl Pts',(6.2509983619233,-4.9474532612022,4.64914002730695));
#56394=CARTESIAN_POINT('Ctrl Pts',(5.82838558568794,-6.26617071740609,3.88777814898258));
#56395=CARTESIAN_POINT('Origin',(0.,-6.3830865704891,3.68527674973257));
#56396=CARTESIAN_POINT('',(0.691578435026327,-6.2661731409782,3.88777674973257));
#56397=CARTESIAN_POINT('',(0.691578435026392,-6.5,3.48277674973257));
#56398=CARTESIAN_POINT('Ctrl Pts',(0.691578435026327,-6.2661731409782,3.88777674973257));
#56399=CARTESIAN_POINT('Ctrl Pts',(0.687292182208882,-6.3830865704891,3.68527674973257));
#56400=CARTESIAN_POINT('Ctrl Pts',(0.691578435026392,-6.5,3.48277674973257));
#56401=CARTESIAN_POINT('',(0.,-6.5,3.48277674973257));
#56402=CARTESIAN_POINT('',(0.,-6.2661731409782,3.88777674973257));
#56403=CARTESIAN_POINT('Ctrl Pts',(5.82127992530897,-6.5,-3.50831139001062));
#56404=CARTESIAN_POINT('Ctrl Pts',(6.14241820370575,-6.5,-2.35707374163068));
#56405=CARTESIAN_POINT('Ctrl Pts',(6.49243586254982,-6.5,-0.118785051139954));
#56406=CARTESIAN_POINT('Ctrl Pts',(6.2494642965047,-6.5,1.97332785883873));
#56407=CARTESIAN_POINT('Ctrl Pts',(5.82127992530902,-6.5,3.50831139001058));
#56408=CARTESIAN_POINT('Ctrl Pts',(5.94576262842914,-6.41900247093969,-3.5430358980446));
#56409=CARTESIAN_POINT('Ctrl Pts',(6.27212071493947,-6.4204964496477,-2.38456443644943));
#56410=CARTESIAN_POINT('Ctrl Pts',(6.63194145333222,-6.42341735463559,-0.121399944768473));
#56411=CARTESIAN_POINT('Ctrl Pts',(6.38090674377616,-6.42099444255032,1.99840728258572));
#56412=CARTESIAN_POINT('Ctrl Pts',(5.94576262842918,-6.41900247093969,3.54303589804458));
#56413=CARTESIAN_POINT('Ctrl Pts',(6.07024533154931,-6.33800494187939,-3.57776040607858));
#56414=CARTESIAN_POINT('Ctrl Pts',(6.40182322617319,-6.3409928992954,-2.41205513126818));
#56415=CARTESIAN_POINT('Ctrl Pts',(6.77144704411462,-6.34683470927118,-0.124014838396995));
#56416=CARTESIAN_POINT('Ctrl Pts',(6.51234919104763,-6.34198888510063,2.02348670633271));
#56417=CARTESIAN_POINT('Ctrl Pts',(6.07024533154933,-6.33800494187938,3.57776040607859));
#56418=CARTESIAN_POINT('Ctrl Pts',(6.19472803466948,-6.25700741281908,-3.61248491411256));
#56419=CARTESIAN_POINT('Ctrl Pts',(6.53152573740691,-6.2614893489431,-2.43954582608693));
#56420=CARTESIAN_POINT('Ctrl Pts',(6.91095263489701,-6.27025206390677,-0.126629732025515));
#56421=CARTESIAN_POINT('Ctrl Pts',(6.64379163831909,-6.26298332765095,2.0485661300797));
#56422=CARTESIAN_POINT('Ctrl Pts',(6.19472803466948,-6.25700741281907,3.61248491411259));
#56423=CARTESIAN_POINT('Ctrl Pts',(5.82838560050068,-6.5,3.48277395419486));
#56424=CARTESIAN_POINT('Ctrl Pts',(6.25100014187621,-6.5,1.96005055047028));
#56425=CARTESIAN_POINT('Ctrl Pts',(6.49056037813313,-6.5,-0.119247370498952));
#56426=CARTESIAN_POINT('Ctrl Pts',(6.14463332716764,-6.5,-2.34287179454352));
#56427=CARTESIAN_POINT('Ctrl Pts',(5.82838423229859,-6.5,-3.48277411916905));
#56428=CARTESIAN_POINT('Origin',(0.,5.3776427755281E-16,7.37055349946514));
#56429=CARTESIAN_POINT('',(0.691578435026327,0.233826859021798,7.37055349946513));
#56430=CARTESIAN_POINT('',(0.691578435026391,-0.233826859021798,7.37055349946514));
#56431=CARTESIAN_POINT('Ctrl Pts',(0.691578435026327,0.233826859021798,
7.37055349946513));
#56432=CARTESIAN_POINT('Ctrl Pts',(0.687292182208882,3.78169717762944E-15,
7.37055349946514));
#56433=CARTESIAN_POINT('Ctrl Pts',(0.691578435026391,-0.233826859021798,
7.37055349946514));
#56434=CARTESIAN_POINT('',(0.,-0.233826859021798,7.37055349946514));
#56435=CARTESIAN_POINT('',(0.,0.233826859021799,7.37055349946514));
#56436=CARTESIAN_POINT('Origin',(0.,-6.3830865704891,-3.68527674973257));
#56437=CARTESIAN_POINT('',(0.691578435026327,-6.5,-3.48277674973257));
#56438=CARTESIAN_POINT('',(0.691578435026391,-6.2661731409782,-3.88777674973257));
#56439=CARTESIAN_POINT('Ctrl Pts',(0.691578435026327,-6.5,-3.48277674973257));
#56440=CARTESIAN_POINT('Ctrl Pts',(0.687292182208882,-6.38308657048911,
-3.68527674973256));
#56441=CARTESIAN_POINT('Ctrl Pts',(0.691578435026391,-6.2661731409782,-3.88777674973257));
#56442=CARTESIAN_POINT('',(0.,-6.2661731409782,-3.88777674973257));
#56443=CARTESIAN_POINT('',(0.,-6.5,-3.48277674973257));
#56444=CARTESIAN_POINT('Ctrl Pts',(5.82127992530897,-0.211713211864505,
-7.38332081960416));
#56445=CARTESIAN_POINT('Ctrl Pts',(6.14241820370575,-1.20871426115459,-6.80770199541419));
#56446=CARTESIAN_POINT('Ctrl Pts',(6.49215447047434,-3.14708040407219,-5.68858578101266));
#56447=CARTESIAN_POINT('Ctrl Pts',(6.2494642965047,-4.95895205574989,-4.64250119517949));
#56448=CARTESIAN_POINT('Ctrl Pts',(5.82127992530902,-6.28828678813546,-3.87500942959356));
#56449=CARTESIAN_POINT('Ctrl Pts',(5.94576262842914,-0.141142141243009,
-7.33053715581116));
#56450=CARTESIAN_POINT('Ctrl Pts',(6.27212071493947,-1.14515484589772,-6.75259524852742));
#56451=CARTESIAN_POINT('Ctrl Pts',(6.63166480681812,-3.1065235293192,-5.62357322350997));
#56452=CARTESIAN_POINT('Ctrl Pts',(6.38090674377616,-4.94116869510222,-4.56154066351441));
#56453=CARTESIAN_POINT('Ctrl Pts',(5.94576262842917,-6.27786032969667,-3.78750125776656));
#56454=CARTESIAN_POINT('Ctrl Pts',(6.07024533154931,-0.0705710706215116,
-7.27775349201816));
#56455=CARTESIAN_POINT('Ctrl Pts',(6.40182322617319,-1.08159543064085,-6.69748850164065));
#56456=CARTESIAN_POINT('Ctrl Pts',(6.7711751431619,-3.06596665456621,-5.55856066600728));
#56457=CARTESIAN_POINT('Ctrl Pts',(6.51234919104763,-4.92338533445454,-4.48058013184934));
#56458=CARTESIAN_POINT('Ctrl Pts',(6.07024533154933,-6.26743387125788,-3.69999308593956));
#56459=CARTESIAN_POINT('Ctrl Pts',(6.19472803466948,-1.47104550762833E-14,
-7.22496982822515));
#56460=CARTESIAN_POINT('Ctrl Pts',(6.53152573740691,-1.01803601538398,-6.64238175475387));
#56461=CARTESIAN_POINT('Ctrl Pts',(6.91068547950568,-3.02540977981322,-5.49354810850458));
#56462=CARTESIAN_POINT('Ctrl Pts',(6.64379163831909,-4.90560197380687,-4.39961960018427));
#56463=CARTESIAN_POINT('Ctrl Pts',(6.19472803466948,-6.25700741281908,-3.61248491411256));
#56464=CARTESIAN_POINT('Ctrl Pts',(5.82838558568782,-6.26617071740664,-3.88777814898226));
#56465=CARTESIAN_POINT('Ctrl Pts',(6.25099836192328,-4.94745326120368,-4.6491400273061));
#56466=CARTESIAN_POINT('Ctrl Pts',(6.49028076601057,-3.14668033196789,-5.68881676274977));
#56467=CARTESIAN_POINT('Ctrl Pts',(6.14463154721472,-1.22101319991002,-6.800601199813));
#56468=CARTESIAN_POINT('Ctrl Pts',(5.82838421256034,-0.233829133738889,
-7.37055218615661));
#56469=CARTESIAN_POINT('Origin',(0.,6.3830865704891,3.68527674973257));
#56470=CARTESIAN_POINT('',(0.691578435026327,6.5,3.48277674973257));
#56471=CARTESIAN_POINT('',(0.691578435026392,6.2661731409782,3.88777674973257));
#56472=CARTESIAN_POINT('Ctrl Pts',(0.691578435026327,6.5,3.48277674973257));
#56473=CARTESIAN_POINT('Ctrl Pts',(0.687292182208883,6.3830865704891,3.68527674973256));
#56474=CARTESIAN_POINT('Ctrl Pts',(0.691578435026392,6.2661731409782,3.88777674973257));
#56475=CARTESIAN_POINT('',(0.,6.2661731409782,3.88777674973257));
#56476=CARTESIAN_POINT('',(0.,6.5,3.48277674973257));
#56477=CARTESIAN_POINT('Origin',(0.,-1.23165366794353E-15,-7.37055349946514));
#56478=CARTESIAN_POINT('',(0.691578435026327,-0.233826859021799,-7.37055349946513));
#56479=CARTESIAN_POINT('',(0.691578435026391,0.233826859021797,-7.37055349946514));
#56480=CARTESIAN_POINT('Ctrl Pts',(0.691578435026327,-0.233826859021799,
-7.37055349946513));
#56481=CARTESIAN_POINT('Ctrl Pts',(0.687292182208882,-4.44089209850063E-15,
-7.37055349946514));
#56482=CARTESIAN_POINT('Ctrl Pts',(0.691578435026391,0.233826859021797,
-7.37055349946514));
#56483=CARTESIAN_POINT('',(0.,0.233826859021797,-7.37055349946514));
#56484=CARTESIAN_POINT('',(0.,-0.2338268590218,-7.37055349946514));
#56485=CARTESIAN_POINT('Origin',(0.,6.3830865704891,-3.68527674973257));
#56486=CARTESIAN_POINT('',(0.691578435026327,6.2661731409782,-3.88777674973257));
#56487=CARTESIAN_POINT('',(0.691578435026391,6.5,-3.48277674973257));
#56488=CARTESIAN_POINT('Ctrl Pts',(0.691578435026327,6.2661731409782,-3.88777674973257));
#56489=CARTESIAN_POINT('Ctrl Pts',(0.687292182208882,6.3830865704891,-3.68527674973257));
#56490=CARTESIAN_POINT('Ctrl Pts',(0.691578435026391,6.5,-3.48277674973257));
#56491=CARTESIAN_POINT('',(0.,6.5,-3.48277674973257));
#56492=CARTESIAN_POINT('',(0.,6.2661731409782,-3.88777674973257));
#56493=CARTESIAN_POINT('Origin',(0.,6.5,3.75277674973257));
#56494=CARTESIAN_POINT('Ctrl Pts',(0.691578435026392,6.2661731409782,3.88777674973257));
#56495=CARTESIAN_POINT('Ctrl Pts',(-0.259333426979357,3.2499999999987,5.62916512459961));
#56496=CARTESIAN_POINT('Ctrl Pts',(0.691578435026327,0.233826859021798,
7.37055349946514));
#56497=CARTESIAN_POINT('Origin',(0.,6.5,-3.75277674973257));
#56498=CARTESIAN_POINT('Ctrl Pts',(0.691578435026391,6.5,-3.48277674973257));
#56499=CARTESIAN_POINT('Ctrl Pts',(-0.259333426979358,6.5,1.50435219836709E-12));
#56500=CARTESIAN_POINT('Ctrl Pts',(0.691578435026327,6.5,3.48277674973257));
#56501=CARTESIAN_POINT('Origin',(0.,-1.37874781034238E-15,-7.50555349946513));
#56502=CARTESIAN_POINT('Ctrl Pts',(0.691578435026391,0.233826859021797,
-7.37055349946514));
#56503=CARTESIAN_POINT('Ctrl Pts',(-0.259333426979357,3.2500000000013,-5.6291651245981));
#56504=CARTESIAN_POINT('Ctrl Pts',(0.691578435026327,6.2661731409782,-3.88777674973257));
#56505=CARTESIAN_POINT('Origin',(0.622792580677002,0.,0.));
#56506=CARTESIAN_POINT('',(0.,-6.17797863635533,7.56584176221328E-16));
#56507=CARTESIAN_POINT('Origin',(0.,0.,0.));
#56508=CARTESIAN_POINT('',(0.186162505632566,-6.5,-1.05927327362393E-15));
#56509=CARTESIAN_POINT('',(0.622792580677002,-7.25527674973257,-8.8851514484882E-16));
#56510=CARTESIAN_POINT('Ctrl Pts',(0.691578435026392,-6.5,3.48277674973257));
#56511=CARTESIAN_POINT('Ctrl Pts',(0.186162505632697,-6.5,1.63165792561282));
#56512=CARTESIAN_POINT('Ctrl Pts',(0.186162505632566,-6.5,-1.32252612780209E-15));
#56513=CARTESIAN_POINT('Ctrl Pts',(0.691578435026392,-0.233826859021798,
7.37055349946514));
#56514=CARTESIAN_POINT('Ctrl Pts',(-0.259333426979358,-3.2500000000013,
5.6291651245981));
#56515=CARTESIAN_POINT('Ctrl Pts',(0.691578435026327,-6.2661731409782,3.88777674973257));
#56516=CARTESIAN_POINT('Ctrl Pts',(0.691578435026391,-6.2661731409782,-3.88777674973257));
#56517=CARTESIAN_POINT('Ctrl Pts',(-0.25933342697936,-3.2499999999987,-5.6291651245996));
#56518=CARTESIAN_POINT('Ctrl Pts',(0.691578435026327,-0.233826859021799,
-7.37055349946513));
#56519=CARTESIAN_POINT('Ctrl Pts',(0.186162505632566,-6.5,-1.32252612780209E-15));
#56520=CARTESIAN_POINT('Ctrl Pts',(0.186162505632435,-6.5,-1.63165792561357));
#56521=CARTESIAN_POINT('Ctrl Pts',(0.691578435026327,-6.5,-3.48277674973257));
#56522=CARTESIAN_POINT('Origin',(0.15,0.,0.));
#56523=CARTESIAN_POINT('',(0.,-4.37,-5.35170651227393E-16));
#56524=CARTESIAN_POINT('Origin',(0.,0.,0.));
#56525=CARTESIAN_POINT('',(0.4,-4.05,-4.95981953654678E-16));
#56526=CARTESIAN_POINT('',(0.15,-4.25,-5.20474889637625E-16));
#56527=CARTESIAN_POINT('Origin',(0.4,0.,0.));
#56528=CARTESIAN_POINT('Origin',(3.4,0.,0.));
#56529=CARTESIAN_POINT('',(6.4,-4.05,-4.95981953654678E-16));
#56530=CARTESIAN_POINT('',(3.4,-4.05,-4.95981953654678E-16));
#56531=CARTESIAN_POINT('Origin',(6.4,0.,0.));
#56532=CARTESIAN_POINT('Origin',(6.65,0.,0.));
#56533=CARTESIAN_POINT('',(6.65,-4.25,-5.20474889637625E-16));
#56534=CARTESIAN_POINT('Origin',(0.,-6.5,-3.75277674973257));
#56535=CARTESIAN_POINT('Origin',(0.,-6.5,3.75277674973257));
#56536=CARTESIAN_POINT('Origin',(0.,4.5958260344746E-16,7.50555349946513));
#56537=CARTESIAN_POINT('Origin',(0.,0.,-1.11022302462516E-15));
#56538=CARTESIAN_POINT('',(0.,0.,140.));
#56539=CARTESIAN_POINT('',(0.,0.,140.));
#56540=CARTESIAN_POINT('',(0.,0.,140.));
#56541=CARTESIAN_POINT('',(0.,0.,140.));
#56542=CARTESIAN_POINT('',(0.,0.,140.));
#56543=CARTESIAN_POINT('',(0.,0.,140.));
#56544=CARTESIAN_POINT('',(0.,0.,140.));
#56545=CARTESIAN_POINT('',(0.,0.,140.));
#56546=CARTESIAN_POINT('',(0.,0.,140.));
#56547=CARTESIAN_POINT('',(0.,0.,140.));
#56548=CARTESIAN_POINT('',(0.,0.,140.));
#56549=CARTESIAN_POINT('',(0.,0.,140.));
#56550=CARTESIAN_POINT('',(44.,0.,140.));
#56551=CARTESIAN_POINT('',(-44.,0.,140.));
#56552=CARTESIAN_POINT('',(0.,0.,45.));
#56553=CARTESIAN_POINT('',(0.,0.,240.));
#56554=CARTESIAN_POINT('',(0.,0.,45.));
#56555=CARTESIAN_POINT('',(0.,0.,240.));
#56556=CARTESIAN_POINT('',(0.,0.,140.));
#56557=CARTESIAN_POINT('',(0.,0.,140.));
#56558=CARTESIAN_POINT('',(61.,0.,74.3115));
#56559=CARTESIAN_POINT('',(61.,0.,227.3115));
#56560=CARTESIAN_POINT('',(61.,0.,63.));
#56561=CARTESIAN_POINT('',(61.,0.,216.));
#56562=CARTESIAN_POINT('',(0.,0.,0.));
#56563=CARTESIAN_POINT('',(61.,-52.5,0.));
#56564=CARTESIAN_POINT('',(61.,-52.5,21.));
#56565=CARTESIAN_POINT('',(61.,52.5,0.));
#56566=CARTESIAN_POINT('',(61.,52.5,21.));
#56567=CARTESIAN_POINT('',(61.,-25.,18.));
#56568=CARTESIAN_POINT('',(61.,-25.,264.));
#56569=CARTESIAN_POINT('',(61.,25.,18.));
#56570=CARTESIAN_POINT('',(61.,25.,264.));
#56571=CARTESIAN_POINT('',(-61.,0.,74.3115));
#56572=CARTESIAN_POINT('',(-61.,0.,227.3115));
#56573=CARTESIAN_POINT('',(-61.,0.,63.));
#56574=CARTESIAN_POINT('',(-61.,0.,216.));
#56575=CARTESIAN_POINT('',(0.,0.,0.));
#56576=CARTESIAN_POINT('',(-61.,-52.5,0.));
#56577=CARTESIAN_POINT('',(-61.,-52.5,21.));
#56578=CARTESIAN_POINT('',(-61.,52.5,0.));
#56579=CARTESIAN_POINT('',(-61.,52.5,21.));
#56580=CARTESIAN_POINT('',(-61.,-25.,18.));
#56581=CARTESIAN_POINT('',(-61.,-25.,264.));
#56582=CARTESIAN_POINT('',(-61.,25.,18.));
#56583=CARTESIAN_POINT('',(-61.,25.,264.));
#56584=CARTESIAN_POINT('',(-48.5,62.,140.));
#56585=CARTESIAN_POINT('',(48.5,62.,140.));
#56586=CARTESIAN_POINT('',(-48.5,31.,193.693575034635));
#56587=CARTESIAN_POINT('',(48.5,31.,193.693575034635));
#56588=CARTESIAN_POINT('',(-48.5,-31.,193.693575034635));
#56589=CARTESIAN_POINT('',(48.5,-31.,193.693575034635));
#56590=CARTESIAN_POINT('',(-48.5,-62.,140.));
#56591=CARTESIAN_POINT('',(48.5,-62.,140.));
#56592=CARTESIAN_POINT('',(-48.5,-31.,86.3064249653648));
#56593=CARTESIAN_POINT('',(48.5,-31.,86.3064249653648));
#56594=CARTESIAN_POINT('',(-48.5,31.,86.3064249653648));
#56595=CARTESIAN_POINT('',(48.5,31.,86.3064249653648));
#56596=UNCERTAINTY_MEASURE_WITH_UNIT(LENGTH_MEASURE(0.01),#56640,
'DISTANCE_ACCURACY_VALUE',
'Maximum model space distance between geometric entities at asserted c
onnectivities');
#56597=UNCERTAINTY_MEASURE_WITH_UNIT(LENGTH_MEASURE(0.01),#56640,
'DISTANCE_ACCURACY_VALUE',
'Maximum model space distance between geometric entities at asserted c
onnectivities');
#56598=UNCERTAINTY_MEASURE_WITH_UNIT(LENGTH_MEASURE(0.01),#56640,
'DISTANCE_ACCURACY_VALUE',
'Maximum model space distance between geometric entities at asserted c
onnectivities');
#56599=UNCERTAINTY_MEASURE_WITH_UNIT(LENGTH_MEASURE(0.01),#56640,
'DISTANCE_ACCURACY_VALUE',
'Maximum model space distance between geometric entities at asserted c
onnectivities');
#56600=UNCERTAINTY_MEASURE_WITH_UNIT(LENGTH_MEASURE(0.01),#56640,
'DISTANCE_ACCURACY_VALUE',
'Maximum model space distance between geometric entities at asserted c
onnectivities');
#56601=UNCERTAINTY_MEASURE_WITH_UNIT(LENGTH_MEASURE(0.01),#56640,
'DISTANCE_ACCURACY_VALUE',
'Maximum model space distance between geometric entities at asserted c
onnectivities');
#56602=UNCERTAINTY_MEASURE_WITH_UNIT(LENGTH_MEASURE(0.01),#56640,
'DISTANCE_ACCURACY_VALUE',
'Maximum model space distance between geometric entities at asserted c
onnectivities');
#56603=UNCERTAINTY_MEASURE_WITH_UNIT(LENGTH_MEASURE(0.01),#56640,
'DISTANCE_ACCURACY_VALUE',
'Maximum model space distance between geometric entities at asserted c
onnectivities');
#56604=UNCERTAINTY_MEASURE_WITH_UNIT(LENGTH_MEASURE(0.01),#56640,
'DISTANCE_ACCURACY_VALUE',
'Maximum model space distance between geometric entities at asserted c
onnectivities');
#56605=UNCERTAINTY_MEASURE_WITH_UNIT(LENGTH_MEASURE(0.01),#56640,
'DISTANCE_ACCURACY_VALUE',
'Maximum model space distance between geometric entities at asserted c
onnectivities');
#56606=UNCERTAINTY_MEASURE_WITH_UNIT(LENGTH_MEASURE(0.01),#56640,
'DISTANCE_ACCURACY_VALUE',
'Maximum model space distance between geometric entities at asserted c
onnectivities');
#56607=UNCERTAINTY_MEASURE_WITH_UNIT(LENGTH_MEASURE(0.01),#56640,
'DISTANCE_ACCURACY_VALUE',
'Maximum model space distance between geometric entities at asserted c
onnectivities');
#56608=UNCERTAINTY_MEASURE_WITH_UNIT(LENGTH_MEASURE(0.01),#56640,
'DISTANCE_ACCURACY_VALUE',
'Maximum model space distance between geometric entities at asserted c
onnectivities');
#56609=UNCERTAINTY_MEASURE_WITH_UNIT(LENGTH_MEASURE(0.01),#56640,
'DISTANCE_ACCURACY_VALUE',
'Maximum model space distance between geometric entities at asserted c
onnectivities');
#56610=UNCERTAINTY_MEASURE_WITH_UNIT(LENGTH_MEASURE(0.01),#56640,
'DISTANCE_ACCURACY_VALUE',
'Maximum model space distance between geometric entities at asserted c
onnectivities');
#56611=UNCERTAINTY_MEASURE_WITH_UNIT(LENGTH_MEASURE(0.01),#56640,
'DISTANCE_ACCURACY_VALUE',
'Maximum model space distance between geometric entities at asserted c
onnectivities');
#56612=UNCERTAINTY_MEASURE_WITH_UNIT(LENGTH_MEASURE(0.01),#56640,
'DISTANCE_ACCURACY_VALUE',
'Maximum model space distance between geometric entities at asserted c
onnectivities');
#56613=UNCERTAINTY_MEASURE_WITH_UNIT(LENGTH_MEASURE(0.01),#56640,
'DISTANCE_ACCURACY_VALUE',
'Maximum model space distance between geometric entities at asserted c
onnectivities');
#56614=UNCERTAINTY_MEASURE_WITH_UNIT(LENGTH_MEASURE(0.01),#56640,
'DISTANCE_ACCURACY_VALUE',
'Maximum model space distance between geometric entities at asserted c
onnectivities');
#56615=UNCERTAINTY_MEASURE_WITH_UNIT(LENGTH_MEASURE(0.01),#56640,
'DISTANCE_ACCURACY_VALUE',
'Maximum model space distance between geometric entities at asserted c
onnectivities');
#56616=UNCERTAINTY_MEASURE_WITH_UNIT(LENGTH_MEASURE(0.01),#56640,
'DISTANCE_ACCURACY_VALUE',
'Maximum model space distance between geometric entities at asserted c
onnectivities');
#56617=UNCERTAINTY_MEASURE_WITH_UNIT(LENGTH_MEASURE(0.01),#56640,
'DISTANCE_ACCURACY_VALUE',
'Maximum model space distance between geometric entities at asserted c
onnectivities');
#56618=(
GEOMETRIC_REPRESENTATION_CONTEXT(3)
GLOBAL_UNCERTAINTY_ASSIGNED_CONTEXT((#56596))
GLOBAL_UNIT_ASSIGNED_CONTEXT((#56640,#56642,#56643))
REPRESENTATION_CONTEXT('','3D')
);
#56619=(
GEOMETRIC_REPRESENTATION_CONTEXT(3)
GLOBAL_UNCERTAINTY_ASSIGNED_CONTEXT((#56597))
GLOBAL_UNIT_ASSIGNED_CONTEXT((#56640,#56642,#56643))
REPRESENTATION_CONTEXT('','3D')
);
#56620=(
GEOMETRIC_REPRESENTATION_CONTEXT(3)
GLOBAL_UNCERTAINTY_ASSIGNED_CONTEXT((#56598))
GLOBAL_UNIT_ASSIGNED_CONTEXT((#56640,#56642,#56643))
REPRESENTATION_CONTEXT('','3D')
);
#56621=(
GEOMETRIC_REPRESENTATION_CONTEXT(3)
GLOBAL_UNCERTAINTY_ASSIGNED_CONTEXT((#56599))
GLOBAL_UNIT_ASSIGNED_CONTEXT((#56640,#56642,#56643))
REPRESENTATION_CONTEXT('','3D')
);
#56622=(
GEOMETRIC_REPRESENTATION_CONTEXT(3)
GLOBAL_UNCERTAINTY_ASSIGNED_CONTEXT((#56600))
GLOBAL_UNIT_ASSIGNED_CONTEXT((#56640,#56642,#56643))
REPRESENTATION_CONTEXT('','3D')
);
#56623=(
GEOMETRIC_REPRESENTATION_CONTEXT(3)
GLOBAL_UNCERTAINTY_ASSIGNED_CONTEXT((#56601))
GLOBAL_UNIT_ASSIGNED_CONTEXT((#56640,#56642,#56643))
REPRESENTATION_CONTEXT('','3D')
);
#56624=(
GEOMETRIC_REPRESENTATION_CONTEXT(3)
GLOBAL_UNCERTAINTY_ASSIGNED_CONTEXT((#56602))
GLOBAL_UNIT_ASSIGNED_CONTEXT((#56640,#56642,#56643))
REPRESENTATION_CONTEXT('','3D')
);
#56625=(
GEOMETRIC_REPRESENTATION_CONTEXT(3)
GLOBAL_UNCERTAINTY_ASSIGNED_CONTEXT((#56603))
GLOBAL_UNIT_ASSIGNED_CONTEXT((#56640,#56642,#56643))
REPRESENTATION_CONTEXT('','3D')
);
#56626=(
GEOMETRIC_REPRESENTATION_CONTEXT(3)
GLOBAL_UNCERTAINTY_ASSIGNED_CONTEXT((#56604))
GLOBAL_UNIT_ASSIGNED_CONTEXT((#56640,#56642,#56643))
REPRESENTATION_CONTEXT('','3D')
);
#56627=(
GEOMETRIC_REPRESENTATION_CONTEXT(3)
GLOBAL_UNCERTAINTY_ASSIGNED_CONTEXT((#56605))
GLOBAL_UNIT_ASSIGNED_CONTEXT((#56640,#56642,#56643))
REPRESENTATION_CONTEXT('','3D')
);
#56628=(
GEOMETRIC_REPRESENTATION_CONTEXT(3)
GLOBAL_UNCERTAINTY_ASSIGNED_CONTEXT((#56606))
GLOBAL_UNIT_ASSIGNED_CONTEXT((#56640,#56642,#56643))
REPRESENTATION_CONTEXT('','3D')
);
#56629=(
GEOMETRIC_REPRESENTATION_CONTEXT(3)
GLOBAL_UNCERTAINTY_ASSIGNED_CONTEXT((#56607))
GLOBAL_UNIT_ASSIGNED_CONTEXT((#56640,#56642,#56643))
REPRESENTATION_CONTEXT('','3D')
);
#56630=(
GEOMETRIC_REPRESENTATION_CONTEXT(3)
GLOBAL_UNCERTAINTY_ASSIGNED_CONTEXT((#56608))
GLOBAL_UNIT_ASSIGNED_CONTEXT((#56640,#56642,#56643))
REPRESENTATION_CONTEXT('','3D')
);
#56631=(
GEOMETRIC_REPRESENTATION_CONTEXT(3)
GLOBAL_UNCERTAINTY_ASSIGNED_CONTEXT((#56609))
GLOBAL_UNIT_ASSIGNED_CONTEXT((#56640,#56642,#56643))
REPRESENTATION_CONTEXT('','3D')
);
#56632=(
GEOMETRIC_REPRESENTATION_CONTEXT(3)
GLOBAL_UNCERTAINTY_ASSIGNED_CONTEXT((#56610))
GLOBAL_UNIT_ASSIGNED_CONTEXT((#56640,#56642,#56643))
REPRESENTATION_CONTEXT('','3D')
);
#56633=(
GEOMETRIC_REPRESENTATION_CONTEXT(3)
GLOBAL_UNCERTAINTY_ASSIGNED_CONTEXT((#56611))
GLOBAL_UNIT_ASSIGNED_CONTEXT((#56640,#56642,#56643))
REPRESENTATION_CONTEXT('','3D')
);
#56634=(
GEOMETRIC_REPRESENTATION_CONTEXT(3)
GLOBAL_UNCERTAINTY_ASSIGNED_CONTEXT((#56612))
GLOBAL_UNIT_ASSIGNED_CONTEXT((#56640,#56642,#56643))
REPRESENTATION_CONTEXT('','3D')
);
#56635=(
GEOMETRIC_REPRESENTATION_CONTEXT(3)
GLOBAL_UNCERTAINTY_ASSIGNED_CONTEXT((#56613))
GLOBAL_UNIT_ASSIGNED_CONTEXT((#56640,#56642,#56643))
REPRESENTATION_CONTEXT('','3D')
);
#56636=(
GEOMETRIC_REPRESENTATION_CONTEXT(3)
GLOBAL_UNCERTAINTY_ASSIGNED_CONTEXT((#56614))
GLOBAL_UNIT_ASSIGNED_CONTEXT((#56640,#56642,#56643))
REPRESENTATION_CONTEXT('','3D')
);
#56637=(
GEOMETRIC_REPRESENTATION_CONTEXT(3)
GLOBAL_UNCERTAINTY_ASSIGNED_CONTEXT((#56615))
GLOBAL_UNIT_ASSIGNED_CONTEXT((#56640,#56642,#56643))
REPRESENTATION_CONTEXT('','3D')
);
#56638=(
GEOMETRIC_REPRESENTATION_CONTEXT(3)
GLOBAL_UNCERTAINTY_ASSIGNED_CONTEXT((#56616))
GLOBAL_UNIT_ASSIGNED_CONTEXT((#56640,#56642,#56643))
REPRESENTATION_CONTEXT('','3D')
);
#56639=(
GEOMETRIC_REPRESENTATION_CONTEXT(3)
GLOBAL_UNCERTAINTY_ASSIGNED_CONTEXT((#56617))
GLOBAL_UNIT_ASSIGNED_CONTEXT((#56640,#56642,#56643))
REPRESENTATION_CONTEXT('','3D')
);
#56640=(
LENGTH_UNIT()
NAMED_UNIT(*)
SI_UNIT(.MILLI.,.METRE.)
);
#56641=(
LENGTH_UNIT()
NAMED_UNIT(*)
SI_UNIT($,.METRE.)
);
#56642=(
NAMED_UNIT(*)
PLANE_ANGLE_UNIT()
SI_UNIT($,.RADIAN.)
);
#56643=(
NAMED_UNIT(*)
SI_UNIT($,.STERADIAN.)
SOLID_ANGLE_UNIT()
);
#56644=SHAPE_DEFINITION_REPRESENTATION(#56665,#56744);
#56645=SHAPE_DEFINITION_REPRESENTATION(#56666,#56745);
#56646=SHAPE_DEFINITION_REPRESENTATION(#56667,#56746);
#56647=SHAPE_DEFINITION_REPRESENTATION(#56668,#56747);
#56648=SHAPE_DEFINITION_REPRESENTATION(#56669,#56748);
#56649=SHAPE_DEFINITION_REPRESENTATION(#56670,#56749);
#56650=SHAPE_DEFINITION_REPRESENTATION(#56671,#56750);
#56651=SHAPE_DEFINITION_REPRESENTATION(#56672,#56751);
#56652=SHAPE_DEFINITION_REPRESENTATION(#56673,#56752);
#56653=SHAPE_DEFINITION_REPRESENTATION(#56674,#56753);
#56654=SHAPE_DEFINITION_REPRESENTATION(#56675,#56754);
#56655=SHAPE_DEFINITION_REPRESENTATION(#56676,#56755);
#56656=SHAPE_DEFINITION_REPRESENTATION(#56677,#56756);
#56657=SHAPE_DEFINITION_REPRESENTATION(#56678,#56757);
#56658=SHAPE_DEFINITION_REPRESENTATION(#56679,#56758);
#56659=SHAPE_DEFINITION_REPRESENTATION(#56680,#56759);
#56660=SHAPE_DEFINITION_REPRESENTATION(#56681,#56760);
#56661=SHAPE_DEFINITION_REPRESENTATION(#56682,#56761);
#56662=SHAPE_DEFINITION_REPRESENTATION(#56683,#56762);
#56663=SHAPE_DEFINITION_REPRESENTATION(#56684,#56763);
#56664=SHAPE_DEFINITION_REPRESENTATION(#56685,#56764);
#56665=PRODUCT_DEFINITION_SHAPE('',$,#56766);
#56666=PRODUCT_DEFINITION_SHAPE('',$,#56767);
#56667=PRODUCT_DEFINITION_SHAPE('',$,#56768);
#56668=PRODUCT_DEFINITION_SHAPE('',$,#56769);
#56669=PRODUCT_DEFINITION_SHAPE('',$,#56770);
#56670=PRODUCT_DEFINITION_SHAPE('',$,#56771);
#56671=PRODUCT_DEFINITION_SHAPE('',$,#56772);
#56672=PRODUCT_DEFINITION_SHAPE('',$,#56773);
#56673=PRODUCT_DEFINITION_SHAPE('',$,#56774);
#56674=PRODUCT_DEFINITION_SHAPE('',$,#56775);
#56675=PRODUCT_DEFINITION_SHAPE('',$,#56776);
#56676=PRODUCT_DEFINITION_SHAPE('',$,#56777);
#56677=PRODUCT_DEFINITION_SHAPE('',$,#56778);
#56678=PRODUCT_DEFINITION_SHAPE('',$,#56779);
#56679=PRODUCT_DEFINITION_SHAPE('',$,#56780);
#56680=PRODUCT_DEFINITION_SHAPE('',$,#56781);
#56681=PRODUCT_DEFINITION_SHAPE('',$,#56782);
#56682=PRODUCT_DEFINITION_SHAPE('',$,#56783);
#56683=PRODUCT_DEFINITION_SHAPE('',$,#56784);
#56684=PRODUCT_DEFINITION_SHAPE('',$,#56785);
#56685=PRODUCT_DEFINITION_SHAPE('',$,#56786);
#56686=PRODUCT_DEFINITION_SHAPE($,$,#185);
#56687=PRODUCT_DEFINITION_SHAPE($,$,#186);
#56688=PRODUCT_DEFINITION_SHAPE($,$,#187);
#56689=PRODUCT_DEFINITION_SHAPE($,$,#188);
#56690=PRODUCT_DEFINITION_SHAPE($,$,#189);
#56691=PRODUCT_DEFINITION_SHAPE($,$,#190);
#56692=PRODUCT_DEFINITION_SHAPE($,$,#191);
#56693=PRODUCT_DEFINITION_SHAPE($,$,#192);
#56694=PRODUCT_DEFINITION_SHAPE($,$,#193);
#56695=PRODUCT_DEFINITION_SHAPE($,$,#194);
#56696=PRODUCT_DEFINITION_SHAPE($,$,#195);
#56697=PRODUCT_DEFINITION_SHAPE($,$,#196);
#56698=PRODUCT_DEFINITION_SHAPE($,$,#197);
#56699=PRODUCT_DEFINITION_SHAPE($,$,#198);
#56700=PRODUCT_DEFINITION_SHAPE($,$,#199);
#56701=PRODUCT_DEFINITION_SHAPE($,$,#200);
#56702=PRODUCT_DEFINITION_SHAPE($,$,#201);
#56703=PRODUCT_DEFINITION_SHAPE($,$,#202);
#56704=PRODUCT_DEFINITION_SHAPE($,$,#203);
#56705=PRODUCT_DEFINITION_SHAPE($,$,#204);
#56706=PRODUCT_DEFINITION_SHAPE($,$,#205);
#56707=PRODUCT_DEFINITION_SHAPE($,$,#206);
#56708=PRODUCT_DEFINITION_SHAPE($,$,#207);
#56709=PRODUCT_DEFINITION_SHAPE($,$,#208);
#56710=PRODUCT_DEFINITION_SHAPE($,$,#209);
#56711=PRODUCT_DEFINITION_SHAPE($,$,#210);
#56712=PRODUCT_DEFINITION_SHAPE($,$,#211);
#56713=PRODUCT_DEFINITION_SHAPE($,$,#212);
#56714=PRODUCT_DEFINITION_SHAPE($,$,#213);
#56715=PRODUCT_DEFINITION_SHAPE($,$,#214);
#56716=PRODUCT_DEFINITION_SHAPE($,$,#215);
#56717=PRODUCT_DEFINITION_SHAPE($,$,#216);
#56718=PRODUCT_DEFINITION_SHAPE($,$,#217);
#56719=PRODUCT_DEFINITION_SHAPE($,$,#218);
#56720=PRODUCT_DEFINITION_SHAPE($,$,#219);
#56721=PRODUCT_DEFINITION_SHAPE($,$,#220);
#56722=PRODUCT_DEFINITION_SHAPE($,$,#221);
#56723=PRODUCT_DEFINITION_SHAPE($,$,#222);
#56724=PRODUCT_DEFINITION_SHAPE($,$,#223);
#56725=PRODUCT_DEFINITION_SHAPE($,$,#224);
#56726=PRODUCT_DEFINITION_SHAPE($,$,#225);
#56727=PRODUCT_DEFINITION_SHAPE($,$,#226);
#56728=PRODUCT_DEFINITION_SHAPE($,$,#227);
#56729=PRODUCT_DEFINITION_SHAPE($,$,#228);
#56730=PRODUCT_DEFINITION_SHAPE($,$,#229);
#56731=PRODUCT_DEFINITION_SHAPE($,$,#230);
#56732=PRODUCT_DEFINITION_SHAPE($,$,#231);
#56733=PRODUCT_DEFINITION_SHAPE($,$,#232);
#56734=PRODUCT_DEFINITION_SHAPE($,$,#233);
#56735=PRODUCT_DEFINITION_SHAPE($,$,#234);
#56736=PRODUCT_DEFINITION_SHAPE($,$,#235);
#56737=PRODUCT_DEFINITION_SHAPE($,$,#236);
#56738=PRODUCT_DEFINITION_SHAPE($,$,#237);
#56739=PRODUCT_DEFINITION_SHAPE($,$,#238);
#56740=PRODUCT_DEFINITION_SHAPE($,$,#239);
#56741=PRODUCT_DEFINITION_SHAPE($,$,#240);
#56742=PRODUCT_DEFINITION_SHAPE($,$,#241);
#56743=PRODUCT_DEFINITION_SHAPE($,$,#242);
#56744=SHAPE_REPRESENTATION('',(#17190,#18731,#18732,#18733,#18734,#18735,
#18736,#18737,#18738,#18739,#18740,#18741,#18742,#18743,#18744,#18745,#18746,
#18747,#18748,#18749,#18750,#18751,#18752,#18753,#18754,#18755,#18756,#18757,
#18758,#18759,#18760,#18761,#18762,#18763,#18764,#18765,#18766,#18767,#18768,
#18769,#18770,#18771,#18772,#18773,#18774,#18775,#18776,#18777,#18778,#18779,
#18780,#18781,#18782,#18783,#18784,#18785,#18786,#18787,#18788),#56618);
#56745=SHAPE_REPRESENTATION('',(#17191),#56619);
#56746=SHAPE_REPRESENTATION('',(#17485),#56620);
#56747=SHAPE_REPRESENTATION('',(#17536),#56621);
#56748=SHAPE_REPRESENTATION('',(#17588),#56622);
#56749=SHAPE_REPRESENTATION('',(#17615),#56623);
#56750=SHAPE_REPRESENTATION('',(#17650),#56624);
#56751=SHAPE_REPRESENTATION('',(#17664),#56625);
#56752=SHAPE_REPRESENTATION('',(#17684),#56626);
#56753=SHAPE_REPRESENTATION('',(#17774),#56627);
#56754=SHAPE_REPRESENTATION('',(#17818),#56628);
#56755=SHAPE_REPRESENTATION('',(#18010),#56629);
#56756=SHAPE_REPRESENTATION('',(#18066),#56630);
#56757=SHAPE_REPRESENTATION('',(#18137),#56631);
#56758=SHAPE_REPRESENTATION('',(#18202),#56632);
#56759=SHAPE_REPRESENTATION('',(#18205),#56633);
#56760=SHAPE_REPRESENTATION('',(#18218),#56634);
#56761=SHAPE_REPRESENTATION('',(#18327),#56635);
#56762=SHAPE_REPRESENTATION('',(#18375),#56636);
#56763=SHAPE_REPRESENTATION('',(#18487),#56637);
#56764=SHAPE_REPRESENTATION('',(#18687),#56638);
#56765=PRODUCT_DEFINITION_CONTEXT('part definition',#56830,'design');
#56766=PRODUCT_DEFINITION('2026-10-26-00-02-34-865','MAS-343',#56787,#56765);
#56767=PRODUCT_DEFINITION('2026-10-26-00-02-35-941',
'01_Out_Chamber_ADC12',#56788,#56765);
#56768=PRODUCT_DEFINITION('2026-10-26-00-02-39-148',
'02_Center_Body_A_Air_Inlet',#56789,#56765);
#56769=PRODUCT_DEFINITION('2026-10-26-00-02-39-940',
'03_Center_Body_B_Exhaust',#56790,#56765);
#56770=PRODUCT_DEFINITION('2026-10-26-00-02-40-929','04_Body_Gasket',#56791,
#56765);
#56771=PRODUCT_DEFINITION('2026-10-26-00-02-41-508','05_Diaphragm_TPEE',
#56792,#56765);
#56772=PRODUCT_DEFINITION('2026-10-26-00-02-42-220',
'06_Inner_Center_Disk',#56793,#56765);
#56773=PRODUCT_DEFINITION('2026-10-26-00-02-42-500',
'07_Outer_Center_Disk',#56794,#56765);
#56774=PRODUCT_DEFINITION('2026-10-26-00-02-42-773',
'08_Center_Rod_D16_M10',#56795,#56765);
#56775=PRODUCT_DEFINITION('2026-10-26-00-02-43-431',
'09_Hex_Nut_ISO_4032_M10',#56796,#56765);
#56776=PRODUCT_DEFINITION('2026-10-26-00-02-44-429','10_Manifold',#56797,
#56765);
#56777=PRODUCT_DEFINITION('2026-10-26-00-02-49-069',
'11_Manifold_End_Cap_M24x1.5',#56798,#56765);
#56778=PRODUCT_DEFINITION('2026-10-26-00-02-57-738',
'19_Air_Inlet_Ball_Valve_1-4',#56799,#56765);
#56779=PRODUCT_DEFINITION('2026-10-26-00-03-01-283',
'20_Exhaust_Silencer_3-8',#56800,#56765);
#56780=PRODUCT_DEFINITION('2026-10-26-00-02-50-076',
'12_Check_Ball_D16_TPEE',#56801,#56765);
#56781=PRODUCT_DEFINITION('2026-10-26-00-02-50-406',
'13_Valve_Seat_26x12x6',#56802,#56765);
#56782=PRODUCT_DEFINITION('2026-10-26-00-02-50-838','14_Base_Channel',#56803,
#56765);
#56783=PRODUCT_DEFINITION('2026-10-26-00-02-52-418',
'15_Cushion_Foot_M8',#56804,#56765);
#56784=PRODUCT_DEFINITION('2026-10-26-00-02-56-247',
'18_Manifold_Bolt_ISO_4017_M8x55',#56805,#56765);
#56785=PRODUCT_DEFINITION('2026-10-26-00-02-53-145',
'16_Tie_Bolt_M8x110_ISO_4017_Hex_Head',#56806,#56765);
#56786=PRODUCT_DEFINITION('2026-10-26-00-02-54-694',
'17_Hex_Nut_ISO_4032_M8',#56807,#56765);
#56787=PRODUCT_DEFINITION_FORMATION('',$,#56832);
#56788=PRODUCT_DEFINITION_FORMATION('',$,#56833);
#56789=PRODUCT_DEFINITION_FORMATION('',$,#56834);
#56790=PRODUCT_DEFINITION_FORMATION('',$,#56835);
#56791=PRODUCT_DEFINITION_FORMATION('',$,#56836);
#56792=PRODUCT_DEFINITION_FORMATION('',$,#56837);
#56793=PRODUCT_DEFINITION_FORMATION('',$,#56838);
#56794=PRODUCT_DEFINITION_FORMATION('',$,#56839);
#56795=PRODUCT_DEFINITION_FORMATION('',$,#56840);
#56796=PRODUCT_DEFINITION_FORMATION('',$,#56841);
#56797=PRODUCT_DEFINITION_FORMATION('',$,#56842);
#56798=PRODUCT_DEFINITION_FORMATION('',$,#56843);
#56799=PRODUCT_DEFINITION_FORMATION('',$,#56844);
#56800=PRODUCT_DEFINITION_FORMATION('',$,#56845);
#56801=PRODUCT_DEFINITION_FORMATION('',$,#56846);
#56802=PRODUCT_DEFINITION_FORMATION('',$,#56847);
#56803=PRODUCT_DEFINITION_FORMATION('',$,#56848);
#56804=PRODUCT_DEFINITION_FORMATION('',$,#56849);
#56805=PRODUCT_DEFINITION_FORMATION('',$,#56850);
#56806=PRODUCT_DEFINITION_FORMATION('',$,#56851);
#56807=PRODUCT_DEFINITION_FORMATION('',$,#56852);
#56808=PRODUCT_RELATED_PRODUCT_CATEGORY('MAS-343','MAS-343',(#56832));
#56809=PRODUCT_RELATED_PRODUCT_CATEGORY('01_Out_Chamber_ADC12',
'01_Out_Chamber_ADC12',(#56833));
#56810=PRODUCT_RELATED_PRODUCT_CATEGORY('02_Center_Body_A_Air_Inlet',
'02_Center_Body_A_Air_Inlet',(#56834));
#56811=PRODUCT_RELATED_PRODUCT_CATEGORY('03_Center_Body_B_Exhaust',
'03_Center_Body_B_Exhaust',(#56835));
#56812=PRODUCT_RELATED_PRODUCT_CATEGORY('04_Body_Gasket',
'04_Body_Gasket',(#56836));
#56813=PRODUCT_RELATED_PRODUCT_CATEGORY('05_Diaphragm_TPEE',
'05_Diaphragm_TPEE',(#56837));
#56814=PRODUCT_RELATED_PRODUCT_CATEGORY('06_Inner_Center_Disk',
'06_Inner_Center_Disk',(#56838));
#56815=PRODUCT_RELATED_PRODUCT_CATEGORY('07_Outer_Center_Disk',
'07_Outer_Center_Disk',(#56839));
#56816=PRODUCT_RELATED_PRODUCT_CATEGORY('08_Center_Rod_D16_M10',
'08_Center_Rod_D16_M10',(#56840));
#56817=PRODUCT_RELATED_PRODUCT_CATEGORY('09_Hex_Nut_ISO_4032_M10',
'09_Hex_Nut_ISO_4032_M10',(#56841));
#56818=PRODUCT_RELATED_PRODUCT_CATEGORY('10_Manifold','10_Manifold',(#56842));
#56819=PRODUCT_RELATED_PRODUCT_CATEGORY('11_Manifold_End_Cap_M24x1.5',
'11_Manifold_End_Cap_M24x1.5',(#56843));
#56820=PRODUCT_RELATED_PRODUCT_CATEGORY('19_Air_Inlet_Ball_Valve_1-4',
'19_Air_Inlet_Ball_Valve_1-4',(#56844));
#56821=PRODUCT_RELATED_PRODUCT_CATEGORY('20_Exhaust_Silencer_3-8',
'20_Exhaust_Silencer_3-8',(#56845));
#56822=PRODUCT_RELATED_PRODUCT_CATEGORY('12_Check_Ball_D16_TPEE',
'12_Check_Ball_D16_TPEE',(#56846));
#56823=PRODUCT_RELATED_PRODUCT_CATEGORY('13_Valve_Seat_26x12x6',
'13_Valve_Seat_26x12x6',(#56847));
#56824=PRODUCT_RELATED_PRODUCT_CATEGORY('14_Base_Channel',
'14_Base_Channel',(#56848));
#56825=PRODUCT_RELATED_PRODUCT_CATEGORY('15_Cushion_Foot_M8',
'15_Cushion_Foot_M8',(#56849));
#56826=PRODUCT_RELATED_PRODUCT_CATEGORY(
'18_Manifold_Bolt_ISO_4017_M8x55','18_Manifold_Bolt_ISO_4017_M8x55',(#56850));
#56827=PRODUCT_RELATED_PRODUCT_CATEGORY(
'16_Tie_Bolt_M8x110_ISO_4017_Hex_Head',
'16_Tie_Bolt_M8x110_ISO_4017_Hex_Head',(#56851));
#56828=PRODUCT_RELATED_PRODUCT_CATEGORY('17_Hex_Nut_ISO_4032_M8',
'17_Hex_Nut_ISO_4032_M8',(#56852));
#56829=APPLICATION_PROTOCOL_DEFINITION('international standard',
'automotive_design',2009,#56830);
#56830=APPLICATION_CONTEXT(
'Core Data for Automotive Mechanical Design Process');
#56831=PRODUCT_CONTEXT('part definition',#56830,'mechanical');
#56832=PRODUCT('2026-10-26-00-02-34-865','MAS-343',$,(#56831));
#56833=PRODUCT('2026-10-26-00-02-35-941','01_Out_Chamber_ADC12',$,(#56831));
#56834=PRODUCT('2026-10-26-00-02-39-148','02_Center_Body_A_Air_Inlet',$,
(#56831));
#56835=PRODUCT('2026-10-26-00-02-39-940','03_Center_Body_B_Exhaust',$,(#56831));
#56836=PRODUCT('2026-10-26-00-02-40-929','04_Body_Gasket',$,(#56831));
#56837=PRODUCT('2026-10-26-00-02-41-508','05_Diaphragm_TPEE',$,(#56831));
#56838=PRODUCT('2026-10-26-00-02-42-220','06_Inner_Center_Disk',$,(#56831));
#56839=PRODUCT('2026-10-26-00-02-42-500','07_Outer_Center_Disk',$,(#56831));
#56840=PRODUCT('2026-10-26-00-02-42-773','08_Center_Rod_D16_M10',$,(#56831));
#56841=PRODUCT('2026-10-26-00-02-43-431','09_Hex_Nut_ISO_4032_M10',$,(#56831));
#56842=PRODUCT('2026-10-26-00-02-44-429','10_Manifold',$,(#56831));
#56843=PRODUCT('2026-10-26-00-02-49-069','11_Manifold_End_Cap_M24x1.5',
$,(#56831));
#56844=PRODUCT('2026-10-26-00-02-57-738','19_Air_Inlet_Ball_Valve_1-4',
$,(#56831));
#56845=PRODUCT('2026-10-26-00-03-01-283','20_Exhaust_Silencer_3-8',$,(#56831));
#56846=PRODUCT('2026-10-26-00-02-50-076','12_Check_Ball_D16_TPEE',$,(#56831));
#56847=PRODUCT('2026-10-26-00-02-50-406','13_Valve_Seat_26x12x6',$,(#56831));
#56848=PRODUCT('2026-10-26-00-02-50-838','14_Base_Channel',$,(#56831));
#56849=PRODUCT('2026-10-26-00-02-52-418','15_Cushion_Foot_M8',$,(#56831));
#56850=PRODUCT('2026-10-26-00-02-56-247',
'18_Manifold_Bolt_ISO_4017_M8x55',$,(#56831));
#56851=PRODUCT('2026-10-26-00-02-53-145',
'16_Tie_Bolt_M8x110_ISO_4017_Hex_Head',$,(#56831));
#56852=PRODUCT('2026-10-26-00-02-54-694','17_Hex_Nut_ISO_4032_M8',$,(#56831));
#56853=PRESENTATION_STYLE_ASSIGNMENT((#56858));
#56854=PRESENTATION_STYLE_ASSIGNMENT((#56859));
#56855=PRESENTATION_STYLE_ASSIGNMENT((#56860));
#56856=PRESENTATION_STYLE_ASSIGNMENT((#56861));
#56857=PRESENTATION_STYLE_ASSIGNMENT((#56862));
#56858=SURFACE_STYLE_USAGE(.BOTH.,#56863);
#56859=SURFACE_STYLE_USAGE(.BOTH.,#56864);
#56860=SURFACE_STYLE_USAGE(.BOTH.,#56865);
#56861=SURFACE_STYLE_USAGE(.BOTH.,#56866);
#56862=SURFACE_STYLE_USAGE(.BOTH.,#56867);
#56863=SURFACE_SIDE_STYLE('',(#56868));
#56864=SURFACE_SIDE_STYLE('',(#56869));
#56865=SURFACE_SIDE_STYLE('',(#56870));
#56866=SURFACE_SIDE_STYLE('',(#56871));
#56867=SURFACE_SIDE_STYLE('',(#56872));
#56868=SURFACE_STYLE_FILL_AREA(#56873);
#56869=SURFACE_STYLE_FILL_AREA(#56874);
#56870=SURFACE_STYLE_FILL_AREA(#56875);
#56871=SURFACE_STYLE_FILL_AREA(#56876);
#56872=SURFACE_STYLE_FILL_AREA(#56877);
#56873=FILL_AREA_STYLE('Steel - Satin',(#56878));
#56874=FILL_AREA_STYLE('MAS496_al',(#56879));
#56875=FILL_AREA_STYLE('MAS496_gun',(#56880));
#56876=FILL_AREA_STYLE('MAS496_ss',(#56881));
#56877=FILL_AREA_STYLE('MAS496_ti',(#56882));
#56878=FILL_AREA_STYLE_COLOUR('Steel - Satin',#56883);
#56879=FILL_AREA_STYLE_COLOUR('MAS496_al',#56884);
#56880=FILL_AREA_STYLE_COLOUR('MAS496_gun',#56885);
#56881=FILL_AREA_STYLE_COLOUR('MAS496_ss',#56886);
#56882=FILL_AREA_STYLE_COLOUR('MAS496_ti',#56887);
#56883=COLOUR_RGB('Steel - Satin',0.627450980392157,0.627450980392157,0.627450980392157);
#56884=COLOUR_RGB('MAS496_al',0.67843137254902,0.705882352941177,0.729411764705882);
#56885=COLOUR_RGB('MAS496_gun',0.313725490196078,0.337254901960784,0.364705882352941);
#56886=COLOUR_RGB('MAS496_ss',0.83921568627451,0.850980392156863,0.862745098039216);
#56887=COLOUR_RGB('MAS496_ti',0.549019607843137,0.572549019607843,0.596078431372549);
#56888=COLOUR_RGB('Dark Blue',0.08,0.2,0.34);
#56889=FILL_AREA_STYLE_COLOUR('',#56888);
#56890=FILL_AREA_STYLE('',(#56889));
#56891=SURFACE_STYLE_FILL_AREA(#56890);
#56892=SURFACE_SIDE_STYLE('',(#56891));
#56893=SURFACE_STYLE_USAGE(.BOTH.,#56892);
#56894=PRESENTATION_STYLE_ASSIGNMENT((#56893));
#56895=COLOUR_RGB('Light Blue',0.38,0.62,0.78);
#56896=FILL_AREA_STYLE_COLOUR('',#56895);
#56897=FILL_AREA_STYLE('',(#56896));
#56898=SURFACE_STYLE_FILL_AREA(#56897);
#56899=SURFACE_SIDE_STYLE('',(#56898));
#56900=SURFACE_STYLE_USAGE(.BOTH.,#56899);
#56901=PRESENTATION_STYLE_ASSIGNMENT((#56900));
#56902=COLOUR_RGB('Sky Blue',0.24,0.69,0.87);
#56903=FILL_AREA_STYLE_COLOUR('',#56902);
#56904=FILL_AREA_STYLE('',(#56903));
#56905=SURFACE_STYLE_FILL_AREA(#56904);
#56906=SURFACE_SIDE_STYLE('',(#56905));
#56907=SURFACE_STYLE_USAGE(.BOTH.,#56906);
#56908=PRESENTATION_STYLE_ASSIGNMENT((#56907));
#56909=COLOUR_RGB('Grey',0.48,0.52,0.57);
#56910=FILL_AREA_STYLE_COLOUR('',#56909);
#56911=FILL_AREA_STYLE('',(#56910));
#56912=SURFACE_STYLE_FILL_AREA(#56911);
#56913=SURFACE_SIDE_STYLE('',(#56912));
#56914=SURFACE_STYLE_USAGE(.BOTH.,#56913);
#56915=PRESENTATION_STYLE_ASSIGNMENT((#56914));
#56916=COLOUR_RGB('Black',0.12,0.14,0.17);
#56917=FILL_AREA_STYLE_COLOUR('',#56916);
#56918=FILL_AREA_STYLE('',(#56917));
#56919=SURFACE_STYLE_FILL_AREA(#56918);
#56920=SURFACE_SIDE_STYLE('',(#56919));
#56921=SURFACE_STYLE_USAGE(.BOTH.,#56920);
#56922=PRESENTATION_STYLE_ASSIGNMENT((#56921));
#56923=COLOUR_RGB('Off White',0.89,0.88,0.83);
#56924=FILL_AREA_STYLE_COLOUR('',#56923);
#56925=FILL_AREA_STYLE('',(#56924));
#56926=SURFACE_STYLE_FILL_AREA(#56925);
#56927=SURFACE_SIDE_STYLE('',(#56926));
#56928=SURFACE_STYLE_USAGE(.BOTH.,#56927);
#56929=PRESENTATION_STYLE_ASSIGNMENT((#56928));
ENDSEC;
END-ISO-10303-21;
